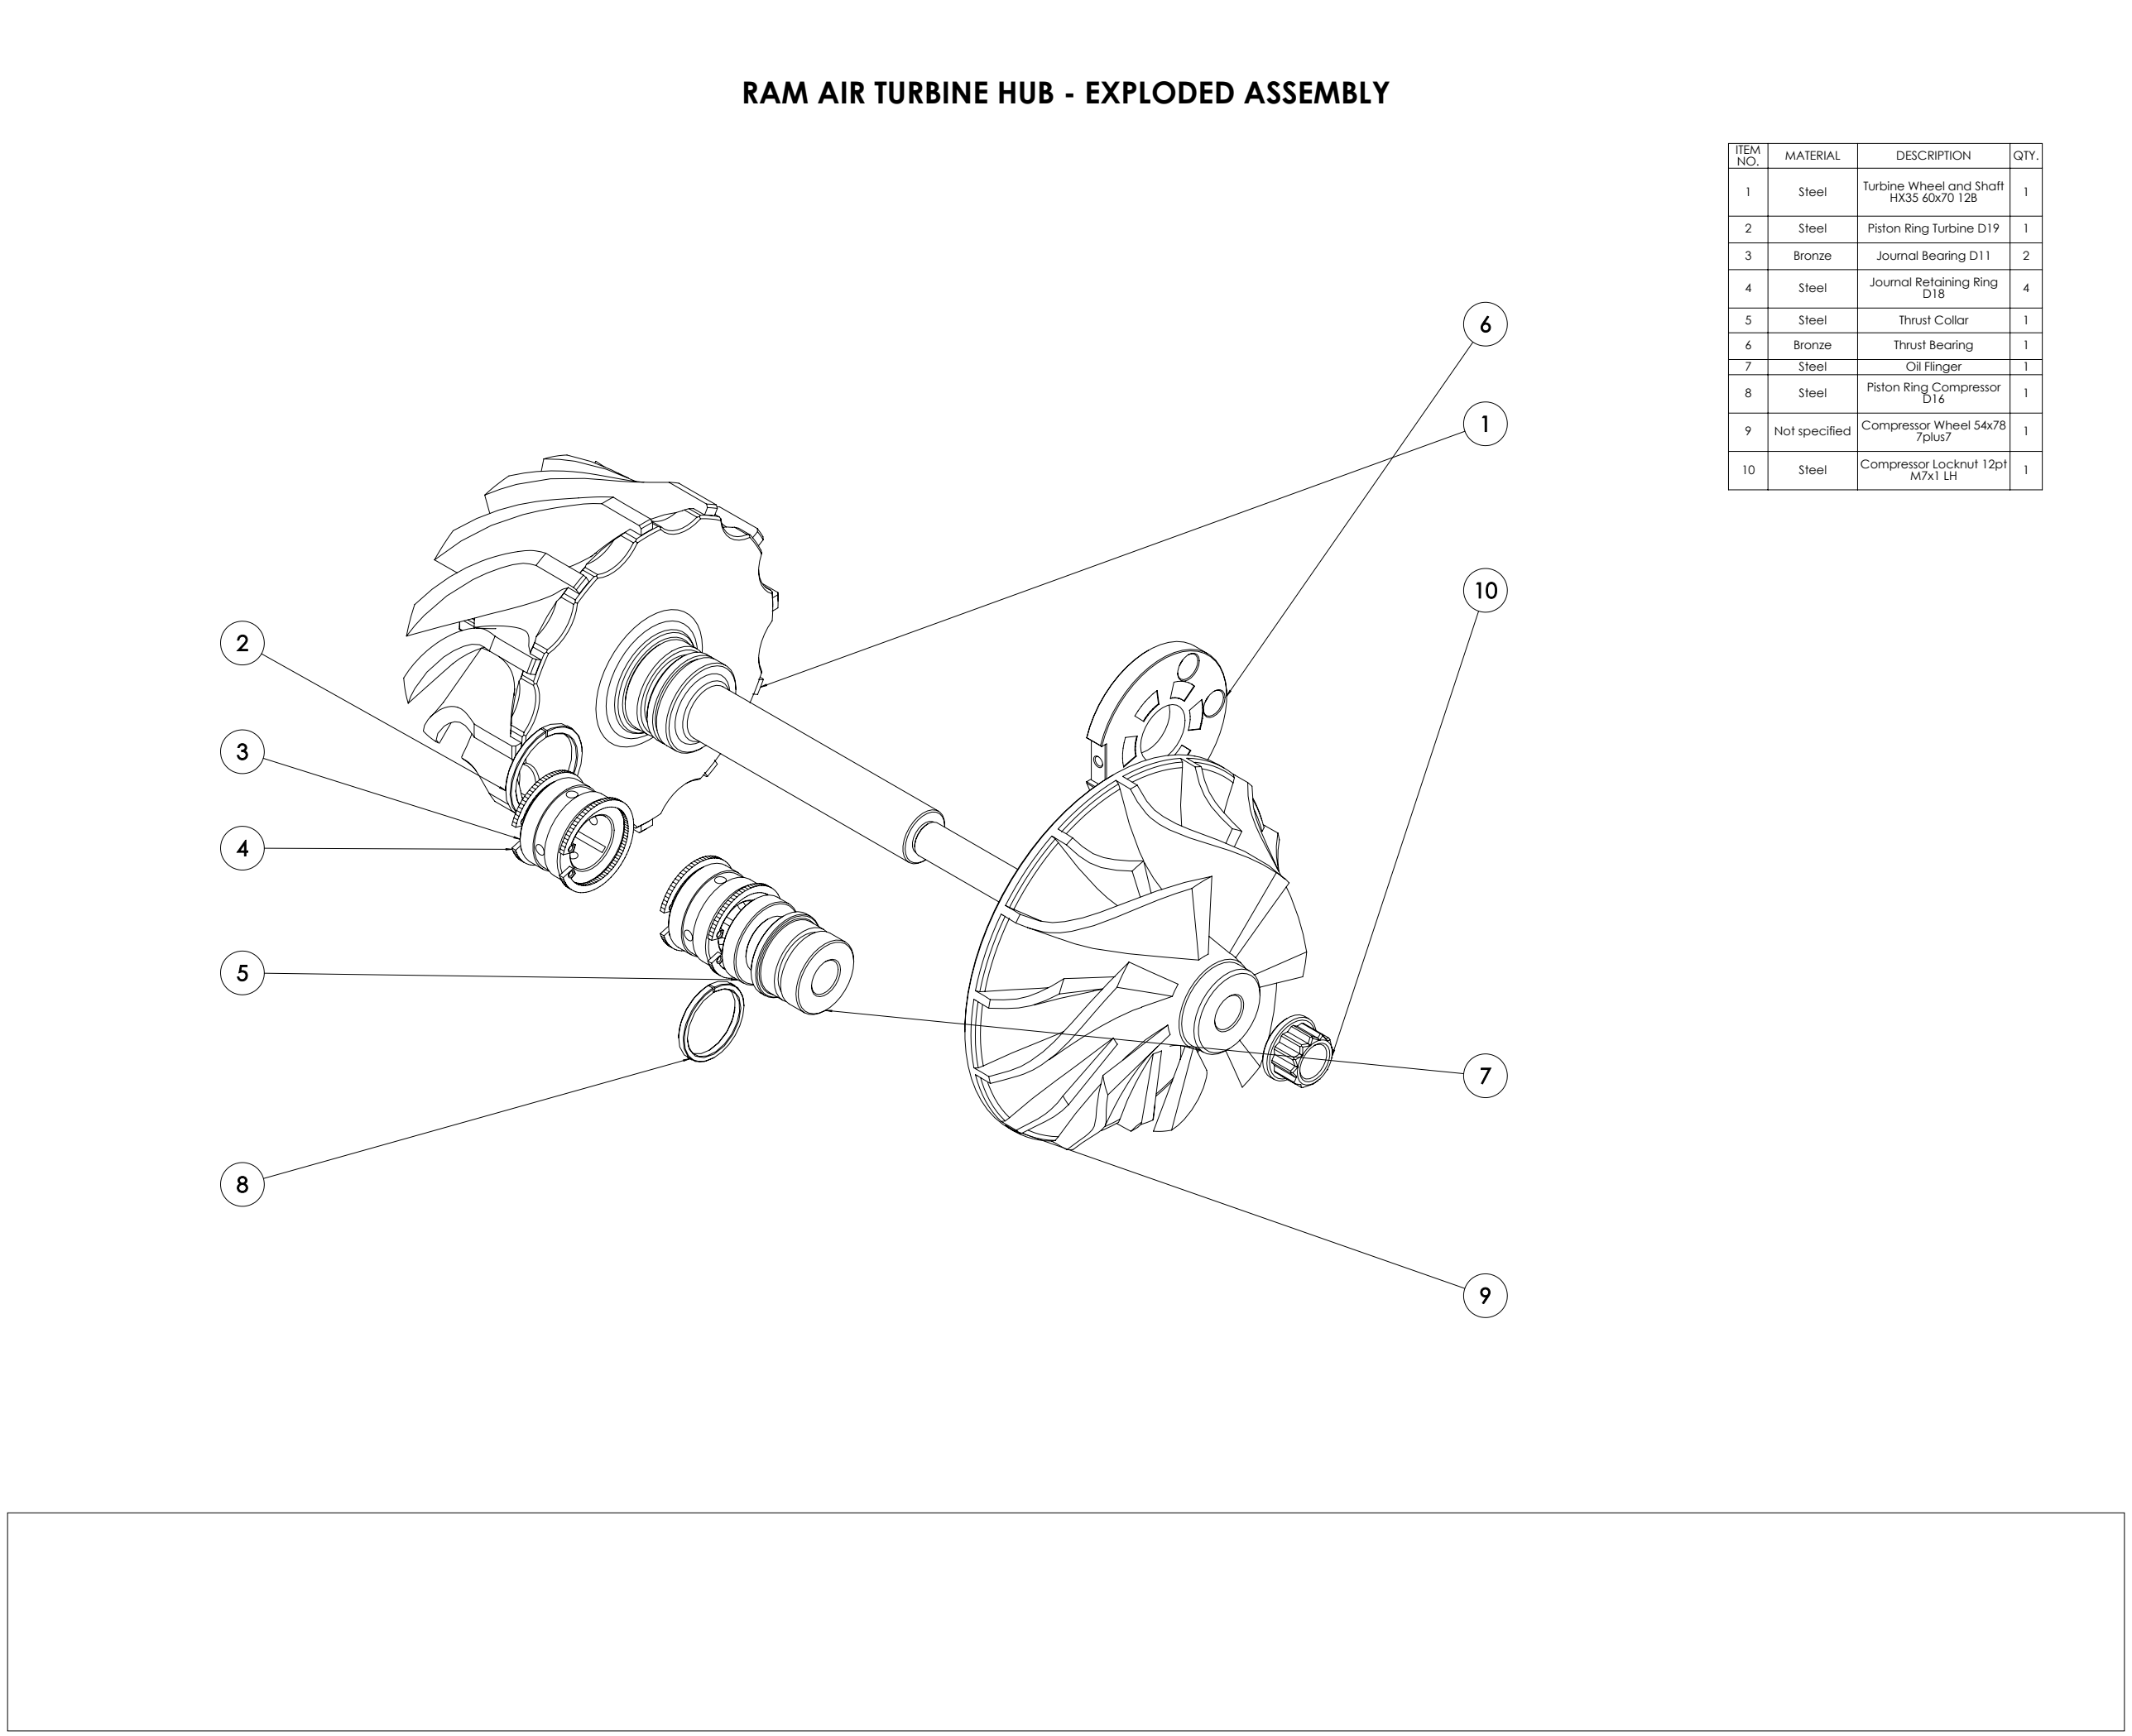
ISO-10303-21;
HEADER;
/* Generated by software containing ST-Developer
 * from STEP Tools, Inc. (www.steptools.com) 
 */

FILE_DESCRIPTION(
/* description */ (''),
/* implementation_level */ '2;1');

FILE_NAME(
/* name */ 'MAS-496',
/* time_stamp */ '2026-10-25T01:10:36-07:00',
/* author */ (''),
/* organization */ (''),
/* preprocessor_version */ 'ST-DEVELOPER v20.2',
/* originating_system */ 'Autodesk Translation Framework v15.15.0.0',
/* authorisation */ '');

FILE_SCHEMA (('AUTOMOTIVE_DESIGN { 1 0 10303 214 3 1 1 }'));
ENDSEC;

DATA;
#10=MECHANICAL_DESIGN_GEOMETRIC_PRESENTATION_REPRESENTATION('',(#1098,#1099,
#1100,#1101,#1102,#1103,#1104,#1105,#1106,#1107,#1108,#1109,#1110,#1111,
#1112,#1113,#1114,#1115,#1116,#1117,#1118,#1119,#1120,#1121,#1122,#1123,
#1124,#1125,#1126,#1127,#1128,#1129,#1130,#1131,#1132,#1133,#1134,#1135,
#1136,#1137,#1138,#1139,#1140,#1141,#1142,#1143,#1144,#1145,#1146,#1147,
#1148,#1149,#1150,#1151,#1152,#1153,#1154,#1155,#1156,#1157,#1158,#1159,
#1160,#1161,#1162,#1163,#1164,#1165,#1166,#1167,#1168,#1169,#1170,#1171,
#1172,#1173,#1174,#1175,#1176,#1177,#1178,#1179,#1180,#1181,#1182,#1183,
#1184,#1185,#1186,#1187,#1188,#1189,#1190,#1191,#1192,#1193,#1194,#1195,
#1196,#1197,#1198,#1199,#1200,#1201,#1202,#1203,#1204,#1205,#1206,#1207,
#1208,#1209,#1210,#1211,#1212,#1213,#1214,#1215,#1216,#1217,#1218,#1219,
#1220,#1221,#1222,#1223,#1224,#1225,#1226,#1227,#1228,#1229,#1230,#1231,
#1232,#1233,#1234,#1235,#1236,#1237,#1238,#1239,#1240,#1241,#1242,#1243,
#1244,#1245,#1246,#1247,#1248,#1249,#1250,#1251,#1252,#1253,#1254,#1255,
#1256,#1257,#1258,#1259,#1260,#1261,#1262,#1263,#1264,#1265,#1266,#1267,
#1268,#1269,#1270,#1271,#1272,#1273,#1274,#1275,#1276,#1277,#1278,#1279,
#1280,#1281,#1282,#1283,#1284,#1285,#1286,#1287,#1288,#1289,#1290,#1291,
#1292,#1293,#1294,#1295,#1296,#1297,#1298,#1299,#1300,#1301,#1302,#1303,
#1304),#60365);
#11=ITEM_DEFINED_TRANSFORMATION($,$,#18419,#19664);
#12=ITEM_DEFINED_TRANSFORMATION($,$,#18916,#19665);
#13=ITEM_DEFINED_TRANSFORMATION($,$,#18921,#19666);
#14=ITEM_DEFINED_TRANSFORMATION($,$,#18938,#19667);
#15=ITEM_DEFINED_TRANSFORMATION($,$,#19163,#19668);
#16=ITEM_DEFINED_TRANSFORMATION($,$,#19226,#19669);
#17=ITEM_DEFINED_TRANSFORMATION($,$,#19231,#19670);
#18=ITEM_DEFINED_TRANSFORMATION($,$,#19368,#19671);
#19=ITEM_DEFINED_TRANSFORMATION($,$,#19440,#19672);
#20=ITEM_DEFINED_TRANSFORMATION($,$,#19440,#19673);
#21=ITEM_DEFINED_TRANSFORMATION($,$,#19497,#19674);
#22=ITEM_DEFINED_TRANSFORMATION($,$,#19497,#19675);
#23=ITEM_DEFINED_TRANSFORMATION($,$,#19497,#19676);
#24=ITEM_DEFINED_TRANSFORMATION($,$,#19497,#19677);
#25=(
REPRESENTATION_RELATIONSHIP($,$,#60407,#60406)
REPRESENTATION_RELATIONSHIP_WITH_TRANSFORMATION(#11)
SHAPE_REPRESENTATION_RELATIONSHIP()
);
#26=(
REPRESENTATION_RELATIONSHIP($,$,#60408,#60406)
REPRESENTATION_RELATIONSHIP_WITH_TRANSFORMATION(#12)
SHAPE_REPRESENTATION_RELATIONSHIP()
);
#27=(
REPRESENTATION_RELATIONSHIP($,$,#60409,#60406)
REPRESENTATION_RELATIONSHIP_WITH_TRANSFORMATION(#13)
SHAPE_REPRESENTATION_RELATIONSHIP()
);
#28=(
REPRESENTATION_RELATIONSHIP($,$,#60410,#60406)
REPRESENTATION_RELATIONSHIP_WITH_TRANSFORMATION(#14)
SHAPE_REPRESENTATION_RELATIONSHIP()
);
#29=(
REPRESENTATION_RELATIONSHIP($,$,#60411,#60406)
REPRESENTATION_RELATIONSHIP_WITH_TRANSFORMATION(#15)
SHAPE_REPRESENTATION_RELATIONSHIP()
);
#30=(
REPRESENTATION_RELATIONSHIP($,$,#60412,#60406)
REPRESENTATION_RELATIONSHIP_WITH_TRANSFORMATION(#16)
SHAPE_REPRESENTATION_RELATIONSHIP()
);
#31=(
REPRESENTATION_RELATIONSHIP($,$,#60413,#60406)
REPRESENTATION_RELATIONSHIP_WITH_TRANSFORMATION(#17)
SHAPE_REPRESENTATION_RELATIONSHIP()
);
#32=(
REPRESENTATION_RELATIONSHIP($,$,#60414,#60406)
REPRESENTATION_RELATIONSHIP_WITH_TRANSFORMATION(#18)
SHAPE_REPRESENTATION_RELATIONSHIP()
);
#33=(
REPRESENTATION_RELATIONSHIP($,$,#60415,#60406)
REPRESENTATION_RELATIONSHIP_WITH_TRANSFORMATION(#19)
SHAPE_REPRESENTATION_RELATIONSHIP()
);
#34=(
REPRESENTATION_RELATIONSHIP($,$,#60415,#60406)
REPRESENTATION_RELATIONSHIP_WITH_TRANSFORMATION(#20)
SHAPE_REPRESENTATION_RELATIONSHIP()
);
#35=(
REPRESENTATION_RELATIONSHIP($,$,#60416,#60406)
REPRESENTATION_RELATIONSHIP_WITH_TRANSFORMATION(#21)
SHAPE_REPRESENTATION_RELATIONSHIP()
);
#36=(
REPRESENTATION_RELATIONSHIP($,$,#60416,#60406)
REPRESENTATION_RELATIONSHIP_WITH_TRANSFORMATION(#22)
SHAPE_REPRESENTATION_RELATIONSHIP()
);
#37=(
REPRESENTATION_RELATIONSHIP($,$,#60416,#60406)
REPRESENTATION_RELATIONSHIP_WITH_TRANSFORMATION(#23)
SHAPE_REPRESENTATION_RELATIONSHIP()
);
#38=(
REPRESENTATION_RELATIONSHIP($,$,#60416,#60406)
REPRESENTATION_RELATIONSHIP_WITH_TRANSFORMATION(#24)
SHAPE_REPRESENTATION_RELATIONSHIP()
);
#39=CONTEXT_DEPENDENT_SHAPE_REPRESENTATION(#25,#60392);
#40=CONTEXT_DEPENDENT_SHAPE_REPRESENTATION(#26,#60393);
#41=CONTEXT_DEPENDENT_SHAPE_REPRESENTATION(#27,#60394);
#42=CONTEXT_DEPENDENT_SHAPE_REPRESENTATION(#28,#60395);
#43=CONTEXT_DEPENDENT_SHAPE_REPRESENTATION(#29,#60396);
#44=CONTEXT_DEPENDENT_SHAPE_REPRESENTATION(#30,#60397);
#45=CONTEXT_DEPENDENT_SHAPE_REPRESENTATION(#31,#60398);
#46=CONTEXT_DEPENDENT_SHAPE_REPRESENTATION(#32,#60399);
#47=CONTEXT_DEPENDENT_SHAPE_REPRESENTATION(#33,#60400);
#48=CONTEXT_DEPENDENT_SHAPE_REPRESENTATION(#34,#60401);
#49=CONTEXT_DEPENDENT_SHAPE_REPRESENTATION(#35,#60402);
#50=CONTEXT_DEPENDENT_SHAPE_REPRESENTATION(#36,#60403);
#51=CONTEXT_DEPENDENT_SHAPE_REPRESENTATION(#37,#60404);
#52=CONTEXT_DEPENDENT_SHAPE_REPRESENTATION(#38,#60405);
#53=NEXT_ASSEMBLY_USAGE_OCCURRENCE(
'01_Turbine_Wheel_and_Shaft_HX35_60x70_12B:2',
'01_Turbine_Wheel_and_Shaft_HX35_60x70_12B:2',
'01_Turbine_Wheel_and_Shaft_HX35_60x70_12B:2',#60418,#60419,
'01_Turbine_Wheel_and_Shaft_HX35_60x70_12B:2');
#54=NEXT_ASSEMBLY_USAGE_OCCURRENCE('02_Piston_Ring_Turbine_D19:2',
'02_Piston_Ring_Turbine_D19:2','02_Piston_Ring_Turbine_D19:2',#60418,#60420,
'02_Piston_Ring_Turbine_D19:2');
#55=NEXT_ASSEMBLY_USAGE_OCCURRENCE('05_Thrust_Collar:2',
'05_Thrust_Collar:2','05_Thrust_Collar:2',#60418,#60421,
'05_Thrust_Collar:2');
#56=NEXT_ASSEMBLY_USAGE_OCCURRENCE('06_Thrust_Bearing:2',
'06_Thrust_Bearing:2','06_Thrust_Bearing:2',#60418,#60422,
'06_Thrust_Bearing:2');
#57=NEXT_ASSEMBLY_USAGE_OCCURRENCE('07_Oil_Flinger:2',
'07_Oil_Flinger:2','07_Oil_Flinger:2',#60418,#60423,'07_Oil_Flinger:2');
#58=NEXT_ASSEMBLY_USAGE_OCCURRENCE('08_Piston_Ring_Compressor_D16:2',
'08_Piston_Ring_Compressor_D16:2','08_Piston_Ring_Compressor_D16:2',#60418,
#60424,'08_Piston_Ring_Compressor_D16:2');
#59=NEXT_ASSEMBLY_USAGE_OCCURRENCE('09_Compressor_Wheel_54x78_7plus7:2',
'09_Compressor_Wheel_54x78_7plus7:2',
'09_Compressor_Wheel_54x78_7plus7:2',#60418,#60425,
'09_Compressor_Wheel_54x78_7plus7:2');
#60=NEXT_ASSEMBLY_USAGE_OCCURRENCE(
'10_Compressor_Locknut_12pt_M7x1_LH:2',
'10_Compressor_Locknut_12pt_M7x1_LH:2',
'10_Compressor_Locknut_12pt_M7x1_LH:2',#60418,#60426,
'10_Compressor_Locknut_12pt_M7x1_LH:2');
#61=NEXT_ASSEMBLY_USAGE_OCCURRENCE('03_Journal_Bearing_D11:2',
'03_Journal_Bearing_D11:2','03_Journal_Bearing_D11:2',#60418,#60427,
'03_Journal_Bearing_D11:2');
#62=NEXT_ASSEMBLY_USAGE_OCCURRENCE('03_Journal_Bearing_D11:3',
'03_Journal_Bearing_D11:3','03_Journal_Bearing_D11:3',#60418,#60427,
'03_Journal_Bearing_D11:3');
#63=NEXT_ASSEMBLY_USAGE_OCCURRENCE('04_Journal_Retaining_Ring_D18:2',
'04_Journal_Retaining_Ring_D18:2','04_Journal_Retaining_Ring_D18:2',#60418,
#60428,'04_Journal_Retaining_Ring_D18:2');
#64=NEXT_ASSEMBLY_USAGE_OCCURRENCE('04_Journal_Retaining_Ring_D18:3',
'04_Journal_Retaining_Ring_D18:3','04_Journal_Retaining_Ring_D18:3',#60418,
#60428,'04_Journal_Retaining_Ring_D18:3');
#65=NEXT_ASSEMBLY_USAGE_OCCURRENCE('04_Journal_Retaining_Ring_D18:4',
'04_Journal_Retaining_Ring_D18:4','04_Journal_Retaining_Ring_D18:4',#60418,
#60428,'04_Journal_Retaining_Ring_D18:4');
#66=NEXT_ASSEMBLY_USAGE_OCCURRENCE('04_Journal_Retaining_Ring_D18:5',
'04_Journal_Retaining_Ring_D18:5','04_Journal_Retaining_Ring_D18:5',#60418,
#60428,'04_Journal_Retaining_Ring_D18:5');
#67=SHAPE_REPRESENTATION_RELATIONSHIP('SRR','None',#60407,#77);
#68=SHAPE_REPRESENTATION_RELATIONSHIP('SRR','None',#60408,#78);
#69=SHAPE_REPRESENTATION_RELATIONSHIP('SRR','None',#60409,#79);
#70=SHAPE_REPRESENTATION_RELATIONSHIP('SRR','None',#60410,#80);
#71=SHAPE_REPRESENTATION_RELATIONSHIP('SRR','None',#60411,#81);
#72=SHAPE_REPRESENTATION_RELATIONSHIP('SRR','None',#60412,#82);
#73=SHAPE_REPRESENTATION_RELATIONSHIP('SRR','None',#60413,#83);
#74=SHAPE_REPRESENTATION_RELATIONSHIP('SRR','None',#60414,#84);
#75=SHAPE_REPRESENTATION_RELATIONSHIP('SRR','None',#60415,#85);
#76=SHAPE_REPRESENTATION_RELATIONSHIP('SRR','None',#60416,#86);
#77=ADVANCED_BREP_SHAPE_REPRESENTATION('',(#87),#60355);
#78=ADVANCED_BREP_SHAPE_REPRESENTATION('',(#88),#60356);
#79=ADVANCED_BREP_SHAPE_REPRESENTATION('',(#89),#60357);
#80=ADVANCED_BREP_SHAPE_REPRESENTATION('',(#90),#60358);
#81=ADVANCED_BREP_SHAPE_REPRESENTATION('',(#91),#60359);
#82=ADVANCED_BREP_SHAPE_REPRESENTATION('',(#92),#60360);
#83=ADVANCED_BREP_SHAPE_REPRESENTATION('',(#93),#60361);
#84=ADVANCED_BREP_SHAPE_REPRESENTATION('',(#94),#60362);
#85=ADVANCED_BREP_SHAPE_REPRESENTATION('',(#95),#60363);
#86=ADVANCED_BREP_SHAPE_REPRESENTATION('',(#96),#60364);
#87=MANIFOLD_SOLID_BREP('Body1',#18297);
#88=MANIFOLD_SOLID_BREP('Body1',#18298);
#89=MANIFOLD_SOLID_BREP('Body1',#18299);
#90=MANIFOLD_SOLID_BREP('Body1',#18300);
#91=MANIFOLD_SOLID_BREP('Body1',#18301);
#92=MANIFOLD_SOLID_BREP('Body1',#18302);
#93=MANIFOLD_SOLID_BREP('Body1',#18303);
#94=MANIFOLD_SOLID_BREP('Body1',#18304);
#95=MANIFOLD_SOLID_BREP('Body1',#18305);
#96=MANIFOLD_SOLID_BREP('Body1',#18306);
#97=B_SPLINE_SURFACE_WITH_KNOTS('',3,3,((#27482,#27483,#27484,#27485,#27486,
#27487,#27488,#27489,#27490,#27491,#27492,#27493,#27494,#27495,#27496,#27497,
#27498,#27499,#27500,#27501,#27502,#27503,#27504,#27505,#27506,#27507,#27508,
#27509,#27510,#27511,#27512,#27513,#27514,#27515,#27516,#27517,#27518,#27519,
#27520,#27521,#27522,#27523),(#27524,#27525,#27526,#27527,#27528,#27529,
#27530,#27531,#27532,#27533,#27534,#27535,#27536,#27537,#27538,#27539,#27540,
#27541,#27542,#27543,#27544,#27545,#27546,#27547,#27548,#27549,#27550,#27551,
#27552,#27553,#27554,#27555,#27556,#27557,#27558,#27559,#27560,#27561,#27562,
#27563,#27564,#27565),(#27566,#27567,#27568,#27569,#27570,#27571,#27572,
#27573,#27574,#27575,#27576,#27577,#27578,#27579,#27580,#27581,#27582,#27583,
#27584,#27585,#27586,#27587,#27588,#27589,#27590,#27591,#27592,#27593,#27594,
#27595,#27596,#27597,#27598,#27599,#27600,#27601,#27602,#27603,#27604,#27605,
#27606,#27607),(#27608,#27609,#27610,#27611,#27612,#27613,#27614,#27615,
#27616,#27617,#27618,#27619,#27620,#27621,#27622,#27623,#27624,#27625,#27626,
#27627,#27628,#27629,#27630,#27631,#27632,#27633,#27634,#27635,#27636,#27637,
#27638,#27639,#27640,#27641,#27642,#27643,#27644,#27645,#27646,#27647,#27648,
#27649),(#27650,#27651,#27652,#27653,#27654,#27655,#27656,#27657,#27658,
#27659,#27660,#27661,#27662,#27663,#27664,#27665,#27666,#27667,#27668,#27669,
#27670,#27671,#27672,#27673,#27674,#27675,#27676,#27677,#27678,#27679,#27680,
#27681,#27682,#27683,#27684,#27685,#27686,#27687,#27688,#27689,#27690,#27691)),
 .UNSPECIFIED.,.F.,.F.,.F.,(4,1,4),(4,2,2,2,2,2,1,1,2,1,1,1,1,1,1,2,1,2,
1,1,1,1,2,1,1,1,1,1,1,1,4),(0.10381731230502,0.585202227283102,0.946240913516665),
(0.0903575719412648,0.100793262783688,0.212043315812054,0.313257792411489,
0.405143101782566,0.488664067632647,0.50778607271066,0.526908077788674,
0.565152087944702,0.574062129417373,0.582972170890044,0.600792253835385,
0.618612336780727,0.627522378253398,0.631977398989734,0.636432419726069,
0.66210667165326,0.704897091531912,0.716247203396069,0.727597315260226,
0.736109899158344,0.750297538988541,0.79569798644517,0.806906221911025,
0.815312398510416,0.81811445737688,0.840530928308591,0.851739163774446,
0.874155634706157,0.885363870172012,0.975029753898854),.UNSPECIFIED.);
#98=B_SPLINE_SURFACE_WITH_KNOTS('',3,3,((#27985,#27986,#27987,#27988,#27989,
#27990,#27991,#27992,#27993,#27994,#27995,#27996,#27997,#27998,#27999,#28000,
#28001,#28002,#28003,#28004,#28005,#28006,#28007,#28008,#28009,#28010,#28011,
#28012,#28013,#28014,#28015,#28016,#28017,#28018,#28019,#28020,#28021,#28022),
(#28023,#28024,#28025,#28026,#28027,#28028,#28029,#28030,#28031,#28032,
#28033,#28034,#28035,#28036,#28037,#28038,#28039,#28040,#28041,#28042,#28043,
#28044,#28045,#28046,#28047,#28048,#28049,#28050,#28051,#28052,#28053,#28054,
#28055,#28056,#28057,#28058,#28059,#28060),(#28061,#28062,#28063,#28064,
#28065,#28066,#28067,#28068,#28069,#28070,#28071,#28072,#28073,#28074,#28075,
#28076,#28077,#28078,#28079,#28080,#28081,#28082,#28083,#28084,#28085,#28086,
#28087,#28088,#28089,#28090,#28091,#28092,#28093,#28094,#28095,#28096,#28097,
#28098),(#28099,#28100,#28101,#28102,#28103,#28104,#28105,#28106,#28107,
#28108,#28109,#28110,#28111,#28112,#28113,#28114,#28115,#28116,#28117,#28118,
#28119,#28120,#28121,#28122,#28123,#28124,#28125,#28126,#28127,#28128,#28129,
#28130,#28131,#28132,#28133,#28134,#28135,#28136),(#28137,#28138,#28139,
#28140,#28141,#28142,#28143,#28144,#28145,#28146,#28147,#28148,#28149,#28150,
#28151,#28152,#28153,#28154,#28155,#28156,#28157,#28158,#28159,#28160,#28161,
#28162,#28163,#28164,#28165,#28166,#28167,#28168,#28169,#28170,#28171,#28172,
#28173,#28174)),.UNSPECIFIED.,.F.,.F.,.F.,(4,1,4),(4,2,2,2,2,2,1,1,2,1,
1,1,1,1,2,1,2,1,1,1,2,1,1,1,1,1,4),(0.10381731230502,0.464855998538582,
0.946240913516665),(0.0903575719412648,0.100793262783688,0.212043315812054,
0.313257792411489,0.405143101782566,0.488664067632647,0.50778607271066,
0.526908077788674,0.565152087944702,0.574062129417373,0.582972170890044,
0.600792253835385,0.609702295308056,0.618612336780727,0.636432419726069,
0.65354858767753,0.704897091531912,0.716247203396069,0.727597315260226,
0.750297538988541,0.79569798644517,0.806906221911025,0.81811445737688,0.840530928308591,
0.862947399240301,0.885363870172012,0.975029753898854),.UNSPECIFIED.);
#99=B_SPLINE_SURFACE_WITH_KNOTS('',3,3,((#28427,#28428,#28429,#28430,#28431,
#28432,#28433,#28434,#28435,#28436,#28437,#28438,#28439,#28440,#28441,#28442,
#28443,#28444,#28445,#28446,#28447,#28448,#28449,#28450,#28451,#28452,#28453,
#28454,#28455,#28456,#28457,#28458,#28459,#28460,#28461,#28462,#28463,#28464,
#28465,#28466,#28467,#28468,#28469,#28470),(#28471,#28472,#28473,#28474,
#28475,#28476,#28477,#28478,#28479,#28480,#28481,#28482,#28483,#28484,#28485,
#28486,#28487,#28488,#28489,#28490,#28491,#28492,#28493,#28494,#28495,#28496,
#28497,#28498,#28499,#28500,#28501,#28502,#28503,#28504,#28505,#28506,#28507,
#28508,#28509,#28510,#28511,#28512,#28513,#28514),(#28515,#28516,#28517,
#28518,#28519,#28520,#28521,#28522,#28523,#28524,#28525,#28526,#28527,#28528,
#28529,#28530,#28531,#28532,#28533,#28534,#28535,#28536,#28537,#28538,#28539,
#28540,#28541,#28542,#28543,#28544,#28545,#28546,#28547,#28548,#28549,#28550,
#28551,#28552,#28553,#28554,#28555,#28556,#28557,#28558),(#28559,#28560,
#28561,#28562,#28563,#28564,#28565,#28566,#28567,#28568,#28569,#28570,#28571,
#28572,#28573,#28574,#28575,#28576,#28577,#28578,#28579,#28580,#28581,#28582,
#28583,#28584,#28585,#28586,#28587,#28588,#28589,#28590,#28591,#28592,#28593,
#28594,#28595,#28596,#28597,#28598,#28599,#28600,#28601,#28602),(#28603,
#28604,#28605,#28606,#28607,#28608,#28609,#28610,#28611,#28612,#28613,#28614,
#28615,#28616,#28617,#28618,#28619,#28620,#28621,#28622,#28623,#28624,#28625,
#28626,#28627,#28628,#28629,#28630,#28631,#28632,#28633,#28634,#28635,#28636,
#28637,#28638,#28639,#28640,#28641,#28642,#28643,#28644,#28645,#28646)),
 .UNSPECIFIED.,.F.,.F.,.F.,(4,1,4),(4,2,2,2,2,2,1,1,1,2,1,1,1,1,1,1,1,2,
1,2,1,1,1,1,1,2,1,1,1,1,1,1,4),(0.10381731230502,0.464855998538582,0.946240913516665),
(0.0903575719412648,0.100793262783688,0.212043315812054,0.313257792411489,
0.405143101782566,0.488664067632647,0.50778607271066,0.526908077788674,
0.546030082866688,0.565152087944702,0.574062129417373,0.582972170890044,
0.600792253835385,0.609702295308056,0.618612336780727,0.627522378253398,
0.631977398989734,0.636432419726069,0.670664755628991,0.704897091531912,
0.71057214746399,0.716247203396069,0.727597315260226,0.738947427124383,
0.750297538988541,0.79569798644517,0.806906221911025,0.81811445737688,0.829322692842735,
0.840530928308591,0.862947399240301,0.885363870172012,0.975029753898854),
 .UNSPECIFIED.);
#100=B_SPLINE_SURFACE_WITH_KNOTS('',3,3,((#28899,#28900,#28901,#28902,#28903,
#28904,#28905,#28906,#28907,#28908,#28909,#28910,#28911,#28912,#28913,#28914,
#28915,#28916,#28917,#28918,#28919,#28920,#28921,#28922,#28923,#28924,#28925,
#28926,#28927,#28928,#28929,#28930,#28931,#28932,#28933,#28934,#28935,#28936,
#28937,#28938,#28939,#28940),(#28941,#28942,#28943,#28944,#28945,#28946,
#28947,#28948,#28949,#28950,#28951,#28952,#28953,#28954,#28955,#28956,#28957,
#28958,#28959,#28960,#28961,#28962,#28963,#28964,#28965,#28966,#28967,#28968,
#28969,#28970,#28971,#28972,#28973,#28974,#28975,#28976,#28977,#28978,#28979,
#28980,#28981,#28982),(#28983,#28984,#28985,#28986,#28987,#28988,#28989,
#28990,#28991,#28992,#28993,#28994,#28995,#28996,#28997,#28998,#28999,#29000,
#29001,#29002,#29003,#29004,#29005,#29006,#29007,#29008,#29009,#29010,#29011,
#29012,#29013,#29014,#29015,#29016,#29017,#29018,#29019,#29020,#29021,#29022,
#29023,#29024),(#29025,#29026,#29027,#29028,#29029,#29030,#29031,#29032,
#29033,#29034,#29035,#29036,#29037,#29038,#29039,#29040,#29041,#29042,#29043,
#29044,#29045,#29046,#29047,#29048,#29049,#29050,#29051,#29052,#29053,#29054,
#29055,#29056,#29057,#29058,#29059,#29060,#29061,#29062,#29063,#29064,#29065,
#29066),(#29067,#29068,#29069,#29070,#29071,#29072,#29073,#29074,#29075,
#29076,#29077,#29078,#29079,#29080,#29081,#29082,#29083,#29084,#29085,#29086,
#29087,#29088,#29089,#29090,#29091,#29092,#29093,#29094,#29095,#29096,#29097,
#29098,#29099,#29100,#29101,#29102,#29103,#29104,#29105,#29106,#29107,#29108)),
 .UNSPECIFIED.,.F.,.F.,.F.,(4,1,4),(4,2,2,2,2,2,1,1,2,1,1,1,1,1,1,2,1,2,
1,1,1,1,2,1,1,1,1,1,1,1,4),(0.10381731230502,0.585202227283103,0.946240913516665),
(0.0903575719412648,0.100793262783688,0.212043315812054,0.313257792411489,
0.405143101782566,0.488664067632647,0.50778607271066,0.526908077788674,
0.565152087944702,0.574062129417373,0.582972170890044,0.600792253835385,
0.618612336780727,0.627522378253398,0.631977398989734,0.636432419726069,
0.66210667165326,0.704897091531912,0.716247203396069,0.727597315260226,
0.736109899158344,0.750297538988541,0.79569798644517,0.806906221911025,
0.815312398510416,0.81811445737688,0.840530928308591,0.851739163774446,
0.874155634706157,0.885363870172012,0.975029753898854),.UNSPECIFIED.);
#101=B_SPLINE_SURFACE_WITH_KNOTS('',3,3,((#29355,#29356,#29357,#29358,#29359,
#29360,#29361,#29362,#29363,#29364,#29365,#29366,#29367,#29368,#29369,#29370,
#29371,#29372,#29373,#29374,#29375,#29376,#29377,#29378,#29379,#29380,#29381,
#29382,#29383,#29384,#29385,#29386,#29387,#29388,#29389,#29390,#29391,#29392),
(#29393,#29394,#29395,#29396,#29397,#29398,#29399,#29400,#29401,#29402,
#29403,#29404,#29405,#29406,#29407,#29408,#29409,#29410,#29411,#29412,#29413,
#29414,#29415,#29416,#29417,#29418,#29419,#29420,#29421,#29422,#29423,#29424,
#29425,#29426,#29427,#29428,#29429,#29430),(#29431,#29432,#29433,#29434,
#29435,#29436,#29437,#29438,#29439,#29440,#29441,#29442,#29443,#29444,#29445,
#29446,#29447,#29448,#29449,#29450,#29451,#29452,#29453,#29454,#29455,#29456,
#29457,#29458,#29459,#29460,#29461,#29462,#29463,#29464,#29465,#29466,#29467,
#29468),(#29469,#29470,#29471,#29472,#29473,#29474,#29475,#29476,#29477,
#29478,#29479,#29480,#29481,#29482,#29483,#29484,#29485,#29486,#29487,#29488,
#29489,#29490,#29491,#29492,#29493,#29494,#29495,#29496,#29497,#29498,#29499,
#29500,#29501,#29502,#29503,#29504,#29505,#29506),(#29507,#29508,#29509,
#29510,#29511,#29512,#29513,#29514,#29515,#29516,#29517,#29518,#29519,#29520,
#29521,#29522,#29523,#29524,#29525,#29526,#29527,#29528,#29529,#29530,#29531,
#29532,#29533,#29534,#29535,#29536,#29537,#29538,#29539,#29540,#29541,#29542,
#29543,#29544)),.UNSPECIFIED.,.F.,.F.,.F.,(4,1,4),(4,2,2,2,2,2,1,1,2,1,
1,1,1,1,2,1,2,1,1,1,2,1,1,1,1,1,4),(0.10381731230502,0.464855998538582,
0.946240913516665),(0.0903575719412648,0.100793262783688,0.212043315812054,
0.313257792411489,0.405143101782566,0.488664067632647,0.50778607271066,
0.526908077788674,0.565152087944702,0.574062129417373,0.582972170890044,
0.600792253835385,0.609702295308056,0.618612336780727,0.636432419726069,
0.65354858767753,0.704897091531912,0.716247203396069,0.727597315260226,
0.750297538988541,0.79569798644517,0.806906221911025,0.81811445737688,0.840530928308591,
0.862947399240301,0.885363870172012,0.975029753898854),.UNSPECIFIED.);
#102=B_SPLINE_SURFACE_WITH_KNOTS('',3,3,((#29797,#29798,#29799,#29800,#29801,
#29802,#29803,#29804,#29805,#29806,#29807,#29808,#29809,#29810,#29811,#29812,
#29813,#29814,#29815,#29816,#29817,#29818,#29819,#29820,#29821,#29822,#29823,
#29824,#29825,#29826,#29827,#29828,#29829,#29830,#29831,#29832,#29833,#29834,
#29835,#29836,#29837,#29838,#29839,#29840),(#29841,#29842,#29843,#29844,
#29845,#29846,#29847,#29848,#29849,#29850,#29851,#29852,#29853,#29854,#29855,
#29856,#29857,#29858,#29859,#29860,#29861,#29862,#29863,#29864,#29865,#29866,
#29867,#29868,#29869,#29870,#29871,#29872,#29873,#29874,#29875,#29876,#29877,
#29878,#29879,#29880,#29881,#29882,#29883,#29884),(#29885,#29886,#29887,
#29888,#29889,#29890,#29891,#29892,#29893,#29894,#29895,#29896,#29897,#29898,
#29899,#29900,#29901,#29902,#29903,#29904,#29905,#29906,#29907,#29908,#29909,
#29910,#29911,#29912,#29913,#29914,#29915,#29916,#29917,#29918,#29919,#29920,
#29921,#29922,#29923,#29924,#29925,#29926,#29927,#29928),(#29929,#29930,
#29931,#29932,#29933,#29934,#29935,#29936,#29937,#29938,#29939,#29940,#29941,
#29942,#29943,#29944,#29945,#29946,#29947,#29948,#29949,#29950,#29951,#29952,
#29953,#29954,#29955,#29956,#29957,#29958,#29959,#29960,#29961,#29962,#29963,
#29964,#29965,#29966,#29967,#29968,#29969,#29970,#29971,#29972),(#29973,
#29974,#29975,#29976,#29977,#29978,#29979,#29980,#29981,#29982,#29983,#29984,
#29985,#29986,#29987,#29988,#29989,#29990,#29991,#29992,#29993,#29994,#29995,
#29996,#29997,#29998,#29999,#30000,#30001,#30002,#30003,#30004,#30005,#30006,
#30007,#30008,#30009,#30010,#30011,#30012,#30013,#30014,#30015,#30016)),
 .UNSPECIFIED.,.F.,.F.,.F.,(4,1,4),(4,2,2,2,2,2,1,1,1,2,1,1,1,1,1,1,1,2,
1,2,1,1,1,1,1,2,1,1,1,1,1,1,4),(0.10381731230502,0.585202227283102,0.946240913516665),
(0.0903575719412648,0.100793262783688,0.212043315812054,0.313257792411489,
0.405143101782566,0.488664067632647,0.50778607271066,0.526908077788674,
0.546030082866688,0.565152087944702,0.574062129417373,0.582972170890044,
0.600792253835385,0.609702295308056,0.618612336780727,0.627522378253398,
0.631977398989734,0.636432419726069,0.670664755628991,0.704897091531912,
0.71057214746399,0.716247203396069,0.727597315260226,0.738947427124383,
0.750297538988541,0.79569798644517,0.806906221911025,0.81811445737688,0.829322692842735,
0.840530928308591,0.862947399240301,0.885363870172012,0.975029753898854),
 .UNSPECIFIED.);
#103=B_SPLINE_SURFACE_WITH_KNOTS('',3,3,((#30269,#30270,#30271,#30272,#30273,
#30274,#30275,#30276,#30277,#30278,#30279,#30280,#30281,#30282,#30283,#30284,
#30285,#30286,#30287,#30288,#30289,#30290,#30291,#30292,#30293,#30294,#30295,
#30296,#30297,#30298,#30299,#30300,#30301,#30302,#30303,#30304,#30305,#30306,
#30307,#30308,#30309,#30310),(#30311,#30312,#30313,#30314,#30315,#30316,
#30317,#30318,#30319,#30320,#30321,#30322,#30323,#30324,#30325,#30326,#30327,
#30328,#30329,#30330,#30331,#30332,#30333,#30334,#30335,#30336,#30337,#30338,
#30339,#30340,#30341,#30342,#30343,#30344,#30345,#30346,#30347,#30348,#30349,
#30350,#30351,#30352),(#30353,#30354,#30355,#30356,#30357,#30358,#30359,
#30360,#30361,#30362,#30363,#30364,#30365,#30366,#30367,#30368,#30369,#30370,
#30371,#30372,#30373,#30374,#30375,#30376,#30377,#30378,#30379,#30380,#30381,
#30382,#30383,#30384,#30385,#30386,#30387,#30388,#30389,#30390,#30391,#30392,
#30393,#30394),(#30395,#30396,#30397,#30398,#30399,#30400,#30401,#30402,
#30403,#30404,#30405,#30406,#30407,#30408,#30409,#30410,#30411,#30412,#30413,
#30414,#30415,#30416,#30417,#30418,#30419,#30420,#30421,#30422,#30423,#30424,
#30425,#30426,#30427,#30428,#30429,#30430,#30431,#30432,#30433,#30434,#30435,
#30436),(#30437,#30438,#30439,#30440,#30441,#30442,#30443,#30444,#30445,
#30446,#30447,#30448,#30449,#30450,#30451,#30452,#30453,#30454,#30455,#30456,
#30457,#30458,#30459,#30460,#30461,#30462,#30463,#30464,#30465,#30466,#30467,
#30468,#30469,#30470,#30471,#30472,#30473,#30474,#30475,#30476,#30477,#30478)),
 .UNSPECIFIED.,.F.,.F.,.F.,(4,1,4),(4,2,2,2,2,2,1,1,2,1,1,1,1,1,1,2,1,2,
1,1,1,1,2,1,1,1,1,1,1,1,4),(0.10381731230502,0.585202227283102,0.946240913516665),
(0.0903575719412648,0.100793262783688,0.212043315812054,0.313257792411489,
0.405143101782566,0.488664067632647,0.50778607271066,0.526908077788674,
0.565152087944702,0.574062129417373,0.582972170890044,0.600792253835385,
0.618612336780727,0.627522378253398,0.631977398989734,0.636432419726069,
0.66210667165326,0.704897091531912,0.716247203396069,0.727597315260226,
0.736109899158344,0.750297538988541,0.79569798644517,0.806906221911025,
0.815312398510416,0.81811445737688,0.840530928308591,0.851739163774446,
0.874155634706157,0.885363870172012,0.975029753898854),.UNSPECIFIED.);
#104=B_SPLINE_SURFACE_WITH_KNOTS('',3,3,((#30725,#30726,#30727,#30728,#30729,
#30730,#30731,#30732,#30733,#30734,#30735,#30736,#30737,#30738,#30739,#30740,
#30741,#30742,#30743,#30744,#30745,#30746,#30747,#30748,#30749,#30750,#30751,
#30752,#30753,#30754,#30755,#30756,#30757,#30758,#30759,#30760,#30761,#30762),
(#30763,#30764,#30765,#30766,#30767,#30768,#30769,#30770,#30771,#30772,
#30773,#30774,#30775,#30776,#30777,#30778,#30779,#30780,#30781,#30782,#30783,
#30784,#30785,#30786,#30787,#30788,#30789,#30790,#30791,#30792,#30793,#30794,
#30795,#30796,#30797,#30798,#30799,#30800),(#30801,#30802,#30803,#30804,
#30805,#30806,#30807,#30808,#30809,#30810,#30811,#30812,#30813,#30814,#30815,
#30816,#30817,#30818,#30819,#30820,#30821,#30822,#30823,#30824,#30825,#30826,
#30827,#30828,#30829,#30830,#30831,#30832,#30833,#30834,#30835,#30836,#30837,
#30838),(#30839,#30840,#30841,#30842,#30843,#30844,#30845,#30846,#30847,
#30848,#30849,#30850,#30851,#30852,#30853,#30854,#30855,#30856,#30857,#30858,
#30859,#30860,#30861,#30862,#30863,#30864,#30865,#30866,#30867,#30868,#30869,
#30870,#30871,#30872,#30873,#30874,#30875,#30876),(#30877,#30878,#30879,
#30880,#30881,#30882,#30883,#30884,#30885,#30886,#30887,#30888,#30889,#30890,
#30891,#30892,#30893,#30894,#30895,#30896,#30897,#30898,#30899,#30900,#30901,
#30902,#30903,#30904,#30905,#30906,#30907,#30908,#30909,#30910,#30911,#30912,
#30913,#30914)),.UNSPECIFIED.,.F.,.F.,.F.,(4,1,4),(4,2,2,2,2,2,1,1,2,1,
1,1,1,1,2,1,2,1,1,1,2,1,1,1,1,1,4),(0.10381731230502,0.464855998538582,
0.946240913516665),(0.0903575719412648,0.100793262783688,0.212043315812054,
0.313257792411489,0.405143101782566,0.488664067632647,0.50778607271066,
0.526908077788674,0.565152087944702,0.574062129417373,0.582972170890044,
0.600792253835385,0.609702295308056,0.618612336780727,0.636432419726069,
0.65354858767753,0.704897091531912,0.716247203396069,0.727597315260226,
0.750297538988541,0.79569798644517,0.806906221911025,0.81811445737688,0.840530928308591,
0.862947399240301,0.885363870172012,0.975029753898854),.UNSPECIFIED.);
#105=B_SPLINE_SURFACE_WITH_KNOTS('',3,3,((#31167,#31168,#31169,#31170,#31171,
#31172,#31173,#31174,#31175,#31176,#31177,#31178,#31179,#31180,#31181,#31182,
#31183,#31184,#31185,#31186,#31187,#31188,#31189,#31190,#31191,#31192,#31193,
#31194,#31195,#31196,#31197,#31198,#31199,#31200,#31201,#31202,#31203,#31204,
#31205,#31206,#31207,#31208,#31209,#31210),(#31211,#31212,#31213,#31214,
#31215,#31216,#31217,#31218,#31219,#31220,#31221,#31222,#31223,#31224,#31225,
#31226,#31227,#31228,#31229,#31230,#31231,#31232,#31233,#31234,#31235,#31236,
#31237,#31238,#31239,#31240,#31241,#31242,#31243,#31244,#31245,#31246,#31247,
#31248,#31249,#31250,#31251,#31252,#31253,#31254),(#31255,#31256,#31257,
#31258,#31259,#31260,#31261,#31262,#31263,#31264,#31265,#31266,#31267,#31268,
#31269,#31270,#31271,#31272,#31273,#31274,#31275,#31276,#31277,#31278,#31279,
#31280,#31281,#31282,#31283,#31284,#31285,#31286,#31287,#31288,#31289,#31290,
#31291,#31292,#31293,#31294,#31295,#31296,#31297,#31298),(#31299,#31300,
#31301,#31302,#31303,#31304,#31305,#31306,#31307,#31308,#31309,#31310,#31311,
#31312,#31313,#31314,#31315,#31316,#31317,#31318,#31319,#31320,#31321,#31322,
#31323,#31324,#31325,#31326,#31327,#31328,#31329,#31330,#31331,#31332,#31333,
#31334,#31335,#31336,#31337,#31338,#31339,#31340,#31341,#31342),(#31343,
#31344,#31345,#31346,#31347,#31348,#31349,#31350,#31351,#31352,#31353,#31354,
#31355,#31356,#31357,#31358,#31359,#31360,#31361,#31362,#31363,#31364,#31365,
#31366,#31367,#31368,#31369,#31370,#31371,#31372,#31373,#31374,#31375,#31376,
#31377,#31378,#31379,#31380,#31381,#31382,#31383,#31384,#31385,#31386)),
 .UNSPECIFIED.,.F.,.F.,.F.,(4,1,4),(4,2,2,2,2,2,1,1,1,2,1,1,1,1,1,1,1,2,
1,2,1,1,1,1,1,2,1,1,1,1,1,1,4),(0.10381731230502,0.464855998538582,0.946240913516665),
(0.0903575719412648,0.100793262783688,0.212043315812054,0.313257792411489,
0.405143101782566,0.488664067632647,0.50778607271066,0.526908077788674,
0.546030082866688,0.565152087944702,0.574062129417373,0.582972170890044,
0.600792253835385,0.609702295308056,0.618612336780727,0.627522378253398,
0.631977398989734,0.636432419726069,0.670664755628991,0.704897091531912,
0.71057214746399,0.716247203396069,0.727597315260226,0.738947427124383,
0.750297538988541,0.79569798644517,0.806906221911025,0.81811445737688,0.829322692842735,
0.840530928308591,0.862947399240301,0.885363870172012,0.975029753898854),
 .UNSPECIFIED.);
#106=B_SPLINE_SURFACE_WITH_KNOTS('',3,3,((#31639,#31640,#31641,#31642,#31643,
#31644,#31645,#31646,#31647,#31648,#31649,#31650,#31651,#31652,#31653,#31654,
#31655,#31656,#31657,#31658,#31659,#31660,#31661,#31662,#31663,#31664,#31665,
#31666,#31667,#31668,#31669,#31670,#31671,#31672,#31673,#31674,#31675,#31676,
#31677,#31678,#31679,#31680),(#31681,#31682,#31683,#31684,#31685,#31686,
#31687,#31688,#31689,#31690,#31691,#31692,#31693,#31694,#31695,#31696,#31697,
#31698,#31699,#31700,#31701,#31702,#31703,#31704,#31705,#31706,#31707,#31708,
#31709,#31710,#31711,#31712,#31713,#31714,#31715,#31716,#31717,#31718,#31719,
#31720,#31721,#31722),(#31723,#31724,#31725,#31726,#31727,#31728,#31729,
#31730,#31731,#31732,#31733,#31734,#31735,#31736,#31737,#31738,#31739,#31740,
#31741,#31742,#31743,#31744,#31745,#31746,#31747,#31748,#31749,#31750,#31751,
#31752,#31753,#31754,#31755,#31756,#31757,#31758,#31759,#31760,#31761,#31762,
#31763,#31764),(#31765,#31766,#31767,#31768,#31769,#31770,#31771,#31772,
#31773,#31774,#31775,#31776,#31777,#31778,#31779,#31780,#31781,#31782,#31783,
#31784,#31785,#31786,#31787,#31788,#31789,#31790,#31791,#31792,#31793,#31794,
#31795,#31796,#31797,#31798,#31799,#31800,#31801,#31802,#31803,#31804,#31805,
#31806),(#31807,#31808,#31809,#31810,#31811,#31812,#31813,#31814,#31815,
#31816,#31817,#31818,#31819,#31820,#31821,#31822,#31823,#31824,#31825,#31826,
#31827,#31828,#31829,#31830,#31831,#31832,#31833,#31834,#31835,#31836,#31837,
#31838,#31839,#31840,#31841,#31842,#31843,#31844,#31845,#31846,#31847,#31848)),
 .UNSPECIFIED.,.F.,.F.,.F.,(4,1,4),(4,2,2,2,2,2,1,1,2,1,1,1,1,1,1,2,1,2,
1,1,1,1,2,1,1,1,1,1,1,1,4),(0.10381731230502,0.464855998538582,0.946240913516665),
(0.0903575719412648,0.100793262783688,0.212043315812054,0.313257792411489,
0.405143101782566,0.488664067632647,0.50778607271066,0.526908077788674,
0.565152087944702,0.574062129417373,0.582972170890044,0.600792253835385,
0.618612336780727,0.627522378253398,0.631977398989734,0.636432419726069,
0.66210667165326,0.704897091531912,0.716247203396069,0.727597315260226,
0.736109899158344,0.750297538988541,0.79569798644517,0.806906221911025,
0.815312398510416,0.81811445737688,0.840530928308591,0.851739163774446,
0.874155634706157,0.885363870172012,0.975029753898854),.UNSPECIFIED.);
#107=B_SPLINE_SURFACE_WITH_KNOTS('',3,3,((#32095,#32096,#32097,#32098,#32099,
#32100,#32101,#32102,#32103,#32104,#32105,#32106,#32107,#32108,#32109,#32110,
#32111,#32112,#32113,#32114,#32115,#32116,#32117,#32118,#32119,#32120,#32121,
#32122,#32123,#32124,#32125,#32126,#32127,#32128,#32129,#32130,#32131,#32132),
(#32133,#32134,#32135,#32136,#32137,#32138,#32139,#32140,#32141,#32142,
#32143,#32144,#32145,#32146,#32147,#32148,#32149,#32150,#32151,#32152,#32153,
#32154,#32155,#32156,#32157,#32158,#32159,#32160,#32161,#32162,#32163,#32164,
#32165,#32166,#32167,#32168,#32169,#32170),(#32171,#32172,#32173,#32174,
#32175,#32176,#32177,#32178,#32179,#32180,#32181,#32182,#32183,#32184,#32185,
#32186,#32187,#32188,#32189,#32190,#32191,#32192,#32193,#32194,#32195,#32196,
#32197,#32198,#32199,#32200,#32201,#32202,#32203,#32204,#32205,#32206,#32207,
#32208),(#32209,#32210,#32211,#32212,#32213,#32214,#32215,#32216,#32217,
#32218,#32219,#32220,#32221,#32222,#32223,#32224,#32225,#32226,#32227,#32228,
#32229,#32230,#32231,#32232,#32233,#32234,#32235,#32236,#32237,#32238,#32239,
#32240,#32241,#32242,#32243,#32244,#32245,#32246),(#32247,#32248,#32249,
#32250,#32251,#32252,#32253,#32254,#32255,#32256,#32257,#32258,#32259,#32260,
#32261,#32262,#32263,#32264,#32265,#32266,#32267,#32268,#32269,#32270,#32271,
#32272,#32273,#32274,#32275,#32276,#32277,#32278,#32279,#32280,#32281,#32282,
#32283,#32284)),.UNSPECIFIED.,.F.,.F.,.F.,(4,1,4),(4,2,2,2,2,2,1,1,2,1,
1,1,1,1,2,1,2,1,1,1,2,1,1,1,1,1,4),(0.10381731230502,0.464855998538582,
0.946240913516665),(0.0903575719412648,0.100793262783688,0.212043315812054,
0.313257792411489,0.405143101782566,0.488664067632647,0.50778607271066,
0.526908077788674,0.565152087944702,0.574062129417373,0.582972170890044,
0.600792253835385,0.609702295308056,0.618612336780727,0.636432419726069,
0.65354858767753,0.704897091531912,0.716247203396069,0.727597315260226,
0.750297538988541,0.79569798644517,0.806906221911025,0.81811445737688,0.840530928308591,
0.862947399240301,0.885363870172012,0.975029753898854),.UNSPECIFIED.);
#108=B_SPLINE_SURFACE_WITH_KNOTS('',3,3,((#32537,#32538,#32539,#32540,#32541,
#32542,#32543,#32544,#32545,#32546,#32547,#32548,#32549,#32550,#32551,#32552,
#32553,#32554,#32555,#32556,#32557,#32558,#32559,#32560,#32561,#32562,#32563,
#32564,#32565,#32566,#32567,#32568,#32569,#32570,#32571,#32572,#32573,#32574,
#32575,#32576,#32577,#32578,#32579,#32580),(#32581,#32582,#32583,#32584,
#32585,#32586,#32587,#32588,#32589,#32590,#32591,#32592,#32593,#32594,#32595,
#32596,#32597,#32598,#32599,#32600,#32601,#32602,#32603,#32604,#32605,#32606,
#32607,#32608,#32609,#32610,#32611,#32612,#32613,#32614,#32615,#32616,#32617,
#32618,#32619,#32620,#32621,#32622,#32623,#32624),(#32625,#32626,#32627,
#32628,#32629,#32630,#32631,#32632,#32633,#32634,#32635,#32636,#32637,#32638,
#32639,#32640,#32641,#32642,#32643,#32644,#32645,#32646,#32647,#32648,#32649,
#32650,#32651,#32652,#32653,#32654,#32655,#32656,#32657,#32658,#32659,#32660,
#32661,#32662,#32663,#32664,#32665,#32666,#32667,#32668),(#32669,#32670,
#32671,#32672,#32673,#32674,#32675,#32676,#32677,#32678,#32679,#32680,#32681,
#32682,#32683,#32684,#32685,#32686,#32687,#32688,#32689,#32690,#32691,#32692,
#32693,#32694,#32695,#32696,#32697,#32698,#32699,#32700,#32701,#32702,#32703,
#32704,#32705,#32706,#32707,#32708,#32709,#32710,#32711,#32712),(#32713,
#32714,#32715,#32716,#32717,#32718,#32719,#32720,#32721,#32722,#32723,#32724,
#32725,#32726,#32727,#32728,#32729,#32730,#32731,#32732,#32733,#32734,#32735,
#32736,#32737,#32738,#32739,#32740,#32741,#32742,#32743,#32744,#32745,#32746,
#32747,#32748,#32749,#32750,#32751,#32752,#32753,#32754,#32755,#32756)),
 .UNSPECIFIED.,.F.,.F.,.F.,(4,1,4),(4,2,2,2,2,2,1,1,1,2,1,1,1,1,1,1,1,2,
1,2,1,1,1,1,1,2,1,1,1,1,1,1,4),(0.10381731230502,0.585202227283103,0.946240913516665),
(0.0903575719412648,0.100793262783688,0.212043315812054,0.313257792411489,
0.405143101782566,0.488664067632647,0.50778607271066,0.526908077788674,
0.546030082866688,0.565152087944702,0.574062129417373,0.582972170890044,
0.600792253835385,0.609702295308056,0.618612336780727,0.627522378253398,
0.631977398989734,0.636432419726069,0.670664755628991,0.704897091531912,
0.71057214746399,0.716247203396069,0.727597315260226,0.738947427124383,
0.750297538988541,0.79569798644517,0.806906221911025,0.81811445737688,0.829322692842735,
0.840530928308591,0.862947399240301,0.885363870172012,0.975029753898854),
 .UNSPECIFIED.);
#109=B_SPLINE_SURFACE_WITH_KNOTS('',3,3,((#33831,#33832,#33833,#33834,#33835,
#33836,#33837,#33838,#33839,#33840,#33841,#33842,#33843,#33844,#33845,#33846,
#33847,#33848,#33849,#33850,#33851,#33852,#33853,#33854,#33855,#33856,#33857,
#33858,#33859,#33860,#33861,#33862,#33863,#33864,#33865,#33866,#33867,#33868,
#33869,#33870,#33871,#33872,#33873,#33874,#33875,#33876,#33877,#33878,#33879,
#33880,#33881,#33882,#33883,#33884,#33885,#33886,#33887,#33888,#33889,#33890,
#33891,#33892,#33893,#33894,#33895,#33896,#33897,#33898,#33899,#33900,#33901,
#33902,#33903,#33904,#33905,#33906,#33907,#33908,#33909,#33910,#33911,#33912,
#33913,#33914,#33915,#33916,#33917,#33918,#33919,#33920,#33921,#33922,#33923,
#33924,#33925,#33926,#33927,#33928,#33929,#33930,#33931,#33932,#33933,#33934,
#33935,#33936,#33937),(#33938,#33939,#33940,#33941,#33942,#33943,#33944,
#33945,#33946,#33947,#33948,#33949,#33950,#33951,#33952,#33953,#33954,#33955,
#33956,#33957,#33958,#33959,#33960,#33961,#33962,#33963,#33964,#33965,#33966,
#33967,#33968,#33969,#33970,#33971,#33972,#33973,#33974,#33975,#33976,#33977,
#33978,#33979,#33980,#33981,#33982,#33983,#33984,#33985,#33986,#33987,#33988,
#33989,#33990,#33991,#33992,#33993,#33994,#33995,#33996,#33997,#33998,#33999,
#34000,#34001,#34002,#34003,#34004,#34005,#34006,#34007,#34008,#34009,#34010,
#34011,#34012,#34013,#34014,#34015,#34016,#34017,#34018,#34019,#34020,#34021,
#34022,#34023,#34024,#34025,#34026,#34027,#34028,#34029,#34030,#34031,#34032,
#34033,#34034,#34035,#34036,#34037,#34038,#34039,#34040,#34041,#34042,#34043,
#34044),(#34045,#34046,#34047,#34048,#34049,#34050,#34051,#34052,#34053,
#34054,#34055,#34056,#34057,#34058,#34059,#34060,#34061,#34062,#34063,#34064,
#34065,#34066,#34067,#34068,#34069,#34070,#34071,#34072,#34073,#34074,#34075,
#34076,#34077,#34078,#34079,#34080,#34081,#34082,#34083,#34084,#34085,#34086,
#34087,#34088,#34089,#34090,#34091,#34092,#34093,#34094,#34095,#34096,#34097,
#34098,#34099,#34100,#34101,#34102,#34103,#34104,#34105,#34106,#34107,#34108,
#34109,#34110,#34111,#34112,#34113,#34114,#34115,#34116,#34117,#34118,#34119,
#34120,#34121,#34122,#34123,#34124,#34125,#34126,#34127,#34128,#34129,#34130,
#34131,#34132,#34133,#34134,#34135,#34136,#34137,#34138,#34139,#34140,#34141,
#34142,#34143,#34144,#34145,#34146,#34147,#34148,#34149,#34150,#34151),
(#34152,#34153,#34154,#34155,#34156,#34157,#34158,#34159,#34160,#34161,
#34162,#34163,#34164,#34165,#34166,#34167,#34168,#34169,#34170,#34171,#34172,
#34173,#34174,#34175,#34176,#34177,#34178,#34179,#34180,#34181,#34182,#34183,
#34184,#34185,#34186,#34187,#34188,#34189,#34190,#34191,#34192,#34193,#34194,
#34195,#34196,#34197,#34198,#34199,#34200,#34201,#34202,#34203,#34204,#34205,
#34206,#34207,#34208,#34209,#34210,#34211,#34212,#34213,#34214,#34215,#34216,
#34217,#34218,#34219,#34220,#34221,#34222,#34223,#34224,#34225,#34226,#34227,
#34228,#34229,#34230,#34231,#34232,#34233,#34234,#34235,#34236,#34237,#34238,
#34239,#34240,#34241,#34242,#34243,#34244,#34245,#34246,#34247,#34248,#34249,
#34250,#34251,#34252,#34253,#34254,#34255,#34256,#34257,#34258)),
 .UNSPECIFIED.,.F.,.F.,.F.,(4,4),(4,1,1,1,1,1,1,1,1,1,1,1,1,1,1,1,1,1,1,
1,1,1,1,1,1,1,1,1,1,1,1,1,1,1,1,1,1,1,1,1,1,1,1,1,1,1,1,1,1,1,1,1,1,1,1,
1,1,1,1,1,1,1,1,1,1,1,1,1,1,1,1,1,1,1,1,1,1,1,1,1,1,1,1,1,1,1,1,1,1,1,1,
1,1,1,1,1,1,1,1,1,1,1,1,1,4),(0.,0.0658179306876168),(8.30838445208336,
9.3001665031586,10.2919485542338,11.2837306053091,12.2755126563843,13.2672947074596,
14.2590767585348,15.25085880961,16.2426408606853,17.2344229117605,18.2262049628358,
19.217987013911,20.2097690649862,21.2015511160615,22.1933331671367,23.185115218212,
24.1768972692872,25.1686793203624,26.1604613714377,27.1522434225129,28.1440254735882,
29.1358075246634,30.1275895757386,31.1193716268139,32.1111536778891,33.1029357289644,
34.0947177800396,35.0864998311148,36.0782818821901,37.0700639332653,38.0618459843406,
39.0536280354158,40.0454100864911,41.0371921375663,42.0289741886415,43.0207562397168,
44.012538290792,45.0043203418673,45.9961023929425,46.9878844440177,47.979666495093,
48.9714485461682,49.9632305972435,50.9550126483187,51.9467946993939,52.9385767504692,
53.9303588015444,54.9221408526197,55.9139229036949,56.9057049547701,57.8974870058454,
58.8892690569206,59.8810511079959,60.8728331590711,61.8646152101463,62.8563972612216,
63.8481793122968,64.8399613633721,65.8317434144473,66.8235254655226,67.8153075165978,
68.807089567673,69.7988716187483,70.7906536698235,71.7824357208987,72.774217771974,
73.7659998230492,74.7577818741245,75.7495639251997,76.741345976275,77.7331280273502,
78.7249100784254,79.7166921295007,80.7084741805759,81.7002562316512,82.6920382827264,
83.6838203338016,84.6756023848769,85.6673844359521,86.6591664870274,87.6509485381026,
88.6427305891778,89.6345126402531,90.6262946913283,91.6180767424036,92.6098587934788,
93.601640844554,94.5934228956293,95.5852049467045,96.5769869977798,97.568769048855,
98.5605510999303,99.5523331510055,100.544115202081,101.535897253156,102.527679304231,
103.519461355306,104.511243406382,105.503025457457,106.494807508532,107.486589559607,
108.478371610683,109.470153661758,110.461935712833,111.453717763908),
 .UNSPECIFIED.);
#110=B_SPLINE_SURFACE_WITH_KNOTS('',3,3,((#34494,#34495,#34496,#34497,#34498,
#34499,#34500,#34501,#34502,#34503,#34504,#34505,#34506,#34507,#34508,#34509,
#34510,#34511,#34512,#34513,#34514,#34515,#34516,#34517,#34518,#34519,#34520,
#34521,#34522,#34523,#34524,#34525,#34526,#34527,#34528,#34529,#34530,#34531,
#34532,#34533,#34534,#34535,#34536,#34537,#34538,#34539,#34540,#34541,#34542,
#34543,#34544,#34545,#34546,#34547,#34548,#34549,#34550,#34551,#34552,#34553,
#34554,#34555,#34556,#34557,#34558,#34559,#34560,#34561,#34562,#34563,#34564,
#34565,#34566,#34567,#34568,#34569,#34570,#34571,#34572,#34573,#34574,#34575,
#34576,#34577,#34578,#34579,#34580,#34581,#34582,#34583,#34584,#34585,#34586,
#34587,#34588,#34589,#34590,#34591,#34592,#34593,#34594,#34595,#34596,#34597,
#34598,#34599,#34600),(#34601,#34602,#34603,#34604,#34605,#34606,#34607,
#34608,#34609,#34610,#34611,#34612,#34613,#34614,#34615,#34616,#34617,#34618,
#34619,#34620,#34621,#34622,#34623,#34624,#34625,#34626,#34627,#34628,#34629,
#34630,#34631,#34632,#34633,#34634,#34635,#34636,#34637,#34638,#34639,#34640,
#34641,#34642,#34643,#34644,#34645,#34646,#34647,#34648,#34649,#34650,#34651,
#34652,#34653,#34654,#34655,#34656,#34657,#34658,#34659,#34660,#34661,#34662,
#34663,#34664,#34665,#34666,#34667,#34668,#34669,#34670,#34671,#34672,#34673,
#34674,#34675,#34676,#34677,#34678,#34679,#34680,#34681,#34682,#34683,#34684,
#34685,#34686,#34687,#34688,#34689,#34690,#34691,#34692,#34693,#34694,#34695,
#34696,#34697,#34698,#34699,#34700,#34701,#34702,#34703,#34704,#34705,#34706,
#34707),(#34708,#34709,#34710,#34711,#34712,#34713,#34714,#34715,#34716,
#34717,#34718,#34719,#34720,#34721,#34722,#34723,#34724,#34725,#34726,#34727,
#34728,#34729,#34730,#34731,#34732,#34733,#34734,#34735,#34736,#34737,#34738,
#34739,#34740,#34741,#34742,#34743,#34744,#34745,#34746,#34747,#34748,#34749,
#34750,#34751,#34752,#34753,#34754,#34755,#34756,#34757,#34758,#34759,#34760,
#34761,#34762,#34763,#34764,#34765,#34766,#34767,#34768,#34769,#34770,#34771,
#34772,#34773,#34774,#34775,#34776,#34777,#34778,#34779,#34780,#34781,#34782,
#34783,#34784,#34785,#34786,#34787,#34788,#34789,#34790,#34791,#34792,#34793,
#34794,#34795,#34796,#34797,#34798,#34799,#34800,#34801,#34802,#34803,#34804,
#34805,#34806,#34807,#34808,#34809,#34810,#34811,#34812,#34813,#34814),
(#34815,#34816,#34817,#34818,#34819,#34820,#34821,#34822,#34823,#34824,
#34825,#34826,#34827,#34828,#34829,#34830,#34831,#34832,#34833,#34834,#34835,
#34836,#34837,#34838,#34839,#34840,#34841,#34842,#34843,#34844,#34845,#34846,
#34847,#34848,#34849,#34850,#34851,#34852,#34853,#34854,#34855,#34856,#34857,
#34858,#34859,#34860,#34861,#34862,#34863,#34864,#34865,#34866,#34867,#34868,
#34869,#34870,#34871,#34872,#34873,#34874,#34875,#34876,#34877,#34878,#34879,
#34880,#34881,#34882,#34883,#34884,#34885,#34886,#34887,#34888,#34889,#34890,
#34891,#34892,#34893,#34894,#34895,#34896,#34897,#34898,#34899,#34900,#34901,
#34902,#34903,#34904,#34905,#34906,#34907,#34908,#34909,#34910,#34911,#34912,
#34913,#34914,#34915,#34916,#34917,#34918,#34919,#34920,#34921)),
 .UNSPECIFIED.,.F.,.F.,.F.,(4,4),(4,1,1,1,1,1,1,1,1,1,1,1,1,1,1,1,1,1,1,
1,1,1,1,1,1,1,1,1,1,1,1,1,1,1,1,1,1,1,1,1,1,1,1,1,1,1,1,1,1,1,1,1,1,1,1,
1,1,1,1,1,1,1,1,1,1,1,1,1,1,1,1,1,1,1,1,1,1,1,1,1,1,1,1,1,1,1,1,1,1,1,1,
1,1,1,1,1,1,1,1,1,1,1,1,1,4),(0.,0.0658179306876168),(11.6150328478185,
12.6068148988938,13.598596949969,14.5903790010443,15.5821610521195,16.5739431031947,
17.56572515427,18.5575072053452,19.5492892564205,20.5410713074957,21.5328533585709,
22.5246354096462,23.5164174607214,24.5081995117967,25.4999815628719,26.4917636139471,
27.4835456650224,28.4753277160976,29.4671097671729,30.4588918182481,31.4506738693233,
32.4424559203986,33.4342379714738,34.4260200225491,35.4178020736243,36.4095841246995,
37.4013661757748,38.39314822685,39.3849302779253,40.3767123290005,41.3684943800758,
42.360276431151,43.3520584822262,44.3438405333015,45.3356225843767,46.327404635452,
47.3191866865272,48.3109687376024,49.3027507886777,50.2945328397529,51.2863148908282,
52.2780969419034,53.2698789929786,54.2616610440539,55.2534430951291,56.2452251462044,
57.2370071972796,58.2287892483548,59.2205712994301,60.2123533505053,61.2041354015806,
62.1959174526558,63.187699503731,64.1794815548063,65.1712636058815,66.1630456569568,
67.154827708032,68.1466097591072,69.1383918101825,70.1301738612577,71.121955912333,
72.1137379634082,73.1055200144834,74.0973020655587,75.0890841166339,76.0808661677092,
77.0726482187844,78.0644302698597,79.0562123209349,80.0479943720101,81.0397764230854,
82.0315584741606,83.0233405252359,84.0151225763111,85.0069046273863,85.9986866784616,
86.9904687295368,87.9822507806121,88.9740328316873,89.9658148827625,90.9575969338378,
91.949378984913,92.9411610359883,93.9329430870635,94.9247251381387,95.916507189214,
96.9082892402892,97.9000712913645,98.8918533424397,99.883635393515,100.87541744459,
101.867199495665,102.858981546741,103.850763597816,104.842545648891,105.834327699966,
106.826109751042,107.817891802117,108.809673853192,109.801455904267,110.793237955343,
111.785020006418,112.776802057493,113.768584108568,114.760366159644),
 .UNSPECIFIED.);
#111=B_SPLINE_SURFACE_WITH_KNOTS('',3,3,((#35814,#35815,#35816,#35817,#35818,
#35819,#35820,#35821,#35822,#35823,#35824,#35825,#35826,#35827,#35828,#35829,
#35830,#35831,#35832,#35833,#35834,#35835,#35836,#35837,#35838,#35839,#35840,
#35841,#35842,#35843,#35844,#35845,#35846,#35847,#35848,#35849,#35850,#35851,
#35852,#35853),(#35854,#35855,#35856,#35857,#35858,#35859,#35860,#35861,
#35862,#35863,#35864,#35865,#35866,#35867,#35868,#35869,#35870,#35871,#35872,
#35873,#35874,#35875,#35876,#35877,#35878,#35879,#35880,#35881,#35882,#35883,
#35884,#35885,#35886,#35887,#35888,#35889,#35890,#35891,#35892,#35893),
(#35894,#35895,#35896,#35897,#35898,#35899,#35900,#35901,#35902,#35903,
#35904,#35905,#35906,#35907,#35908,#35909,#35910,#35911,#35912,#35913,#35914,
#35915,#35916,#35917,#35918,#35919,#35920,#35921,#35922,#35923,#35924,#35925,
#35926,#35927,#35928,#35929,#35930,#35931,#35932,#35933),(#35934,#35935,
#35936,#35937,#35938,#35939,#35940,#35941,#35942,#35943,#35944,#35945,#35946,
#35947,#35948,#35949,#35950,#35951,#35952,#35953,#35954,#35955,#35956,#35957,
#35958,#35959,#35960,#35961,#35962,#35963,#35964,#35965,#35966,#35967,#35968,
#35969,#35970,#35971,#35972,#35973),(#35974,#35975,#35976,#35977,#35978,
#35979,#35980,#35981,#35982,#35983,#35984,#35985,#35986,#35987,#35988,#35989,
#35990,#35991,#35992,#35993,#35994,#35995,#35996,#35997,#35998,#35999,#36000,
#36001,#36002,#36003,#36004,#36005,#36006,#36007,#36008,#36009,#36010,#36011,
#36012,#36013)),.UNSPECIFIED.,.F.,.F.,.F.,(4,1,4),(4,2,2,2,2,2,1,1,2,1,
1,1,1,1,1,2,1,2,1,1,1,1,2,1,1,1,1,1,4),(0.104020343629189,0.464972094135687,
0.946241094811018),(0.00211325483337195,0.100793262783688,0.212043315812054,
0.313257792411489,0.405143101782566,0.488664067632647,0.50778607271066,
0.526908077788674,0.565152087944702,0.569607108681037,0.574062129417373,
0.582972170890044,0.600792253835385,0.618612336780727,0.627522378253398,
0.636432419726069,0.670664755628991,0.704897091531912,0.71057214746399,
0.716247203396069,0.727597315260226,0.750297538988541,0.79569798644517,
0.806906221911025,0.81811445737688,0.840530928308591,0.862947399240301,
0.885363870172012,0.975029753898854),.UNSPECIFIED.);
#112=B_SPLINE_SURFACE_WITH_KNOTS('',3,3,((#36323,#36324,#36325,#36326,#36327,
#36328,#36329,#36330,#36331,#36332,#36333,#36334,#36335,#36336,#36337,#36338,
#36339,#36340,#36341,#36342,#36343,#36344,#36345,#36346,#36347,#36348,#36349,
#36350,#36351,#36352,#36353,#36354,#36355,#36356,#36357,#36358,#36359,#36360,
#36361,#36362,#36363,#36364),(#36365,#36366,#36367,#36368,#36369,#36370,
#36371,#36372,#36373,#36374,#36375,#36376,#36377,#36378,#36379,#36380,#36381,
#36382,#36383,#36384,#36385,#36386,#36387,#36388,#36389,#36390,#36391,#36392,
#36393,#36394,#36395,#36396,#36397,#36398,#36399,#36400,#36401,#36402,#36403,
#36404,#36405,#36406),(#36407,#36408,#36409,#36410,#36411,#36412,#36413,
#36414,#36415,#36416,#36417,#36418,#36419,#36420,#36421,#36422,#36423,#36424,
#36425,#36426,#36427,#36428,#36429,#36430,#36431,#36432,#36433,#36434,#36435,
#36436,#36437,#36438,#36439,#36440,#36441,#36442,#36443,#36444,#36445,#36446,
#36447,#36448),(#36449,#36450,#36451,#36452,#36453,#36454,#36455,#36456,
#36457,#36458,#36459,#36460,#36461,#36462,#36463,#36464,#36465,#36466,#36467,
#36468,#36469,#36470,#36471,#36472,#36473,#36474,#36475,#36476,#36477,#36478,
#36479,#36480,#36481,#36482,#36483,#36484,#36485,#36486,#36487,#36488,#36489,
#36490),(#36491,#36492,#36493,#36494,#36495,#36496,#36497,#36498,#36499,
#36500,#36501,#36502,#36503,#36504,#36505,#36506,#36507,#36508,#36509,#36510,
#36511,#36512,#36513,#36514,#36515,#36516,#36517,#36518,#36519,#36520,#36521,
#36522,#36523,#36524,#36525,#36526,#36527,#36528,#36529,#36530,#36531,#36532)),
 .UNSPECIFIED.,.F.,.F.,.F.,(4,1,4),(4,2,2,2,1,2,2,1,1,2,1,1,1,1,1,1,1,2,
1,2,1,1,1,1,2,1,1,1,1,1,4),(0.104020343629189,0.464972094135687,0.946241094811018),
(0.00211325483337195,0.100793262783688,0.212043315812054,0.313257792411489,
0.336229119754259,0.405143101782566,0.488664067632647,0.50778607271066,
0.526908077788674,0.565152087944702,0.582972170890044,0.600792253835385,
0.609702295308056,0.618612336780727,0.627522378253398,0.631977398989734,
0.634204909357901,0.636432419726069,0.670664755628991,0.704897091531912,
0.71057214746399,0.716247203396069,0.727597315260226,0.750297538988541,
0.79569798644517,0.806906221911025,0.81811445737688,0.840530928308591,0.862947399240301,
0.885363870172012,0.975029753898854),.UNSPECIFIED.);
#113=B_SPLINE_SURFACE_WITH_KNOTS('',3,3,((#36842,#36843,#36844,#36845,#36846,
#36847,#36848,#36849,#36850,#36851,#36852,#36853,#36854,#36855,#36856,#36857,
#36858,#36859,#36860,#36861,#36862,#36863,#36864,#36865,#36866,#36867,#36868,
#36869,#36870,#36871,#36872,#36873,#36874,#36875,#36876,#36877,#36878,#36879),
(#36880,#36881,#36882,#36883,#36884,#36885,#36886,#36887,#36888,#36889,
#36890,#36891,#36892,#36893,#36894,#36895,#36896,#36897,#36898,#36899,#36900,
#36901,#36902,#36903,#36904,#36905,#36906,#36907,#36908,#36909,#36910,#36911,
#36912,#36913,#36914,#36915,#36916,#36917),(#36918,#36919,#36920,#36921,
#36922,#36923,#36924,#36925,#36926,#36927,#36928,#36929,#36930,#36931,#36932,
#36933,#36934,#36935,#36936,#36937,#36938,#36939,#36940,#36941,#36942,#36943,
#36944,#36945,#36946,#36947,#36948,#36949,#36950,#36951,#36952,#36953,#36954,
#36955),(#36956,#36957,#36958,#36959,#36960,#36961,#36962,#36963,#36964,
#36965,#36966,#36967,#36968,#36969,#36970,#36971,#36972,#36973,#36974,#36975,
#36976,#36977,#36978,#36979,#36980,#36981,#36982,#36983,#36984,#36985,#36986,
#36987,#36988,#36989,#36990,#36991,#36992,#36993),(#36994,#36995,#36996,
#36997,#36998,#36999,#37000,#37001,#37002,#37003,#37004,#37005,#37006,#37007,
#37008,#37009,#37010,#37011,#37012,#37013,#37014,#37015,#37016,#37017,#37018,
#37019,#37020,#37021,#37022,#37023,#37024,#37025,#37026,#37027,#37028,#37029,
#37030,#37031)),.UNSPECIFIED.,.F.,.F.,.F.,(4,1,4),(4,2,2,2,1,2,2,1,2,1,
1,1,1,1,2,1,2,1,1,1,2,1,1,1,1,1,4),(0.104020343629189,0.464972094135687,
0.946241094811018),(0.00211325483337195,0.100793262783688,0.212043315812054,
0.313257792411489,0.336229119754259,0.405143101782566,0.488664067632647,
0.526908077788674,0.565152087944702,0.569607108681037,0.574062129417373,
0.582972170890044,0.600792253835385,0.618612336780727,0.636432419726069,
0.65354858767753,0.704897091531912,0.716247203396069,0.727597315260226,
0.750297538988541,0.79569798644517,0.806906221911025,0.81811445737688,0.840530928308591,
0.851739163774446,0.885363870172012,0.975029753898854),.UNSPECIFIED.);
#114=B_SPLINE_SURFACE_WITH_KNOTS('',3,3,((#37341,#37342,#37343,#37344,#37345,
#37346,#37347,#37348,#37349,#37350,#37351,#37352,#37353,#37354,#37355,#37356,
#37357,#37358,#37359,#37360,#37361,#37362,#37363,#37364,#37365,#37366,#37367,
#37368,#37369,#37370,#37371,#37372,#37373,#37374,#37375,#37376,#37377,#37378,
#37379,#37380),(#37381,#37382,#37383,#37384,#37385,#37386,#37387,#37388,
#37389,#37390,#37391,#37392,#37393,#37394,#37395,#37396,#37397,#37398,#37399,
#37400,#37401,#37402,#37403,#37404,#37405,#37406,#37407,#37408,#37409,#37410,
#37411,#37412,#37413,#37414,#37415,#37416,#37417,#37418,#37419,#37420),
(#37421,#37422,#37423,#37424,#37425,#37426,#37427,#37428,#37429,#37430,
#37431,#37432,#37433,#37434,#37435,#37436,#37437,#37438,#37439,#37440,#37441,
#37442,#37443,#37444,#37445,#37446,#37447,#37448,#37449,#37450,#37451,#37452,
#37453,#37454,#37455,#37456,#37457,#37458,#37459,#37460),(#37461,#37462,
#37463,#37464,#37465,#37466,#37467,#37468,#37469,#37470,#37471,#37472,#37473,
#37474,#37475,#37476,#37477,#37478,#37479,#37480,#37481,#37482,#37483,#37484,
#37485,#37486,#37487,#37488,#37489,#37490,#37491,#37492,#37493,#37494,#37495,
#37496,#37497,#37498,#37499,#37500),(#37501,#37502,#37503,#37504,#37505,
#37506,#37507,#37508,#37509,#37510,#37511,#37512,#37513,#37514,#37515,#37516,
#37517,#37518,#37519,#37520,#37521,#37522,#37523,#37524,#37525,#37526,#37527,
#37528,#37529,#37530,#37531,#37532,#37533,#37534,#37535,#37536,#37537,#37538,
#37539,#37540)),.UNSPECIFIED.,.F.,.F.,.F.,(4,1,4),(4,2,2,2,2,2,1,1,2,1,
1,1,1,1,1,2,1,2,1,1,1,1,2,1,1,1,1,1,4),(0.104020343629189,0.464972094135687,
0.946241094811018),(0.00211325483337195,0.100793262783688,0.212043315812054,
0.313257792411489,0.405143101782566,0.488664067632647,0.50778607271066,
0.526908077788674,0.565152087944702,0.569607108681037,0.574062129417373,
0.582972170890044,0.600792253835385,0.618612336780727,0.627522378253398,
0.636432419726069,0.670664755628991,0.704897091531912,0.71057214746399,
0.716247203396069,0.727597315260226,0.750297538988541,0.79569798644517,
0.806906221911025,0.81811445737688,0.840530928308591,0.862947399240301,
0.885363870172012,0.975029753898854),.UNSPECIFIED.);
#115=B_SPLINE_SURFACE_WITH_KNOTS('',3,3,((#37850,#37851,#37852,#37853,#37854,
#37855,#37856,#37857,#37858,#37859,#37860,#37861,#37862,#37863,#37864,#37865,
#37866,#37867,#37868,#37869,#37870,#37871,#37872,#37873,#37874,#37875,#37876,
#37877,#37878,#37879,#37880,#37881,#37882,#37883,#37884,#37885,#37886,#37887,
#37888,#37889,#37890,#37891),(#37892,#37893,#37894,#37895,#37896,#37897,
#37898,#37899,#37900,#37901,#37902,#37903,#37904,#37905,#37906,#37907,#37908,
#37909,#37910,#37911,#37912,#37913,#37914,#37915,#37916,#37917,#37918,#37919,
#37920,#37921,#37922,#37923,#37924,#37925,#37926,#37927,#37928,#37929,#37930,
#37931,#37932,#37933),(#37934,#37935,#37936,#37937,#37938,#37939,#37940,
#37941,#37942,#37943,#37944,#37945,#37946,#37947,#37948,#37949,#37950,#37951,
#37952,#37953,#37954,#37955,#37956,#37957,#37958,#37959,#37960,#37961,#37962,
#37963,#37964,#37965,#37966,#37967,#37968,#37969,#37970,#37971,#37972,#37973,
#37974,#37975),(#37976,#37977,#37978,#37979,#37980,#37981,#37982,#37983,
#37984,#37985,#37986,#37987,#37988,#37989,#37990,#37991,#37992,#37993,#37994,
#37995,#37996,#37997,#37998,#37999,#38000,#38001,#38002,#38003,#38004,#38005,
#38006,#38007,#38008,#38009,#38010,#38011,#38012,#38013,#38014,#38015,#38016,
#38017),(#38018,#38019,#38020,#38021,#38022,#38023,#38024,#38025,#38026,
#38027,#38028,#38029,#38030,#38031,#38032,#38033,#38034,#38035,#38036,#38037,
#38038,#38039,#38040,#38041,#38042,#38043,#38044,#38045,#38046,#38047,#38048,
#38049,#38050,#38051,#38052,#38053,#38054,#38055,#38056,#38057,#38058,#38059)),
 .UNSPECIFIED.,.F.,.F.,.F.,(4,1,4),(4,2,2,2,1,2,2,1,1,2,1,1,1,1,1,1,1,2,
1,2,1,1,1,1,2,1,1,1,1,1,4),(0.104020343629189,0.464972094135687,0.946241094811018),
(0.00211325483337195,0.100793262783688,0.212043315812054,0.313257792411489,
0.336229119754259,0.405143101782566,0.488664067632647,0.50778607271066,
0.526908077788674,0.565152087944702,0.582972170890044,0.600792253835385,
0.609702295308056,0.618612336780727,0.627522378253398,0.631977398989734,
0.634204909357901,0.636432419726069,0.670664755628991,0.704897091531912,
0.71057214746399,0.716247203396069,0.727597315260226,0.750297538988541,
0.79569798644517,0.806906221911025,0.81811445737688,0.840530928308591,0.862947399240301,
0.885363870172012,0.975029753898854),.UNSPECIFIED.);
#116=B_SPLINE_SURFACE_WITH_KNOTS('',3,3,((#38369,#38370,#38371,#38372,#38373,
#38374,#38375,#38376,#38377,#38378,#38379,#38380,#38381,#38382,#38383,#38384,
#38385,#38386,#38387,#38388,#38389,#38390,#38391,#38392,#38393,#38394,#38395,
#38396,#38397,#38398,#38399,#38400,#38401,#38402,#38403,#38404,#38405,#38406),
(#38407,#38408,#38409,#38410,#38411,#38412,#38413,#38414,#38415,#38416,
#38417,#38418,#38419,#38420,#38421,#38422,#38423,#38424,#38425,#38426,#38427,
#38428,#38429,#38430,#38431,#38432,#38433,#38434,#38435,#38436,#38437,#38438,
#38439,#38440,#38441,#38442,#38443,#38444),(#38445,#38446,#38447,#38448,
#38449,#38450,#38451,#38452,#38453,#38454,#38455,#38456,#38457,#38458,#38459,
#38460,#38461,#38462,#38463,#38464,#38465,#38466,#38467,#38468,#38469,#38470,
#38471,#38472,#38473,#38474,#38475,#38476,#38477,#38478,#38479,#38480,#38481,
#38482),(#38483,#38484,#38485,#38486,#38487,#38488,#38489,#38490,#38491,
#38492,#38493,#38494,#38495,#38496,#38497,#38498,#38499,#38500,#38501,#38502,
#38503,#38504,#38505,#38506,#38507,#38508,#38509,#38510,#38511,#38512,#38513,
#38514,#38515,#38516,#38517,#38518,#38519,#38520),(#38521,#38522,#38523,
#38524,#38525,#38526,#38527,#38528,#38529,#38530,#38531,#38532,#38533,#38534,
#38535,#38536,#38537,#38538,#38539,#38540,#38541,#38542,#38543,#38544,#38545,
#38546,#38547,#38548,#38549,#38550,#38551,#38552,#38553,#38554,#38555,#38556,
#38557,#38558)),.UNSPECIFIED.,.F.,.F.,.F.,(4,1,4),(4,2,2,2,1,2,2,1,2,1,
1,1,1,1,2,1,2,1,1,1,2,1,1,1,1,1,4),(0.104020343629189,0.464972094135687,
0.946241094811018),(0.00211325483337195,0.100793262783688,0.212043315812054,
0.313257792411489,0.336229119754259,0.405143101782566,0.488664067632647,
0.526908077788674,0.565152087944702,0.569607108681037,0.574062129417373,
0.582972170890044,0.600792253835385,0.618612336780727,0.636432419726069,
0.65354858767753,0.704897091531912,0.716247203396069,0.727597315260226,
0.750297538988541,0.79569798644517,0.806906221911025,0.81811445737688,0.840530928308591,
0.851739163774446,0.885363870172012,0.975029753898854),.UNSPECIFIED.);
#117=B_SPLINE_SURFACE_WITH_KNOTS('',3,3,((#38868,#38869,#38870,#38871,#38872,
#38873,#38874,#38875,#38876,#38877,#38878,#38879,#38880,#38881,#38882,#38883,
#38884,#38885,#38886,#38887,#38888,#38889,#38890,#38891,#38892,#38893,#38894,
#38895,#38896,#38897,#38898,#38899,#38900,#38901,#38902,#38903,#38904,#38905,
#38906,#38907),(#38908,#38909,#38910,#38911,#38912,#38913,#38914,#38915,
#38916,#38917,#38918,#38919,#38920,#38921,#38922,#38923,#38924,#38925,#38926,
#38927,#38928,#38929,#38930,#38931,#38932,#38933,#38934,#38935,#38936,#38937,
#38938,#38939,#38940,#38941,#38942,#38943,#38944,#38945,#38946,#38947),
(#38948,#38949,#38950,#38951,#38952,#38953,#38954,#38955,#38956,#38957,
#38958,#38959,#38960,#38961,#38962,#38963,#38964,#38965,#38966,#38967,#38968,
#38969,#38970,#38971,#38972,#38973,#38974,#38975,#38976,#38977,#38978,#38979,
#38980,#38981,#38982,#38983,#38984,#38985,#38986,#38987),(#38988,#38989,
#38990,#38991,#38992,#38993,#38994,#38995,#38996,#38997,#38998,#38999,#39000,
#39001,#39002,#39003,#39004,#39005,#39006,#39007,#39008,#39009,#39010,#39011,
#39012,#39013,#39014,#39015,#39016,#39017,#39018,#39019,#39020,#39021,#39022,
#39023,#39024,#39025,#39026,#39027),(#39028,#39029,#39030,#39031,#39032,
#39033,#39034,#39035,#39036,#39037,#39038,#39039,#39040,#39041,#39042,#39043,
#39044,#39045,#39046,#39047,#39048,#39049,#39050,#39051,#39052,#39053,#39054,
#39055,#39056,#39057,#39058,#39059,#39060,#39061,#39062,#39063,#39064,#39065,
#39066,#39067)),.UNSPECIFIED.,.F.,.F.,.F.,(4,1,4),(4,2,2,2,2,2,1,1,2,1,
1,1,1,1,1,2,1,2,1,1,1,1,2,1,1,1,1,1,4),(0.104020343629189,0.464972094135687,
0.946241094811018),(0.00211325483337195,0.100793262783688,0.212043315812054,
0.313257792411489,0.405143101782566,0.488664067632647,0.50778607271066,
0.526908077788674,0.565152087944702,0.569607108681037,0.574062129417373,
0.582972170890044,0.600792253835385,0.618612336780727,0.627522378253398,
0.636432419726069,0.670664755628991,0.704897091531912,0.71057214746399,
0.716247203396069,0.727597315260226,0.750297538988541,0.79569798644517,
0.806906221911025,0.81811445737688,0.840530928308591,0.862947399240301,
0.885363870172012,0.975029753898854),.UNSPECIFIED.);
#118=B_SPLINE_SURFACE_WITH_KNOTS('',3,3,((#39377,#39378,#39379,#39380,#39381,
#39382,#39383,#39384,#39385,#39386,#39387,#39388,#39389,#39390,#39391,#39392,
#39393,#39394,#39395,#39396,#39397,#39398,#39399,#39400,#39401,#39402,#39403,
#39404,#39405,#39406,#39407,#39408,#39409,#39410,#39411,#39412,#39413,#39414,
#39415,#39416,#39417,#39418),(#39419,#39420,#39421,#39422,#39423,#39424,
#39425,#39426,#39427,#39428,#39429,#39430,#39431,#39432,#39433,#39434,#39435,
#39436,#39437,#39438,#39439,#39440,#39441,#39442,#39443,#39444,#39445,#39446,
#39447,#39448,#39449,#39450,#39451,#39452,#39453,#39454,#39455,#39456,#39457,
#39458,#39459,#39460),(#39461,#39462,#39463,#39464,#39465,#39466,#39467,
#39468,#39469,#39470,#39471,#39472,#39473,#39474,#39475,#39476,#39477,#39478,
#39479,#39480,#39481,#39482,#39483,#39484,#39485,#39486,#39487,#39488,#39489,
#39490,#39491,#39492,#39493,#39494,#39495,#39496,#39497,#39498,#39499,#39500,
#39501,#39502),(#39503,#39504,#39505,#39506,#39507,#39508,#39509,#39510,
#39511,#39512,#39513,#39514,#39515,#39516,#39517,#39518,#39519,#39520,#39521,
#39522,#39523,#39524,#39525,#39526,#39527,#39528,#39529,#39530,#39531,#39532,
#39533,#39534,#39535,#39536,#39537,#39538,#39539,#39540,#39541,#39542,#39543,
#39544),(#39545,#39546,#39547,#39548,#39549,#39550,#39551,#39552,#39553,
#39554,#39555,#39556,#39557,#39558,#39559,#39560,#39561,#39562,#39563,#39564,
#39565,#39566,#39567,#39568,#39569,#39570,#39571,#39572,#39573,#39574,#39575,
#39576,#39577,#39578,#39579,#39580,#39581,#39582,#39583,#39584,#39585,#39586)),
 .UNSPECIFIED.,.F.,.F.,.F.,(4,1,4),(4,2,2,2,1,2,2,1,1,2,1,1,1,1,1,1,1,2,
1,2,1,1,1,1,2,1,1,1,1,1,4),(0.104020343629189,0.464972094135687,0.946241094811018),
(0.00211325483337195,0.100793262783688,0.212043315812054,0.313257792411489,
0.336229119754259,0.405143101782566,0.488664067632647,0.50778607271066,
0.526908077788674,0.565152087944702,0.582972170890044,0.600792253835385,
0.609702295308056,0.618612336780727,0.627522378253398,0.631977398989734,
0.634204909357901,0.636432419726069,0.670664755628991,0.704897091531912,
0.71057214746399,0.716247203396069,0.727597315260226,0.750297538988541,
0.79569798644517,0.806906221911025,0.81811445737688,0.840530928308591,0.862947399240301,
0.885363870172012,0.975029753898854),.UNSPECIFIED.);
#119=B_SPLINE_SURFACE_WITH_KNOTS('',3,3,((#39896,#39897,#39898,#39899,#39900,
#39901,#39902,#39903,#39904,#39905,#39906,#39907,#39908,#39909,#39910,#39911,
#39912,#39913,#39914,#39915,#39916,#39917,#39918,#39919,#39920,#39921,#39922,
#39923,#39924,#39925,#39926,#39927,#39928,#39929,#39930,#39931,#39932,#39933,
#39934,#39935),(#39936,#39937,#39938,#39939,#39940,#39941,#39942,#39943,
#39944,#39945,#39946,#39947,#39948,#39949,#39950,#39951,#39952,#39953,#39954,
#39955,#39956,#39957,#39958,#39959,#39960,#39961,#39962,#39963,#39964,#39965,
#39966,#39967,#39968,#39969,#39970,#39971,#39972,#39973,#39974,#39975),
(#39976,#39977,#39978,#39979,#39980,#39981,#39982,#39983,#39984,#39985,
#39986,#39987,#39988,#39989,#39990,#39991,#39992,#39993,#39994,#39995,#39996,
#39997,#39998,#39999,#40000,#40001,#40002,#40003,#40004,#40005,#40006,#40007,
#40008,#40009,#40010,#40011,#40012,#40013,#40014,#40015),(#40016,#40017,
#40018,#40019,#40020,#40021,#40022,#40023,#40024,#40025,#40026,#40027,#40028,
#40029,#40030,#40031,#40032,#40033,#40034,#40035,#40036,#40037,#40038,#40039,
#40040,#40041,#40042,#40043,#40044,#40045,#40046,#40047,#40048,#40049,#40050,
#40051,#40052,#40053,#40054,#40055),(#40056,#40057,#40058,#40059,#40060,
#40061,#40062,#40063,#40064,#40065,#40066,#40067,#40068,#40069,#40070,#40071,
#40072,#40073,#40074,#40075,#40076,#40077,#40078,#40079,#40080,#40081,#40082,
#40083,#40084,#40085,#40086,#40087,#40088,#40089,#40090,#40091,#40092,#40093,
#40094,#40095)),.UNSPECIFIED.,.F.,.F.,.F.,(4,1,4),(4,2,1,2,1,2,2,2,1,2,
1,1,1,1,1,1,2,1,2,1,1,1,2,1,1,1,1,1,4),(0.104020343629189,0.58528934430452,
0.946241094811018),(0.00211325483337195,0.100793262783688,0.184230802554962,
0.212043315812054,0.287954173261631,0.313257792411489,0.405143101782566,
0.488664067632647,0.526908077788674,0.565152087944702,0.569607108681037,
0.574062129417373,0.582972170890044,0.600792253835385,0.618612336780727,
0.627522378253398,0.636432419726069,0.65354858767753,0.704897091531912,
0.716247203396069,0.727597315260226,0.750297538988541,0.79569798644517,
0.806906221911025,0.81811445737688,0.840530928308591,0.851739163774446,
0.885363870172012,0.975029753898854),.UNSPECIFIED.);
#120=B_SPLINE_SURFACE_WITH_KNOTS('',3,3,((#40405,#40406,#40407,#40408,#40409,
#40410,#40411,#40412,#40413,#40414,#40415,#40416,#40417,#40418,#40419,#40420,
#40421,#40422,#40423,#40424,#40425,#40426,#40427,#40428,#40429,#40430,#40431,
#40432,#40433,#40434,#40435,#40436,#40437,#40438,#40439,#40440,#40441,#40442,
#40443,#40444),(#40445,#40446,#40447,#40448,#40449,#40450,#40451,#40452,
#40453,#40454,#40455,#40456,#40457,#40458,#40459,#40460,#40461,#40462,#40463,
#40464,#40465,#40466,#40467,#40468,#40469,#40470,#40471,#40472,#40473,#40474,
#40475,#40476,#40477,#40478,#40479,#40480,#40481,#40482,#40483,#40484),
(#40485,#40486,#40487,#40488,#40489,#40490,#40491,#40492,#40493,#40494,
#40495,#40496,#40497,#40498,#40499,#40500,#40501,#40502,#40503,#40504,#40505,
#40506,#40507,#40508,#40509,#40510,#40511,#40512,#40513,#40514,#40515,#40516,
#40517,#40518,#40519,#40520,#40521,#40522,#40523,#40524),(#40525,#40526,
#40527,#40528,#40529,#40530,#40531,#40532,#40533,#40534,#40535,#40536,#40537,
#40538,#40539,#40540,#40541,#40542,#40543,#40544,#40545,#40546,#40547,#40548,
#40549,#40550,#40551,#40552,#40553,#40554,#40555,#40556,#40557,#40558,#40559,
#40560,#40561,#40562,#40563,#40564),(#40565,#40566,#40567,#40568,#40569,
#40570,#40571,#40572,#40573,#40574,#40575,#40576,#40577,#40578,#40579,#40580,
#40581,#40582,#40583,#40584,#40585,#40586,#40587,#40588,#40589,#40590,#40591,
#40592,#40593,#40594,#40595,#40596,#40597,#40598,#40599,#40600,#40601,#40602,
#40603,#40604)),.UNSPECIFIED.,.F.,.F.,.F.,(4,1,4),(4,2,2,2,2,2,1,1,2,1,
1,1,1,1,1,2,1,2,1,1,1,1,2,1,1,1,1,1,4),(0.104020343629189,0.464972094135687,
0.946241094811018),(0.00211325483337195,0.100793262783688,0.212043315812054,
0.313257792411489,0.405143101782566,0.488664067632647,0.50778607271066,
0.526908077788674,0.565152087944702,0.569607108681037,0.574062129417373,
0.582972170890044,0.600792253835385,0.618612336780727,0.627522378253398,
0.636432419726069,0.670664755628991,0.704897091531912,0.71057214746399,
0.716247203396069,0.727597315260226,0.750297538988541,0.79569798644517,
0.806906221911025,0.81811445737688,0.840530928308591,0.862947399240301,
0.885363870172012,0.975029753898854),.UNSPECIFIED.);
#121=B_SPLINE_SURFACE_WITH_KNOTS('',3,3,((#40914,#40915,#40916,#40917,#40918,
#40919,#40920,#40921,#40922,#40923,#40924,#40925,#40926,#40927,#40928,#40929,
#40930,#40931,#40932,#40933,#40934,#40935,#40936,#40937,#40938,#40939,#40940,
#40941,#40942,#40943,#40944,#40945,#40946,#40947,#40948,#40949,#40950,#40951,
#40952,#40953,#40954,#40955),(#40956,#40957,#40958,#40959,#40960,#40961,
#40962,#40963,#40964,#40965,#40966,#40967,#40968,#40969,#40970,#40971,#40972,
#40973,#40974,#40975,#40976,#40977,#40978,#40979,#40980,#40981,#40982,#40983,
#40984,#40985,#40986,#40987,#40988,#40989,#40990,#40991,#40992,#40993,#40994,
#40995,#40996,#40997),(#40998,#40999,#41000,#41001,#41002,#41003,#41004,
#41005,#41006,#41007,#41008,#41009,#41010,#41011,#41012,#41013,#41014,#41015,
#41016,#41017,#41018,#41019,#41020,#41021,#41022,#41023,#41024,#41025,#41026,
#41027,#41028,#41029,#41030,#41031,#41032,#41033,#41034,#41035,#41036,#41037,
#41038,#41039),(#41040,#41041,#41042,#41043,#41044,#41045,#41046,#41047,
#41048,#41049,#41050,#41051,#41052,#41053,#41054,#41055,#41056,#41057,#41058,
#41059,#41060,#41061,#41062,#41063,#41064,#41065,#41066,#41067,#41068,#41069,
#41070,#41071,#41072,#41073,#41074,#41075,#41076,#41077,#41078,#41079,#41080,
#41081),(#41082,#41083,#41084,#41085,#41086,#41087,#41088,#41089,#41090,
#41091,#41092,#41093,#41094,#41095,#41096,#41097,#41098,#41099,#41100,#41101,
#41102,#41103,#41104,#41105,#41106,#41107,#41108,#41109,#41110,#41111,#41112,
#41113,#41114,#41115,#41116,#41117,#41118,#41119,#41120,#41121,#41122,#41123)),
 .UNSPECIFIED.,.F.,.F.,.F.,(4,1,4),(4,2,2,2,1,2,2,1,1,2,1,1,1,1,1,1,1,2,
1,2,1,1,1,1,2,1,1,1,1,1,4),(0.104020343629189,0.464972094135687,0.946241094811018),
(0.00211325483337195,0.100793262783688,0.212043315812054,0.313257792411489,
0.336229119754259,0.405143101782566,0.488664067632647,0.50778607271066,
0.526908077788674,0.565152087944702,0.582972170890044,0.600792253835385,
0.609702295308056,0.618612336780727,0.627522378253398,0.631977398989734,
0.634204909357901,0.636432419726069,0.670664755628991,0.704897091531912,
0.71057214746399,0.716247203396069,0.727597315260226,0.750297538988541,
0.79569798644517,0.806906221911025,0.81811445737688,0.840530928308591,0.862947399240301,
0.885363870172012,0.975029753898854),.UNSPECIFIED.);
#122=B_SPLINE_SURFACE_WITH_KNOTS('',3,3,((#41433,#41434,#41435,#41436,#41437,
#41438,#41439,#41440,#41441,#41442,#41443,#41444,#41445,#41446,#41447,#41448,
#41449,#41450,#41451,#41452,#41453,#41454,#41455,#41456,#41457,#41458,#41459,
#41460,#41461,#41462,#41463,#41464,#41465,#41466,#41467,#41468,#41469,#41470),
(#41471,#41472,#41473,#41474,#41475,#41476,#41477,#41478,#41479,#41480,
#41481,#41482,#41483,#41484,#41485,#41486,#41487,#41488,#41489,#41490,#41491,
#41492,#41493,#41494,#41495,#41496,#41497,#41498,#41499,#41500,#41501,#41502,
#41503,#41504,#41505,#41506,#41507,#41508),(#41509,#41510,#41511,#41512,
#41513,#41514,#41515,#41516,#41517,#41518,#41519,#41520,#41521,#41522,#41523,
#41524,#41525,#41526,#41527,#41528,#41529,#41530,#41531,#41532,#41533,#41534,
#41535,#41536,#41537,#41538,#41539,#41540,#41541,#41542,#41543,#41544,#41545,
#41546),(#41547,#41548,#41549,#41550,#41551,#41552,#41553,#41554,#41555,
#41556,#41557,#41558,#41559,#41560,#41561,#41562,#41563,#41564,#41565,#41566,
#41567,#41568,#41569,#41570,#41571,#41572,#41573,#41574,#41575,#41576,#41577,
#41578,#41579,#41580,#41581,#41582,#41583,#41584),(#41585,#41586,#41587,
#41588,#41589,#41590,#41591,#41592,#41593,#41594,#41595,#41596,#41597,#41598,
#41599,#41600,#41601,#41602,#41603,#41604,#41605,#41606,#41607,#41608,#41609,
#41610,#41611,#41612,#41613,#41614,#41615,#41616,#41617,#41618,#41619,#41620,
#41621,#41622)),.UNSPECIFIED.,.F.,.F.,.F.,(4,1,4),(4,2,2,2,1,2,2,1,2,1,
1,1,1,1,2,1,2,1,1,1,2,1,1,1,1,1,4),(0.104020343629189,0.464972094135687,
0.946241094811018),(0.00211325483337195,0.100793262783688,0.212043315812054,
0.313257792411489,0.336229119754259,0.405143101782566,0.488664067632647,
0.526908077788674,0.565152087944702,0.569607108681037,0.574062129417373,
0.582972170890044,0.600792253835385,0.618612336780727,0.636432419726069,
0.65354858767753,0.704897091531912,0.716247203396069,0.727597315260226,
0.750297538988541,0.79569798644517,0.806906221911025,0.81811445737688,0.840530928308591,
0.851739163774446,0.885363870172012,0.975029753898854),.UNSPECIFIED.);
#123=B_SPLINE_SURFACE_WITH_KNOTS('',3,3,((#41716,#41717,#41718,#41719,#41720,
#41721,#41722,#41723,#41724,#41725,#41726,#41727,#41728,#41729,#41730,#41731,
#41732),(#41733,#41734,#41735,#41736,#41737,#41738,#41739,#41740,#41741,
#41742,#41743,#41744,#41745,#41746,#41747,#41748,#41749),(#41750,#41751,
#41752,#41753,#41754,#41755,#41756,#41757,#41758,#41759,#41760,#41761,#41762,
#41763,#41764,#41765,#41766),(#41767,#41768,#41769,#41770,#41771,#41772,
#41773,#41774,#41775,#41776,#41777,#41778,#41779,#41780,#41781,#41782,#41783)),
 .UNSPECIFIED.,.F.,.F.,.F.,(4,4),(4,1,1,1,1,1,1,1,1,1,1,1,1,1,4),(0.,1.),
(0.,0.0714285714285714,0.142857142857143,0.214285714285714,0.285714285714286,
0.357142857142857,0.428571428571429,0.476190476190476,0.571428571428571,
0.619047619047619,0.714285714285714,0.785714285714286,0.857142857142857,
0.928571428571429,1.),.UNSPECIFIED.);
#124=B_SPLINE_SURFACE_WITH_KNOTS('',3,3,((#42606,#42607,#42608,#42609,#42610,
#42611,#42612,#42613,#42614,#42615,#42616,#42617,#42618,#42619,#42620,#42621,
#42622),(#42623,#42624,#42625,#42626,#42627,#42628,#42629,#42630,#42631,
#42632,#42633,#42634,#42635,#42636,#42637,#42638,#42639),(#42640,#42641,
#42642,#42643,#42644,#42645,#42646,#42647,#42648,#42649,#42650,#42651,#42652,
#42653,#42654,#42655,#42656),(#42657,#42658,#42659,#42660,#42661,#42662,
#42663,#42664,#42665,#42666,#42667,#42668,#42669,#42670,#42671,#42672,#42673)),
 .UNSPECIFIED.,.F.,.F.,.F.,(4,4),(4,1,1,1,1,1,1,1,1,1,1,1,1,1,4),(0.,1.),
(-3.39227166254691E-15,0.071428563366594,0.142857126733191,0.214285690099789,
0.285714253466386,0.380952337955183,0.428571380199581,0.523809464688377,
0.571428506932776,0.642857070299373,0.71428563366597,0.785714197032568,
0.857142760399165,0.928571323765762,0.99999988713236),.UNSPECIFIED.);
#125=B_SPLINE_SURFACE_WITH_KNOTS('',3,3,((#42696,#42697,#42698,#42699,#42700,
#42701,#42702,#42703,#42704,#42705,#42706,#42707,#42708,#42709,#42710,#42711),
(#42712,#42713,#42714,#42715,#42716,#42717,#42718,#42719,#42720,#42721,
#42722,#42723,#42724,#42725,#42726,#42727),(#42728,#42729,#42730,#42731,
#42732,#42733,#42734,#42735,#42736,#42737,#42738,#42739,#42740,#42741,#42742,
#42743),(#42744,#42745,#42746,#42747,#42748,#42749,#42750,#42751,#42752,
#42753,#42754,#42755,#42756,#42757,#42758,#42759),(#42760,#42761,#42762,
#42763,#42764,#42765,#42766,#42767,#42768,#42769,#42770,#42771,#42772,#42773,
#42774,#42775),(#42776,#42777,#42778,#42779,#42780,#42781,#42782,#42783,
#42784,#42785,#42786,#42787,#42788,#42789,#42790,#42791),(#42792,#42793,
#42794,#42795,#42796,#42797,#42798,#42799,#42800,#42801,#42802,#42803,#42804,
#42805,#42806,#42807),(#42808,#42809,#42810,#42811,#42812,#42813,#42814,
#42815,#42816,#42817,#42818,#42819,#42820,#42821,#42822,#42823),(#42824,
#42825,#42826,#42827,#42828,#42829,#42830,#42831,#42832,#42833,#42834,#42835,
#42836,#42837,#42838,#42839)),.UNSPECIFIED.,.F.,.F.,.F.,(4,1,1,1,1,1,4),
(4,1,1,1,1,1,1,1,1,1,1,1,1,4),(0.,0.0357142857142857,0.0714285714285714,
0.107142857142857,0.142857142857143,0.285714285714286,1.),(-1.31922727866773E-7,
0.0444444444444444,0.114351851851852,0.184259259259259,0.254166666666666,
0.324074074074073,0.39398148148148,0.463888888888888,0.55324074074074,0.642592592592592,
0.731944444444444,0.821296296296296,0.910648148148148,1.),.UNSPECIFIED.);
#126=B_SPLINE_SURFACE_WITH_KNOTS('',3,3,((#43632,#43633,#43634,#43635,#43636,
#43637,#43638,#43639,#43640,#43641,#43642,#43643,#43644,#43645,#43646,#43647,
#43648),(#43649,#43650,#43651,#43652,#43653,#43654,#43655,#43656,#43657,
#43658,#43659,#43660,#43661,#43662,#43663,#43664,#43665),(#43666,#43667,
#43668,#43669,#43670,#43671,#43672,#43673,#43674,#43675,#43676,#43677,#43678,
#43679,#43680,#43681,#43682),(#43683,#43684,#43685,#43686,#43687,#43688,
#43689,#43690,#43691,#43692,#43693,#43694,#43695,#43696,#43697,#43698,#43699)),
 .UNSPECIFIED.,.F.,.F.,.F.,(4,4),(4,1,1,1,1,1,1,1,1,1,1,1,1,1,4),(0.,1.),
(-1.31922727866773E-7,0.0305555555555556,0.0444444444444444,0.114351851851852,
0.184259259259259,0.254166666666666,0.324074074074073,0.39398148148148,
0.463888888888888,0.55324074074074,0.642592592592592,0.731944444444444,
0.821296296296296,0.910648148148148,1.),.UNSPECIFIED.);
#127=B_SPLINE_SURFACE_WITH_KNOTS('',3,3,((#45073,#45074,#45075,#45076,#45077,
#45078,#45079,#45080,#45081,#45082,#45083,#45084,#45085,#45086),(#45087,
#45088,#45089,#45090,#45091,#45092,#45093,#45094,#45095,#45096,#45097,#45098,
#45099,#45100),(#45101,#45102,#45103,#45104,#45105,#45106,#45107,#45108,
#45109,#45110,#45111,#45112,#45113,#45114),(#45115,#45116,#45117,#45118,
#45119,#45120,#45121,#45122,#45123,#45124,#45125,#45126,#45127,#45128)),
 .UNSPECIFIED.,.F.,.F.,.F.,(4,4),(4,1,1,1,1,1,1,1,1,1,1,4),(0.,1.),(-3.29679099043599E-16,
0.0888888888888885,0.177777777777777,0.266666666666666,0.275,0.389814814814814,
0.504629629629628,0.619444444444443,0.744444444444442,0.829629629629628,
0.914814814814814,1.),.UNSPECIFIED.);
#128=B_SPLINE_SURFACE_WITH_KNOTS('',3,3,((#45942,#45943,#45944,#45945,#45946,
#45947,#45948,#45949,#45950,#45951,#45952,#45953,#45954,#45955),(#45956,
#45957,#45958,#45959,#45960,#45961,#45962,#45963,#45964,#45965,#45966,#45967,
#45968,#45969),(#45970,#45971,#45972,#45973,#45974,#45975,#45976,#45977,
#45978,#45979,#45980,#45981,#45982,#45983),(#45984,#45985,#45986,#45987,
#45988,#45989,#45990,#45991,#45992,#45993,#45994,#45995,#45996,#45997)),
 .UNSPECIFIED.,.F.,.F.,.F.,(4,4),(4,1,1,1,1,1,1,1,1,1,1,4),(0.,1.),(-4.77815499535063E-15,
0.0888888888888856,0.177777777777776,0.266666666666666,0.275,0.389814814814814,
0.504629629629628,0.619444444444443,0.744444444444442,0.829629584919082,
0.914814725393722,0.999999865868361),.UNSPECIFIED.);
#129=B_SPLINE_SURFACE_WITH_KNOTS('',3,3,((#46017,#46018,#46019,#46020,#46021,
#46022,#46023,#46024,#46025,#46026,#46027,#46028,#46029,#46030,#46031,#46032,
#46033,#46034,#46035,#46036,#46037,#46038,#46039,#46040,#46041,#46042),
(#46043,#46044,#46045,#46046,#46047,#46048,#46049,#46050,#46051,#46052,
#46053,#46054,#46055,#46056,#46057,#46058,#46059,#46060,#46061,#46062,#46063,
#46064,#46065,#46066,#46067,#46068),(#46069,#46070,#46071,#46072,#46073,
#46074,#46075,#46076,#46077,#46078,#46079,#46080,#46081,#46082,#46083,#46084,
#46085,#46086,#46087,#46088,#46089,#46090,#46091,#46092,#46093,#46094),
(#46095,#46096,#46097,#46098,#46099,#46100,#46101,#46102,#46103,#46104,
#46105,#46106,#46107,#46108,#46109,#46110,#46111,#46112,#46113,#46114,#46115,
#46116,#46117,#46118,#46119,#46120)),.UNSPECIFIED.,.F.,.F.,.F.,(4,4),(4,
1,1,1,1,1,1,1,1,1,1,1,1,1,1,1,1,1,1,1,1,1,1,4),(0.,1.),(-1.52611180263545E-7,
0.00277777777777778,0.05,0.102777777777778,0.105555555555556,0.130555555555556,
0.147222222222222,0.15,0.158333333333333,0.218055555555555,0.277777777777777,
0.36111111111111,0.433333333333332,0.466666666666666,0.547222222222221,
0.644444444444443,0.658333333333332,0.686111111111109,0.688888888888887,
0.744444444444442,0.856944444444442,0.969444444444442,0.988888888888886,
1.),.UNSPECIFIED.);
#130=B_SPLINE_SURFACE_WITH_KNOTS('',3,3,((#46935,#46936,#46937,#46938,#46939,
#46940,#46941,#46942,#46943,#46944,#46945,#46946,#46947,#46948,#46949,#46950,
#46951,#46952,#46953,#46954,#46955,#46956,#46957,#46958),(#46959,#46960,
#46961,#46962,#46963,#46964,#46965,#46966,#46967,#46968,#46969,#46970,#46971,
#46972,#46973,#46974,#46975,#46976,#46977,#46978,#46979,#46980,#46981,#46982),
(#46983,#46984,#46985,#46986,#46987,#46988,#46989,#46990,#46991,#46992,
#46993,#46994,#46995,#46996,#46997,#46998,#46999,#47000,#47001,#47002,#47003,
#47004,#47005,#47006),(#47007,#47008,#47009,#47010,#47011,#47012,#47013,
#47014,#47015,#47016,#47017,#47018,#47019,#47020,#47021,#47022,#47023,#47024,
#47025,#47026,#47027,#47028,#47029,#47030)),.UNSPECIFIED.,.F.,.F.,.F.,(4,
4),(4,1,1,1,1,1,1,1,1,1,1,1,1,1,1,1,1,1,1,1,1,4),(0.,1.),(-1.52611180304074E-7,
0.05,0.0527777777777778,0.105555555555556,0.147222222222222,0.15,0.158333333333333,
0.218055555555555,0.277777777777777,0.36111111111111,0.433333333333332,
0.466666666666666,0.547222222222221,0.644444444444443,0.658333333333332,
0.686111111111109,0.688888888888887,0.744444444444442,0.856944444444442,
0.969444444444442,0.988888888888886,1.),.UNSPECIFIED.);
#131=B_SPLINE_SURFACE_WITH_KNOTS('',3,3,((#48070,#48071,#48072,#48073,#48074,
#48075,#48076,#48077,#48078,#48079,#48080,#48081,#48082,#48083,#48084,#48085,
#48086,#48087,#48088,#48089,#48090,#48091,#48092,#48093,#48094,#48095,#48096),
(#48097,#48098,#48099,#48100,#48101,#48102,#48103,#48104,#48105,#48106,
#48107,#48108,#48109,#48110,#48111,#48112,#48113,#48114,#48115,#48116,#48117,
#48118,#48119,#48120,#48121,#48122,#48123),(#48124,#48125,#48126,#48127,
#48128,#48129,#48130,#48131,#48132,#48133,#48134,#48135,#48136,#48137,#48138,
#48139,#48140,#48141,#48142,#48143,#48144,#48145,#48146,#48147,#48148,#48149,
#48150),(#48151,#48152,#48153,#48154,#48155,#48156,#48157,#48158,#48159,
#48160,#48161,#48162,#48163,#48164,#48165,#48166,#48167,#48168,#48169,#48170,
#48171,#48172,#48173,#48174,#48175,#48176,#48177)),.UNSPECIFIED.,.F.,.F.,
 .F.,(4,4),(4,2,1,1,1,2,1,1,1,1,1,1,2,1,1,1,1,1,2,1,4),(0.266176291422809,
0.969386396335851),(0.0275328340336186,0.114720141806747,0.131928163077759,
0.149136184348771,0.183552226890795,0.252384311974843,0.26119115197838,
0.269997991981918,0.287611671988993,0.305225351996068,0.322839032003143,
0.358066392017293,0.393293752031443,0.516081621889917,0.536546266866329,
0.546778589354535,0.551894750598638,0.55445283122069,0.557010911842741,
0.604124367076873,0.651237822311005),.UNSPECIFIED.);
#132=B_SPLINE_SURFACE_WITH_KNOTS('',3,3,((#48414,#48415,#48416,#48417,#48418,
#48419,#48420,#48421,#48422,#48423,#48424,#48425,#48426,#48427,#48428,#48429,
#48430,#48431,#48432,#48433,#48434,#48435,#48436,#48437,#48438),(#48439,
#48440,#48441,#48442,#48443,#48444,#48445,#48446,#48447,#48448,#48449,#48450,
#48451,#48452,#48453,#48454,#48455,#48456,#48457,#48458,#48459,#48460,#48461,
#48462,#48463),(#48464,#48465,#48466,#48467,#48468,#48469,#48470,#48471,
#48472,#48473,#48474,#48475,#48476,#48477,#48478,#48479,#48480,#48481,#48482,
#48483,#48484,#48485,#48486,#48487,#48488),(#48489,#48490,#48491,#48492,
#48493,#48494,#48495,#48496,#48497,#48498,#48499,#48500,#48501,#48502,#48503,
#48504,#48505,#48506,#48507,#48508,#48509,#48510,#48511,#48512,#48513)),
 .UNSPECIFIED.,.F.,.F.,.F.,(4,4),(4,2,1,1,2,1,1,1,1,1,1,2,1,1,1,2,1,1,4),
(0.266100373933286,0.969385828517312),(0.0275328340336185,0.114720141806747,
0.149136184348771,0.183552226890795,0.252384311974843,0.26119115197838,
0.269997991981918,0.287611671988993,0.305225351996068,0.322839032003143,
0.340452712010218,0.393293752031443,0.475152331937092,0.516081621889917,
0.536546266866329,0.557010911842741,0.602472788890741,0.647934665938741,
0.738858420034741),.UNSPECIFIED.);
#133=B_SPLINE_SURFACE_WITH_KNOTS('',3,3,((#48540,#48541,#48542,#48543,#48544,
#48545,#48546,#48547,#48548,#48549,#48550,#48551,#48552,#48553,#48554,#48555,
#48556,#48557,#48558,#48559,#48560,#48561,#48562,#48563,#48564,#48565,#48566),
(#48567,#48568,#48569,#48570,#48571,#48572,#48573,#48574,#48575,#48576,
#48577,#48578,#48579,#48580,#48581,#48582,#48583,#48584,#48585,#48586,#48587,
#48588,#48589,#48590,#48591,#48592,#48593),(#48594,#48595,#48596,#48597,
#48598,#48599,#48600,#48601,#48602,#48603,#48604,#48605,#48606,#48607,#48608,
#48609,#48610,#48611,#48612,#48613,#48614,#48615,#48616,#48617,#48618,#48619,
#48620),(#48621,#48622,#48623,#48624,#48625,#48626,#48627,#48628,#48629,
#48630,#48631,#48632,#48633,#48634,#48635,#48636,#48637,#48638,#48639,#48640,
#48641,#48642,#48643,#48644,#48645,#48646,#48647)),.UNSPECIFIED.,.F.,.F.,
 .F.,(4,4),(4,2,1,1,1,2,1,1,1,1,1,1,2,1,1,1,1,1,2,1,4),(0.266176291422809,
0.969386396335851),(0.0275328340336186,0.114720141806747,0.131928163077759,
0.149136184348771,0.183552226890795,0.252384311974843,0.26119115197838,
0.269997991981918,0.287611671988993,0.305225351996068,0.322839032003143,
0.358066392017293,0.393293752031443,0.516081621889917,0.536546266866329,
0.546778589354535,0.551894750598638,0.55445283122069,0.557010911842741,
0.604124367076873,0.651237822311005),.UNSPECIFIED.);
#134=B_SPLINE_SURFACE_WITH_KNOTS('',3,3,((#48884,#48885,#48886,#48887,#48888,
#48889,#48890,#48891,#48892,#48893,#48894,#48895,#48896,#48897,#48898,#48899,
#48900,#48901,#48902,#48903,#48904,#48905,#48906,#48907,#48908),(#48909,
#48910,#48911,#48912,#48913,#48914,#48915,#48916,#48917,#48918,#48919,#48920,
#48921,#48922,#48923,#48924,#48925,#48926,#48927,#48928,#48929,#48930,#48931,
#48932,#48933),(#48934,#48935,#48936,#48937,#48938,#48939,#48940,#48941,
#48942,#48943,#48944,#48945,#48946,#48947,#48948,#48949,#48950,#48951,#48952,
#48953,#48954,#48955,#48956,#48957,#48958),(#48959,#48960,#48961,#48962,
#48963,#48964,#48965,#48966,#48967,#48968,#48969,#48970,#48971,#48972,#48973,
#48974,#48975,#48976,#48977,#48978,#48979,#48980,#48981,#48982,#48983)),
 .UNSPECIFIED.,.F.,.F.,.F.,(4,4),(4,2,1,1,2,1,1,1,1,1,1,2,1,1,1,2,1,1,4),
(0.266100373933286,0.969385828517312),(0.0275328340336192,0.114720141806747,
0.149136184348771,0.183552226890795,0.252384311974843,0.26119115197838,
0.269997991981918,0.287611671988993,0.305225351996068,0.322839032003143,
0.340452712010218,0.393293752031443,0.475152331937092,0.516081621889917,
0.536546266866329,0.557010911842741,0.602472788890741,0.647934665938741,
0.738858420034741),.UNSPECIFIED.);
#135=B_SPLINE_SURFACE_WITH_KNOTS('',3,3,((#49010,#49011,#49012,#49013,#49014,
#49015,#49016,#49017,#49018,#49019,#49020,#49021,#49022,#49023,#49024,#49025,
#49026,#49027,#49028,#49029,#49030,#49031,#49032,#49033,#49034,#49035,#49036),
(#49037,#49038,#49039,#49040,#49041,#49042,#49043,#49044,#49045,#49046,
#49047,#49048,#49049,#49050,#49051,#49052,#49053,#49054,#49055,#49056,#49057,
#49058,#49059,#49060,#49061,#49062,#49063),(#49064,#49065,#49066,#49067,
#49068,#49069,#49070,#49071,#49072,#49073,#49074,#49075,#49076,#49077,#49078,
#49079,#49080,#49081,#49082,#49083,#49084,#49085,#49086,#49087,#49088,#49089,
#49090),(#49091,#49092,#49093,#49094,#49095,#49096,#49097,#49098,#49099,
#49100,#49101,#49102,#49103,#49104,#49105,#49106,#49107,#49108,#49109,#49110,
#49111,#49112,#49113,#49114,#49115,#49116,#49117)),.UNSPECIFIED.,.F.,.F.,
 .F.,(4,4),(4,2,1,1,1,2,1,1,1,1,1,1,2,1,1,1,1,1,2,1,4),(0.266176291422809,
0.969386396335851),(0.0275328340336192,0.114720141806747,0.131928163077759,
0.149136184348771,0.183552226890795,0.252384311974843,0.26119115197838,
0.269997991981918,0.287611671988993,0.305225351996068,0.322839032003143,
0.358066392017293,0.393293752031443,0.516081621889917,0.536546266866329,
0.546778589354535,0.551894750598638,0.55445283122069,0.557010911842741,
0.604124367076873,0.651237822311005),.UNSPECIFIED.);
#136=B_SPLINE_SURFACE_WITH_KNOTS('',3,3,((#49354,#49355,#49356,#49357,#49358,
#49359,#49360,#49361,#49362,#49363,#49364,#49365,#49366,#49367,#49368,#49369,
#49370,#49371,#49372,#49373,#49374,#49375,#49376,#49377,#49378),(#49379,
#49380,#49381,#49382,#49383,#49384,#49385,#49386,#49387,#49388,#49389,#49390,
#49391,#49392,#49393,#49394,#49395,#49396,#49397,#49398,#49399,#49400,#49401,
#49402,#49403),(#49404,#49405,#49406,#49407,#49408,#49409,#49410,#49411,
#49412,#49413,#49414,#49415,#49416,#49417,#49418,#49419,#49420,#49421,#49422,
#49423,#49424,#49425,#49426,#49427,#49428),(#49429,#49430,#49431,#49432,
#49433,#49434,#49435,#49436,#49437,#49438,#49439,#49440,#49441,#49442,#49443,
#49444,#49445,#49446,#49447,#49448,#49449,#49450,#49451,#49452,#49453)),
 .UNSPECIFIED.,.F.,.F.,.F.,(4,4),(4,2,1,1,2,1,1,1,1,1,1,2,1,1,1,2,1,1,4),
(0.266100373933287,0.969385828517312),(0.0275328340336187,0.114720141806747,
0.149136184348771,0.183552226890795,0.252384311974843,0.26119115197838,
0.269997991981918,0.287611671988993,0.305225351996068,0.322839032003143,
0.340452712010218,0.393293752031443,0.475152331937092,0.516081621889917,
0.536546266866329,0.557010911842741,0.602472788890741,0.647934665938741,
0.738858420034741),.UNSPECIFIED.);
#137=B_SPLINE_SURFACE_WITH_KNOTS('',3,3,((#49480,#49481,#49482,#49483,#49484,
#49485,#49486,#49487,#49488,#49489,#49490,#49491,#49492,#49493,#49494,#49495,
#49496,#49497,#49498,#49499,#49500,#49501,#49502,#49503,#49504,#49505,#49506),
(#49507,#49508,#49509,#49510,#49511,#49512,#49513,#49514,#49515,#49516,
#49517,#49518,#49519,#49520,#49521,#49522,#49523,#49524,#49525,#49526,#49527,
#49528,#49529,#49530,#49531,#49532,#49533),(#49534,#49535,#49536,#49537,
#49538,#49539,#49540,#49541,#49542,#49543,#49544,#49545,#49546,#49547,#49548,
#49549,#49550,#49551,#49552,#49553,#49554,#49555,#49556,#49557,#49558,#49559,
#49560),(#49561,#49562,#49563,#49564,#49565,#49566,#49567,#49568,#49569,
#49570,#49571,#49572,#49573,#49574,#49575,#49576,#49577,#49578,#49579,#49580,
#49581,#49582,#49583,#49584,#49585,#49586,#49587)),.UNSPECIFIED.,.F.,.F.,
 .F.,(4,4),(4,2,1,1,1,2,1,1,1,1,1,1,2,1,1,1,1,1,2,1,4),(0.266176291422809,
0.969386396335851),(0.0275328340336192,0.114720141806747,0.131928163077759,
0.149136184348771,0.183552226890795,0.252384311974843,0.26119115197838,
0.269997991981918,0.287611671988993,0.305225351996068,0.322839032003143,
0.358066392017293,0.393293752031443,0.516081621889917,0.536546266866329,
0.546778589354535,0.551894750598638,0.55445283122069,0.557010911842741,
0.604124367076873,0.651237822311005),.UNSPECIFIED.);
#138=B_SPLINE_SURFACE_WITH_KNOTS('',3,3,((#49826,#49827,#49828,#49829,#49830,
#49831,#49832,#49833,#49834,#49835,#49836,#49837,#49838,#49839,#49840,#49841,
#49842,#49843,#49844,#49845,#49846,#49847,#49848,#49849,#49850),(#49851,
#49852,#49853,#49854,#49855,#49856,#49857,#49858,#49859,#49860,#49861,#49862,
#49863,#49864,#49865,#49866,#49867,#49868,#49869,#49870,#49871,#49872,#49873,
#49874,#49875),(#49876,#49877,#49878,#49879,#49880,#49881,#49882,#49883,
#49884,#49885,#49886,#49887,#49888,#49889,#49890,#49891,#49892,#49893,#49894,
#49895,#49896,#49897,#49898,#49899,#49900),(#49901,#49902,#49903,#49904,
#49905,#49906,#49907,#49908,#49909,#49910,#49911,#49912,#49913,#49914,#49915,
#49916,#49917,#49918,#49919,#49920,#49921,#49922,#49923,#49924,#49925)),
 .UNSPECIFIED.,.F.,.F.,.F.,(4,4),(4,2,1,1,2,1,1,1,1,1,1,2,1,1,1,2,1,1,4),
(0.266100373933287,0.969385828517312),(0.0275328340336186,0.114720141806747,
0.149136184348771,0.183552226890795,0.252384311974843,0.26119115197838,
0.269997991981918,0.287611671988993,0.305225351996068,0.322839032003143,
0.340452712010218,0.393293752031443,0.475152331937092,0.516081621889917,
0.536546266866329,0.557010911842741,0.602472788890741,0.647934665938741,
0.738858420034741),.UNSPECIFIED.);
#139=B_SPLINE_SURFACE_WITH_KNOTS('',3,3,((#49952,#49953,#49954,#49955,#49956,
#49957,#49958,#49959,#49960,#49961,#49962,#49963,#49964,#49965,#49966,#49967,
#49968,#49969,#49970,#49971,#49972,#49973,#49974,#49975,#49976,#49977,#49978),
(#49979,#49980,#49981,#49982,#49983,#49984,#49985,#49986,#49987,#49988,
#49989,#49990,#49991,#49992,#49993,#49994,#49995,#49996,#49997,#49998,#49999,
#50000,#50001,#50002,#50003,#50004,#50005),(#50006,#50007,#50008,#50009,
#50010,#50011,#50012,#50013,#50014,#50015,#50016,#50017,#50018,#50019,#50020,
#50021,#50022,#50023,#50024,#50025,#50026,#50027,#50028,#50029,#50030,#50031,
#50032),(#50033,#50034,#50035,#50036,#50037,#50038,#50039,#50040,#50041,
#50042,#50043,#50044,#50045,#50046,#50047,#50048,#50049,#50050,#50051,#50052,
#50053,#50054,#50055,#50056,#50057,#50058,#50059)),.UNSPECIFIED.,.F.,.F.,
 .F.,(4,4),(4,2,1,1,1,2,1,1,1,1,1,1,2,1,1,1,1,1,2,1,4),(0.266176291422809,
0.969386396335851),(0.0275328340336195,0.114720141806747,0.131928163077759,
0.149136184348771,0.183552226890795,0.252384311974843,0.26119115197838,
0.269997991981918,0.287611671988993,0.305225351996068,0.322839032003143,
0.358066392017293,0.393293752031443,0.516081621889917,0.536546266866329,
0.546778589354535,0.551894750598638,0.55445283122069,0.557010911842741,
0.604124367076873,0.651237822311005),.UNSPECIFIED.);
#140=B_SPLINE_SURFACE_WITH_KNOTS('',3,3,((#50298,#50299,#50300,#50301,#50302,
#50303,#50304,#50305,#50306,#50307,#50308,#50309,#50310,#50311,#50312,#50313,
#50314,#50315,#50316,#50317,#50318,#50319,#50320,#50321,#50322),(#50323,
#50324,#50325,#50326,#50327,#50328,#50329,#50330,#50331,#50332,#50333,#50334,
#50335,#50336,#50337,#50338,#50339,#50340,#50341,#50342,#50343,#50344,#50345,
#50346,#50347),(#50348,#50349,#50350,#50351,#50352,#50353,#50354,#50355,
#50356,#50357,#50358,#50359,#50360,#50361,#50362,#50363,#50364,#50365,#50366,
#50367,#50368,#50369,#50370,#50371,#50372),(#50373,#50374,#50375,#50376,
#50377,#50378,#50379,#50380,#50381,#50382,#50383,#50384,#50385,#50386,#50387,
#50388,#50389,#50390,#50391,#50392,#50393,#50394,#50395,#50396,#50397)),
 .UNSPECIFIED.,.F.,.F.,.F.,(4,4),(4,2,1,1,2,1,1,1,1,1,1,2,1,1,1,2,1,1,4),
(0.266100373933287,0.969385828517312),(0.0275328340336187,0.114720141806747,
0.149136184348771,0.183552226890795,0.252384311974843,0.26119115197838,
0.269997991981918,0.287611671988993,0.305225351996068,0.322839032003143,
0.340452712010218,0.393293752031443,0.475152331937092,0.516081621889917,
0.536546266866329,0.557010911842741,0.602472788890741,0.647934665938741,
0.738858420034741),.UNSPECIFIED.);
#141=B_SPLINE_SURFACE_WITH_KNOTS('',3,3,((#50424,#50425,#50426,#50427,#50428,
#50429,#50430,#50431,#50432,#50433,#50434,#50435,#50436,#50437,#50438,#50439,
#50440,#50441,#50442,#50443,#50444,#50445,#50446,#50447,#50448,#50449,#50450),
(#50451,#50452,#50453,#50454,#50455,#50456,#50457,#50458,#50459,#50460,
#50461,#50462,#50463,#50464,#50465,#50466,#50467,#50468,#50469,#50470,#50471,
#50472,#50473,#50474,#50475,#50476,#50477),(#50478,#50479,#50480,#50481,
#50482,#50483,#50484,#50485,#50486,#50487,#50488,#50489,#50490,#50491,#50492,
#50493,#50494,#50495,#50496,#50497,#50498,#50499,#50500,#50501,#50502,#50503,
#50504),(#50505,#50506,#50507,#50508,#50509,#50510,#50511,#50512,#50513,
#50514,#50515,#50516,#50517,#50518,#50519,#50520,#50521,#50522,#50523,#50524,
#50525,#50526,#50527,#50528,#50529,#50530,#50531)),.UNSPECIFIED.,.F.,.F.,
 .F.,(4,4),(4,2,1,1,1,2,1,1,1,1,1,1,2,1,1,1,1,1,2,1,4),(0.266176291422809,
0.969386396335851),(0.0275328340336193,0.114720141806747,0.131928163077759,
0.149136184348771,0.183552226890795,0.252384311974843,0.26119115197838,
0.269997991981918,0.287611671988993,0.305225351996068,0.322839032003143,
0.358066392017293,0.393293752031443,0.516081621889917,0.536546266866329,
0.546778589354535,0.551894750598638,0.55445283122069,0.557010911842741,
0.604124367076873,0.651237822311005),.UNSPECIFIED.);
#142=B_SPLINE_SURFACE_WITH_KNOTS('',3,3,((#50768,#50769,#50770,#50771,#50772,
#50773,#50774,#50775,#50776,#50777,#50778,#50779,#50780,#50781,#50782,#50783,
#50784,#50785,#50786,#50787,#50788,#50789,#50790,#50791,#50792),(#50793,
#50794,#50795,#50796,#50797,#50798,#50799,#50800,#50801,#50802,#50803,#50804,
#50805,#50806,#50807,#50808,#50809,#50810,#50811,#50812,#50813,#50814,#50815,
#50816,#50817),(#50818,#50819,#50820,#50821,#50822,#50823,#50824,#50825,
#50826,#50827,#50828,#50829,#50830,#50831,#50832,#50833,#50834,#50835,#50836,
#50837,#50838,#50839,#50840,#50841,#50842),(#50843,#50844,#50845,#50846,
#50847,#50848,#50849,#50850,#50851,#50852,#50853,#50854,#50855,#50856,#50857,
#50858,#50859,#50860,#50861,#50862,#50863,#50864,#50865,#50866,#50867)),
 .UNSPECIFIED.,.F.,.F.,.F.,(4,4),(4,2,1,1,2,1,1,1,1,1,1,2,1,1,1,2,1,1,4),
(0.266100373933286,0.969385828517312),(0.0275328340336187,0.114720141806747,
0.149136184348771,0.183552226890795,0.252384311974843,0.26119115197838,
0.269997991981918,0.287611671988993,0.305225351996068,0.322839032003143,
0.340452712010218,0.393293752031443,0.475152331937092,0.516081621889917,
0.536546266866329,0.557010911842741,0.602472788890741,0.647934665938741,
0.738858420034741),.UNSPECIFIED.);
#143=B_SPLINE_SURFACE_WITH_KNOTS('',3,3,((#50894,#50895,#50896,#50897,#50898,
#50899,#50900,#50901,#50902,#50903,#50904,#50905,#50906,#50907,#50908,#50909,
#50910,#50911,#50912,#50913,#50914,#50915,#50916,#50917,#50918,#50919,#50920),
(#50921,#50922,#50923,#50924,#50925,#50926,#50927,#50928,#50929,#50930,
#50931,#50932,#50933,#50934,#50935,#50936,#50937,#50938,#50939,#50940,#50941,
#50942,#50943,#50944,#50945,#50946,#50947),(#50948,#50949,#50950,#50951,
#50952,#50953,#50954,#50955,#50956,#50957,#50958,#50959,#50960,#50961,#50962,
#50963,#50964,#50965,#50966,#50967,#50968,#50969,#50970,#50971,#50972,#50973,
#50974),(#50975,#50976,#50977,#50978,#50979,#50980,#50981,#50982,#50983,
#50984,#50985,#50986,#50987,#50988,#50989,#50990,#50991,#50992,#50993,#50994,
#50995,#50996,#50997,#50998,#50999,#51000,#51001)),.UNSPECIFIED.,.F.,.F.,
 .F.,(4,4),(4,2,1,1,1,2,1,1,1,1,1,1,2,1,1,1,1,1,2,1,4),(0.266176291422809,
0.969386396335851),(0.0275328340336186,0.114720141806747,0.131928163077759,
0.149136184348771,0.183552226890795,0.252384311974843,0.26119115197838,
0.269997991981918,0.287611671988993,0.305225351996068,0.322839032003143,
0.358066392017293,0.393293752031443,0.516081621889917,0.536546266866329,
0.546778589354535,0.551894750598638,0.55445283122069,0.557010911842741,
0.604124367076873,0.651237822311005),.UNSPECIFIED.);
#144=B_SPLINE_SURFACE_WITH_KNOTS('',3,3,((#51203,#51204,#51205,#51206,#51207,
#51208,#51209,#51210,#51211,#51212,#51213,#51214,#51215,#51216,#51217,#51218,
#51219,#51220,#51221,#51222,#51223,#51224,#51225,#51226,#51227),(#51228,
#51229,#51230,#51231,#51232,#51233,#51234,#51235,#51236,#51237,#51238,#51239,
#51240,#51241,#51242,#51243,#51244,#51245,#51246,#51247,#51248,#51249,#51250,
#51251,#51252),(#51253,#51254,#51255,#51256,#51257,#51258,#51259,#51260,
#51261,#51262,#51263,#51264,#51265,#51266,#51267,#51268,#51269,#51270,#51271,
#51272,#51273,#51274,#51275,#51276,#51277),(#51278,#51279,#51280,#51281,
#51282,#51283,#51284,#51285,#51286,#51287,#51288,#51289,#51290,#51291,#51292,
#51293,#51294,#51295,#51296,#51297,#51298,#51299,#51300,#51301,#51302)),
 .UNSPECIFIED.,.F.,.F.,.F.,(4,4),(4,2,1,1,2,1,1,1,1,1,1,2,1,1,1,2,1,1,4),
(0.266100373933287,0.969385828517312),(0.0275328340336187,0.114720141806747,
0.149136184348771,0.183552226890795,0.252384311974843,0.26119115197838,
0.269997991981918,0.287611671988993,0.305225351996068,0.322839032003143,
0.340452712010218,0.393293752031443,0.475152331937092,0.516081621889917,
0.536546266866329,0.557010911842741,0.602472788890741,0.647934665938741,
0.738858420034741),.UNSPECIFIED.);
#145=B_SPLINE_SURFACE_WITH_KNOTS('',3,3,((#51312,#51313,#51314,#51315,#51316,
#51317,#51318,#51319,#51320,#51321,#51322,#51323,#51324,#51325,#51326,#51327,
#51328,#51329,#51330,#51331,#51332,#51333,#51334,#51335,#51336,#51337,#51338,
#51339,#51340,#51341,#51342,#51343,#51344,#51345,#51346),(#51347,#51348,
#51349,#51350,#51351,#51352,#51353,#51354,#51355,#51356,#51357,#51358,#51359,
#51360,#51361,#51362,#51363,#51364,#51365,#51366,#51367,#51368,#51369,#51370,
#51371,#51372,#51373,#51374,#51375,#51376,#51377,#51378,#51379,#51380,#51381),
(#51382,#51383,#51384,#51385,#51386,#51387,#51388,#51389,#51390,#51391,
#51392,#51393,#51394,#51395,#51396,#51397,#51398,#51399,#51400,#51401,#51402,
#51403,#51404,#51405,#51406,#51407,#51408,#51409,#51410,#51411,#51412,#51413,
#51414,#51415,#51416),(#51417,#51418,#51419,#51420,#51421,#51422,#51423,
#51424,#51425,#51426,#51427,#51428,#51429,#51430,#51431,#51432,#51433,#51434,
#51435,#51436,#51437,#51438,#51439,#51440,#51441,#51442,#51443,#51444,#51445,
#51446,#51447,#51448,#51449,#51450,#51451),(#51452,#51453,#51454,#51455,
#51456,#51457,#51458,#51459,#51460,#51461,#51462,#51463,#51464,#51465,#51466,
#51467,#51468,#51469,#51470,#51471,#51472,#51473,#51474,#51475,#51476,#51477,
#51478,#51479,#51480,#51481,#51482,#51483,#51484,#51485,#51486)),
 .UNSPECIFIED.,.F.,.F.,.F.,(4,1,4),(4,2,1,1,1,2,1,1,1,1,1,1,1,2,1,2,1,1,
2,1,1,2,1,1,2,4),(0.081890721945263,0.462246010974744,0.969386396347385),
(0.0162979902041911,0.0679082925174644,0.0780945363950841,0.0882807802727037,
0.108653268027943,0.149398243538422,0.154611429799316,0.159824616060209,
0.165037802321103,0.170250988581997,0.191103733625573,0.211956478669149,
0.222382851190937,0.232809223712724,0.281265199287278,0.329721174861832,
0.35931187583389,0.388902576805948,0.448083978750065,0.484049840267495,
0.520015701784926,0.591947424819786,0.634833203943942,0.677718983068097,
0.763490541316409,0.884888589856318),.UNSPECIFIED.);
#146=B_SPLINE_SURFACE_WITH_KNOTS('',3,3,((#51895,#51896,#51897,#51898,#51899,
#51900,#51901,#51902,#51903,#51904,#51905,#51906,#51907,#51908,#51909,#51910,
#51911,#51912,#51913,#51914,#51915,#51916,#51917,#51918,#51919,#51920,#51921,
#51922,#51923,#51924,#51925,#51926,#51927,#51928,#51929,#51930),(#51931,
#51932,#51933,#51934,#51935,#51936,#51937,#51938,#51939,#51940,#51941,#51942,
#51943,#51944,#51945,#51946,#51947,#51948,#51949,#51950,#51951,#51952,#51953,
#51954,#51955,#51956,#51957,#51958,#51959,#51960,#51961,#51962,#51963,#51964,
#51965,#51966),(#51967,#51968,#51969,#51970,#51971,#51972,#51973,#51974,
#51975,#51976,#51977,#51978,#51979,#51980,#51981,#51982,#51983,#51984,#51985,
#51986,#51987,#51988,#51989,#51990,#51991,#51992,#51993,#51994,#51995,#51996,
#51997,#51998,#51999,#52000,#52001,#52002),(#52003,#52004,#52005,#52006,
#52007,#52008,#52009,#52010,#52011,#52012,#52013,#52014,#52015,#52016,#52017,
#52018,#52019,#52020,#52021,#52022,#52023,#52024,#52025,#52026,#52027,#52028,
#52029,#52030,#52031,#52032,#52033,#52034,#52035,#52036,#52037,#52038),
(#52039,#52040,#52041,#52042,#52043,#52044,#52045,#52046,#52047,#52048,
#52049,#52050,#52051,#52052,#52053,#52054,#52055,#52056,#52057,#52058,#52059,
#52060,#52061,#52062,#52063,#52064,#52065,#52066,#52067,#52068,#52069,#52070,
#52071,#52072,#52073,#52074)),.UNSPECIFIED.,.F.,.F.,.F.,(4,1,4),(4,2,1,
1,1,2,1,1,1,1,1,1,1,2,1,2,1,1,2,1,1,1,2,1,1,2,4),(0.081835747691657,0.462214353759979,
0.969385828517743),(0.0162979902041911,0.0679082925174644,0.0780945363950841,
0.0882807802727037,0.108653268027943,0.149398243538422,0.154611429799316,
0.159824616060209,0.165037802321103,0.170250988581997,0.191103733625573,
0.211956478669149,0.222382851190937,0.232809223712724,0.281265199287278,
0.329721174861832,0.35931187583389,0.388902576805948,0.448083978750065,
0.46606690950878,0.484049840267495,0.520015701784926,0.591947424819786,
0.634833203943942,0.677718983068097,0.763490541316409,0.988990749040375),
 .UNSPECIFIED.);
#147=B_SPLINE_SURFACE_WITH_KNOTS('',3,3,((#52134,#52135,#52136,#52137,#52138,
#52139,#52140,#52141,#52142,#52143,#52144,#52145,#52146,#52147,#52148,#52149,
#52150,#52151,#52152,#52153,#52154,#52155,#52156,#52157,#52158,#52159,#52160,
#52161,#52162,#52163,#52164,#52165,#52166,#52167,#52168),(#52169,#52170,
#52171,#52172,#52173,#52174,#52175,#52176,#52177,#52178,#52179,#52180,#52181,
#52182,#52183,#52184,#52185,#52186,#52187,#52188,#52189,#52190,#52191,#52192,
#52193,#52194,#52195,#52196,#52197,#52198,#52199,#52200,#52201,#52202,#52203),
(#52204,#52205,#52206,#52207,#52208,#52209,#52210,#52211,#52212,#52213,
#52214,#52215,#52216,#52217,#52218,#52219,#52220,#52221,#52222,#52223,#52224,
#52225,#52226,#52227,#52228,#52229,#52230,#52231,#52232,#52233,#52234,#52235,
#52236,#52237,#52238),(#52239,#52240,#52241,#52242,#52243,#52244,#52245,
#52246,#52247,#52248,#52249,#52250,#52251,#52252,#52253,#52254,#52255,#52256,
#52257,#52258,#52259,#52260,#52261,#52262,#52263,#52264,#52265,#52266,#52267,
#52268,#52269,#52270,#52271,#52272,#52273),(#52274,#52275,#52276,#52277,
#52278,#52279,#52280,#52281,#52282,#52283,#52284,#52285,#52286,#52287,#52288,
#52289,#52290,#52291,#52292,#52293,#52294,#52295,#52296,#52297,#52298,#52299,
#52300,#52301,#52302,#52303,#52304,#52305,#52306,#52307,#52308)),
 .UNSPECIFIED.,.F.,.F.,.F.,(4,1,4),(4,2,1,1,1,2,1,1,1,1,1,1,1,2,1,2,1,1,
2,1,1,2,1,1,2,4),(0.0818907219452629,0.462246010974744,0.969386396347385),
(0.0162979902041915,0.0679082925174644,0.0780945363950841,0.0882807802727037,
0.108653268027943,0.149398243538422,0.154611429799316,0.159824616060209,
0.165037802321103,0.170250988581997,0.191103733625573,0.211956478669149,
0.222382851190937,0.232809223712724,0.281265199287278,0.329721174861832,
0.35931187583389,0.388902576805948,0.448083978750065,0.484049840267495,
0.520015701784926,0.591947424819786,0.634833203943942,0.677718983068097,
0.763490541316409,0.884888589856318),.UNSPECIFIED.);
#148=B_SPLINE_SURFACE_WITH_KNOTS('',3,3,((#52717,#52718,#52719,#52720,#52721,
#52722,#52723,#52724,#52725,#52726,#52727,#52728,#52729,#52730,#52731,#52732,
#52733,#52734,#52735,#52736,#52737,#52738,#52739,#52740,#52741,#52742,#52743,
#52744,#52745,#52746,#52747,#52748,#52749,#52750,#52751),(#52752,#52753,
#52754,#52755,#52756,#52757,#52758,#52759,#52760,#52761,#52762,#52763,#52764,
#52765,#52766,#52767,#52768,#52769,#52770,#52771,#52772,#52773,#52774,#52775,
#52776,#52777,#52778,#52779,#52780,#52781,#52782,#52783,#52784,#52785,#52786),
(#52787,#52788,#52789,#52790,#52791,#52792,#52793,#52794,#52795,#52796,
#52797,#52798,#52799,#52800,#52801,#52802,#52803,#52804,#52805,#52806,#52807,
#52808,#52809,#52810,#52811,#52812,#52813,#52814,#52815,#52816,#52817,#52818,
#52819,#52820,#52821),(#52822,#52823,#52824,#52825,#52826,#52827,#52828,
#52829,#52830,#52831,#52832,#52833,#52834,#52835,#52836,#52837,#52838,#52839,
#52840,#52841,#52842,#52843,#52844,#52845,#52846,#52847,#52848,#52849,#52850,
#52851,#52852,#52853,#52854,#52855,#52856),(#52857,#52858,#52859,#52860,
#52861,#52862,#52863,#52864,#52865,#52866,#52867,#52868,#52869,#52870,#52871,
#52872,#52873,#52874,#52875,#52876,#52877,#52878,#52879,#52880,#52881,#52882,
#52883,#52884,#52885,#52886,#52887,#52888,#52889,#52890,#52891),(#52892,
#52893,#52894,#52895,#52896,#52897,#52898,#52899,#52900,#52901,#52902,#52903,
#52904,#52905,#52906,#52907,#52908,#52909,#52910,#52911,#52912,#52913,#52914,
#52915,#52916,#52917,#52918,#52919,#52920,#52921,#52922,#52923,#52924,#52925,
#52926)),.UNSPECIFIED.,.F.,.F.,.F.,(4,1,1,4),(4,2,1,1,1,2,1,1,1,1,1,1,2,
1,1,2,1,1,2,1,1,2,1,1,2,4),(0.0818357476916571,0.335421485070539,0.58900722244942,
0.969385828517743),(0.016297990204191,0.0679082925174644,0.0780945363950841,
0.0882807802727037,0.108653268027943,0.149398243538422,0.154611429799316,
0.159824616060209,0.170250988581997,0.180677361103785,0.191103733625573,
0.211956478669149,0.232809223712724,0.281265199287278,0.305493187074555,
0.329721174861832,0.35931187583389,0.388902576805948,0.448083978750065,
0.484049840267495,0.520015701784926,0.591947424819786,0.634833203943942,
0.677718983068097,0.763490541316409,0.988990749040375),.UNSPECIFIED.);
#149=B_SPLINE_SURFACE_WITH_KNOTS('',3,3,((#52986,#52987,#52988,#52989,#52990,
#52991,#52992,#52993,#52994,#52995,#52996,#52997,#52998,#52999,#53000,#53001,
#53002,#53003,#53004,#53005,#53006,#53007,#53008,#53009,#53010,#53011,#53012,
#53013,#53014,#53015,#53016,#53017,#53018,#53019,#53020,#53021),(#53022,
#53023,#53024,#53025,#53026,#53027,#53028,#53029,#53030,#53031,#53032,#53033,
#53034,#53035,#53036,#53037,#53038,#53039,#53040,#53041,#53042,#53043,#53044,
#53045,#53046,#53047,#53048,#53049,#53050,#53051,#53052,#53053,#53054,#53055,
#53056,#53057),(#53058,#53059,#53060,#53061,#53062,#53063,#53064,#53065,
#53066,#53067,#53068,#53069,#53070,#53071,#53072,#53073,#53074,#53075,#53076,
#53077,#53078,#53079,#53080,#53081,#53082,#53083,#53084,#53085,#53086,#53087,
#53088,#53089,#53090,#53091,#53092,#53093),(#53094,#53095,#53096,#53097,
#53098,#53099,#53100,#53101,#53102,#53103,#53104,#53105,#53106,#53107,#53108,
#53109,#53110,#53111,#53112,#53113,#53114,#53115,#53116,#53117,#53118,#53119,
#53120,#53121,#53122,#53123,#53124,#53125,#53126,#53127,#53128,#53129),
(#53130,#53131,#53132,#53133,#53134,#53135,#53136,#53137,#53138,#53139,
#53140,#53141,#53142,#53143,#53144,#53145,#53146,#53147,#53148,#53149,#53150,
#53151,#53152,#53153,#53154,#53155,#53156,#53157,#53158,#53159,#53160,#53161,
#53162,#53163,#53164,#53165)),.UNSPECIFIED.,.F.,.F.,.F.,(4,1,4),(4,2,1,
1,1,2,1,1,1,1,1,1,1,2,1,2,1,1,2,1,1,1,2,1,1,2,4),(0.0818907219452629,0.462246010974744,
0.969386396347385),(0.0162979902041916,0.0679082925174644,0.0780945363950841,
0.0882807802727037,0.108653268027943,0.149398243538422,0.154611429799316,
0.159824616060209,0.165037802321103,0.170250988581997,0.191103733625573,
0.211956478669149,0.222382851190937,0.232809223712724,0.281265199287278,
0.329721174861832,0.35931187583389,0.388902576805948,0.448083978750065,
0.46606690950878,0.484049840267495,0.520015701784926,0.591947424819786,
0.634833203943942,0.677718983068097,0.763490541316409,0.884888589856318),
 .UNSPECIFIED.);
#150=B_SPLINE_SURFACE_WITH_KNOTS('',3,3,((#53574,#53575,#53576,#53577,#53578,
#53579,#53580,#53581,#53582,#53583,#53584,#53585,#53586,#53587,#53588,#53589,
#53590,#53591,#53592,#53593,#53594,#53595,#53596,#53597,#53598,#53599,#53600,
#53601,#53602,#53603,#53604,#53605,#53606,#53607,#53608),(#53609,#53610,
#53611,#53612,#53613,#53614,#53615,#53616,#53617,#53618,#53619,#53620,#53621,
#53622,#53623,#53624,#53625,#53626,#53627,#53628,#53629,#53630,#53631,#53632,
#53633,#53634,#53635,#53636,#53637,#53638,#53639,#53640,#53641,#53642,#53643),
(#53644,#53645,#53646,#53647,#53648,#53649,#53650,#53651,#53652,#53653,
#53654,#53655,#53656,#53657,#53658,#53659,#53660,#53661,#53662,#53663,#53664,
#53665,#53666,#53667,#53668,#53669,#53670,#53671,#53672,#53673,#53674,#53675,
#53676,#53677,#53678),(#53679,#53680,#53681,#53682,#53683,#53684,#53685,
#53686,#53687,#53688,#53689,#53690,#53691,#53692,#53693,#53694,#53695,#53696,
#53697,#53698,#53699,#53700,#53701,#53702,#53703,#53704,#53705,#53706,#53707,
#53708,#53709,#53710,#53711,#53712,#53713),(#53714,#53715,#53716,#53717,
#53718,#53719,#53720,#53721,#53722,#53723,#53724,#53725,#53726,#53727,#53728,
#53729,#53730,#53731,#53732,#53733,#53734,#53735,#53736,#53737,#53738,#53739,
#53740,#53741,#53742,#53743,#53744,#53745,#53746,#53747,#53748)),
 .UNSPECIFIED.,.F.,.F.,.F.,(4,1,4),(4,2,1,1,1,2,1,1,1,1,1,1,1,2,1,2,1,1,
2,1,1,2,1,1,2,4),(0.0818357476916571,0.462214353759979,0.969385828517743),
(0.0162979902041911,0.0679082925174644,0.0780945363950841,0.0882807802727037,
0.108653268027943,0.149398243538422,0.154611429799316,0.159824616060209,
0.165037802321103,0.170250988581997,0.191103733625573,0.211956478669149,
0.222382851190937,0.232809223712724,0.281265199287278,0.329721174861832,
0.35931187583389,0.388902576805948,0.448083978750065,0.484049840267495,
0.520015701784926,0.591947424819786,0.634833203943942,0.677718983068097,
0.763490541316409,0.988990749040375),.UNSPECIFIED.);
#151=B_SPLINE_SURFACE_WITH_KNOTS('',3,3,((#53808,#53809,#53810,#53811,#53812,
#53813,#53814,#53815,#53816,#53817,#53818,#53819,#53820,#53821,#53822,#53823,
#53824,#53825,#53826,#53827,#53828,#53829,#53830,#53831,#53832,#53833,#53834,
#53835,#53836,#53837,#53838,#53839,#53840,#53841,#53842),(#53843,#53844,
#53845,#53846,#53847,#53848,#53849,#53850,#53851,#53852,#53853,#53854,#53855,
#53856,#53857,#53858,#53859,#53860,#53861,#53862,#53863,#53864,#53865,#53866,
#53867,#53868,#53869,#53870,#53871,#53872,#53873,#53874,#53875,#53876,#53877),
(#53878,#53879,#53880,#53881,#53882,#53883,#53884,#53885,#53886,#53887,
#53888,#53889,#53890,#53891,#53892,#53893,#53894,#53895,#53896,#53897,#53898,
#53899,#53900,#53901,#53902,#53903,#53904,#53905,#53906,#53907,#53908,#53909,
#53910,#53911,#53912),(#53913,#53914,#53915,#53916,#53917,#53918,#53919,
#53920,#53921,#53922,#53923,#53924,#53925,#53926,#53927,#53928,#53929,#53930,
#53931,#53932,#53933,#53934,#53935,#53936,#53937,#53938,#53939,#53940,#53941,
#53942,#53943,#53944,#53945,#53946,#53947),(#53948,#53949,#53950,#53951,
#53952,#53953,#53954,#53955,#53956,#53957,#53958,#53959,#53960,#53961,#53962,
#53963,#53964,#53965,#53966,#53967,#53968,#53969,#53970,#53971,#53972,#53973,
#53974,#53975,#53976,#53977,#53978,#53979,#53980,#53981,#53982)),
 .UNSPECIFIED.,.F.,.F.,.F.,(4,1,4),(4,2,1,1,1,2,1,1,1,1,1,1,1,2,1,2,1,1,
2,1,1,2,1,1,2,4),(0.0818907219452629,0.462246010974744,0.969386396347385),
(0.0162979902041915,0.0679082925174644,0.0780945363950841,0.0882807802727037,
0.108653268027943,0.149398243538422,0.154611429799316,0.159824616060209,
0.165037802321103,0.170250988581997,0.191103733625573,0.211956478669149,
0.222382851190937,0.232809223712724,0.281265199287278,0.329721174861832,
0.35931187583389,0.388902576805948,0.448083978750065,0.484049840267495,
0.520015701784926,0.591947424819786,0.634833203943942,0.677718983068097,
0.763490541316409,0.884888589856318),.UNSPECIFIED.);
#152=B_SPLINE_SURFACE_WITH_KNOTS('',3,3,((#54391,#54392,#54393,#54394,#54395,
#54396,#54397,#54398,#54399,#54400,#54401,#54402,#54403,#54404,#54405,#54406,
#54407,#54408,#54409,#54410,#54411,#54412,#54413,#54414,#54415,#54416,#54417,
#54418,#54419,#54420,#54421,#54422,#54423,#54424,#54425),(#54426,#54427,
#54428,#54429,#54430,#54431,#54432,#54433,#54434,#54435,#54436,#54437,#54438,
#54439,#54440,#54441,#54442,#54443,#54444,#54445,#54446,#54447,#54448,#54449,
#54450,#54451,#54452,#54453,#54454,#54455,#54456,#54457,#54458,#54459,#54460),
(#54461,#54462,#54463,#54464,#54465,#54466,#54467,#54468,#54469,#54470,
#54471,#54472,#54473,#54474,#54475,#54476,#54477,#54478,#54479,#54480,#54481,
#54482,#54483,#54484,#54485,#54486,#54487,#54488,#54489,#54490,#54491,#54492,
#54493,#54494,#54495),(#54496,#54497,#54498,#54499,#54500,#54501,#54502,
#54503,#54504,#54505,#54506,#54507,#54508,#54509,#54510,#54511,#54512,#54513,
#54514,#54515,#54516,#54517,#54518,#54519,#54520,#54521,#54522,#54523,#54524,
#54525,#54526,#54527,#54528,#54529,#54530),(#54531,#54532,#54533,#54534,
#54535,#54536,#54537,#54538,#54539,#54540,#54541,#54542,#54543,#54544,#54545,
#54546,#54547,#54548,#54549,#54550,#54551,#54552,#54553,#54554,#54555,#54556,
#54557,#54558,#54559,#54560,#54561,#54562,#54563,#54564,#54565),(#54566,
#54567,#54568,#54569,#54570,#54571,#54572,#54573,#54574,#54575,#54576,#54577,
#54578,#54579,#54580,#54581,#54582,#54583,#54584,#54585,#54586,#54587,#54588,
#54589,#54590,#54591,#54592,#54593,#54594,#54595,#54596,#54597,#54598,#54599,
#54600)),.UNSPECIFIED.,.F.,.F.,.F.,(4,1,1,4),(4,2,1,1,1,2,1,1,1,1,1,1,2,
1,1,2,1,1,2,1,1,2,1,1,2,4),(0.0818357476916571,0.335421485070539,0.58900722244942,
0.969385828517743),(0.0162979902041912,0.0679082925174644,0.0780945363950841,
0.0882807802727037,0.108653268027943,0.149398243538422,0.154611429799316,
0.159824616060209,0.170250988581997,0.180677361103785,0.191103733625573,
0.211956478669149,0.232809223712724,0.281265199287278,0.305493187074555,
0.329721174861832,0.35931187583389,0.388902576805948,0.448083978750065,
0.484049840267495,0.520015701784926,0.591947424819786,0.634833203943942,
0.677718983068097,0.763490541316409,0.988990749040375),.UNSPECIFIED.);
#153=B_SPLINE_SURFACE_WITH_KNOTS('',3,3,((#54660,#54661,#54662,#54663,#54664,
#54665,#54666,#54667,#54668,#54669,#54670,#54671,#54672,#54673,#54674,#54675,
#54676,#54677,#54678,#54679,#54680,#54681,#54682,#54683,#54684,#54685,#54686,
#54687,#54688,#54689,#54690,#54691,#54692,#54693,#54694),(#54695,#54696,
#54697,#54698,#54699,#54700,#54701,#54702,#54703,#54704,#54705,#54706,#54707,
#54708,#54709,#54710,#54711,#54712,#54713,#54714,#54715,#54716,#54717,#54718,
#54719,#54720,#54721,#54722,#54723,#54724,#54725,#54726,#54727,#54728,#54729),
(#54730,#54731,#54732,#54733,#54734,#54735,#54736,#54737,#54738,#54739,
#54740,#54741,#54742,#54743,#54744,#54745,#54746,#54747,#54748,#54749,#54750,
#54751,#54752,#54753,#54754,#54755,#54756,#54757,#54758,#54759,#54760,#54761,
#54762,#54763,#54764),(#54765,#54766,#54767,#54768,#54769,#54770,#54771,
#54772,#54773,#54774,#54775,#54776,#54777,#54778,#54779,#54780,#54781,#54782,
#54783,#54784,#54785,#54786,#54787,#54788,#54789,#54790,#54791,#54792,#54793,
#54794,#54795,#54796,#54797,#54798,#54799),(#54800,#54801,#54802,#54803,
#54804,#54805,#54806,#54807,#54808,#54809,#54810,#54811,#54812,#54813,#54814,
#54815,#54816,#54817,#54818,#54819,#54820,#54821,#54822,#54823,#54824,#54825,
#54826,#54827,#54828,#54829,#54830,#54831,#54832,#54833,#54834)),
 .UNSPECIFIED.,.F.,.F.,.F.,(4,1,4),(4,2,1,1,1,2,1,1,1,1,1,1,1,2,1,2,1,1,
2,1,1,2,1,1,2,4),(0.0818907219452629,0.462246010974744,0.969386396347385),
(0.0162979902041915,0.0679082925174644,0.0780945363950841,0.0882807802727037,
0.108653268027943,0.149398243538422,0.154611429799316,0.159824616060209,
0.165037802321103,0.170250988581997,0.191103733625573,0.211956478669149,
0.222382851190937,0.232809223712724,0.281265199287278,0.329721174861832,
0.35931187583389,0.388902576805948,0.448083978750065,0.484049840267495,
0.520015701784926,0.591947424819786,0.634833203943942,0.677718983068097,
0.763490541316409,0.884888589856319),.UNSPECIFIED.);
#154=B_SPLINE_SURFACE_WITH_KNOTS('',3,3,((#55243,#55244,#55245,#55246,#55247,
#55248,#55249,#55250,#55251,#55252,#55253,#55254,#55255,#55256,#55257,#55258,
#55259,#55260,#55261,#55262,#55263,#55264,#55265,#55266,#55267,#55268,#55269,
#55270,#55271,#55272,#55273,#55274,#55275,#55276,#55277),(#55278,#55279,
#55280,#55281,#55282,#55283,#55284,#55285,#55286,#55287,#55288,#55289,#55290,
#55291,#55292,#55293,#55294,#55295,#55296,#55297,#55298,#55299,#55300,#55301,
#55302,#55303,#55304,#55305,#55306,#55307,#55308,#55309,#55310,#55311,#55312),
(#55313,#55314,#55315,#55316,#55317,#55318,#55319,#55320,#55321,#55322,
#55323,#55324,#55325,#55326,#55327,#55328,#55329,#55330,#55331,#55332,#55333,
#55334,#55335,#55336,#55337,#55338,#55339,#55340,#55341,#55342,#55343,#55344,
#55345,#55346,#55347),(#55348,#55349,#55350,#55351,#55352,#55353,#55354,
#55355,#55356,#55357,#55358,#55359,#55360,#55361,#55362,#55363,#55364,#55365,
#55366,#55367,#55368,#55369,#55370,#55371,#55372,#55373,#55374,#55375,#55376,
#55377,#55378,#55379,#55380,#55381,#55382),(#55383,#55384,#55385,#55386,
#55387,#55388,#55389,#55390,#55391,#55392,#55393,#55394,#55395,#55396,#55397,
#55398,#55399,#55400,#55401,#55402,#55403,#55404,#55405,#55406,#55407,#55408,
#55409,#55410,#55411,#55412,#55413,#55414,#55415,#55416,#55417)),
 .UNSPECIFIED.,.F.,.F.,.F.,(4,1,4),(4,2,1,1,1,2,1,1,1,1,1,1,1,2,1,2,1,1,
2,1,1,2,1,1,2,4),(0.081835747691657,0.462214353759979,0.969385828517743),
(0.0162979902041914,0.0679082925174644,0.0780945363950841,0.0882807802727037,
0.108653268027943,0.149398243538422,0.154611429799316,0.159824616060209,
0.165037802321103,0.170250988581997,0.191103733625573,0.211956478669149,
0.222382851190937,0.232809223712724,0.281265199287278,0.329721174861832,
0.35931187583389,0.388902576805948,0.448083978750065,0.484049840267495,
0.520015701784926,0.591947424819786,0.634833203943942,0.677718983068097,
0.763490541316409,0.988990749040375),.UNSPECIFIED.);
#155=B_SPLINE_SURFACE_WITH_KNOTS('',3,3,((#55477,#55478,#55479,#55480,#55481,
#55482,#55483,#55484,#55485,#55486,#55487,#55488,#55489,#55490,#55491,#55492,
#55493,#55494,#55495,#55496,#55497,#55498,#55499,#55500,#55501,#55502,#55503,
#55504,#55505,#55506,#55507,#55508,#55509,#55510,#55511),(#55512,#55513,
#55514,#55515,#55516,#55517,#55518,#55519,#55520,#55521,#55522,#55523,#55524,
#55525,#55526,#55527,#55528,#55529,#55530,#55531,#55532,#55533,#55534,#55535,
#55536,#55537,#55538,#55539,#55540,#55541,#55542,#55543,#55544,#55545,#55546),
(#55547,#55548,#55549,#55550,#55551,#55552,#55553,#55554,#55555,#55556,
#55557,#55558,#55559,#55560,#55561,#55562,#55563,#55564,#55565,#55566,#55567,
#55568,#55569,#55570,#55571,#55572,#55573,#55574,#55575,#55576,#55577,#55578,
#55579,#55580,#55581),(#55582,#55583,#55584,#55585,#55586,#55587,#55588,
#55589,#55590,#55591,#55592,#55593,#55594,#55595,#55596,#55597,#55598,#55599,
#55600,#55601,#55602,#55603,#55604,#55605,#55606,#55607,#55608,#55609,#55610,
#55611,#55612,#55613,#55614,#55615,#55616),(#55617,#55618,#55619,#55620,
#55621,#55622,#55623,#55624,#55625,#55626,#55627,#55628,#55629,#55630,#55631,
#55632,#55633,#55634,#55635,#55636,#55637,#55638,#55639,#55640,#55641,#55642,
#55643,#55644,#55645,#55646,#55647,#55648,#55649,#55650,#55651)),
 .UNSPECIFIED.,.F.,.F.,.F.,(4,1,4),(4,2,1,1,1,2,1,1,1,1,1,1,1,2,1,2,1,1,
2,1,1,2,1,1,2,4),(0.0818907219452629,0.462246010974744,0.969386396347385),
(0.0162979902041911,0.0679082925174644,0.0780945363950841,0.0882807802727037,
0.108653268027943,0.149398243538422,0.154611429799316,0.159824616060209,
0.165037802321103,0.170250988581997,0.191103733625573,0.211956478669149,
0.222382851190937,0.232809223712724,0.281265199287278,0.329721174861832,
0.35931187583389,0.388902576805948,0.448083978750065,0.484049840267495,
0.520015701784926,0.591947424819786,0.634833203943942,0.677718983068097,
0.763490541316409,0.884888589856318),.UNSPECIFIED.);
#156=B_SPLINE_SURFACE_WITH_KNOTS('',3,3,((#56065,#56066,#56067,#56068,#56069,
#56070,#56071,#56072,#56073,#56074,#56075,#56076,#56077,#56078,#56079,#56080,
#56081,#56082,#56083,#56084,#56085,#56086,#56087,#56088,#56089,#56090,#56091,
#56092,#56093,#56094,#56095,#56096,#56097,#56098,#56099,#56100),(#56101,
#56102,#56103,#56104,#56105,#56106,#56107,#56108,#56109,#56110,#56111,#56112,
#56113,#56114,#56115,#56116,#56117,#56118,#56119,#56120,#56121,#56122,#56123,
#56124,#56125,#56126,#56127,#56128,#56129,#56130,#56131,#56132,#56133,#56134,
#56135,#56136),(#56137,#56138,#56139,#56140,#56141,#56142,#56143,#56144,
#56145,#56146,#56147,#56148,#56149,#56150,#56151,#56152,#56153,#56154,#56155,
#56156,#56157,#56158,#56159,#56160,#56161,#56162,#56163,#56164,#56165,#56166,
#56167,#56168,#56169,#56170,#56171,#56172),(#56173,#56174,#56175,#56176,
#56177,#56178,#56179,#56180,#56181,#56182,#56183,#56184,#56185,#56186,#56187,
#56188,#56189,#56190,#56191,#56192,#56193,#56194,#56195,#56196,#56197,#56198,
#56199,#56200,#56201,#56202,#56203,#56204,#56205,#56206,#56207,#56208),
(#56209,#56210,#56211,#56212,#56213,#56214,#56215,#56216,#56217,#56218,
#56219,#56220,#56221,#56222,#56223,#56224,#56225,#56226,#56227,#56228,#56229,
#56230,#56231,#56232,#56233,#56234,#56235,#56236,#56237,#56238,#56239,#56240,
#56241,#56242,#56243,#56244)),.UNSPECIFIED.,.F.,.F.,.F.,(4,1,4),(4,2,1,
1,2,1,1,1,1,1,1,1,2,1,1,2,1,1,2,1,1,2,1,1,1,2,4),(0.0818357476933141,0.462214353760926,
0.969385828517743),(0.0162979902041911,0.0679082925174644,0.0882807802727037,
0.108653268027943,0.149398243538422,0.154611429799316,0.159824616060209,
0.165037802321103,0.170250988581997,0.191103733625573,0.211956478669149,
0.222382851190937,0.232809223712724,0.281265199287278,0.305493187074555,
0.329721174861832,0.35931187583389,0.388902576805948,0.448083978750065,
0.484049840267495,0.520015701784926,0.591947424819786,0.613390314381864,
0.634833203943942,0.677718983068097,0.763490541316409,0.988990749040375),
 .UNSPECIFIED.);
#157=B_SPLINE_SURFACE_WITH_KNOTS('',3,3,((#56626,#56627,#56628,#56629,#56630,
#56631,#56632,#56633,#56634,#56635,#56636,#56637,#56638,#56639,#56640,#56641,
#56642,#56643,#56644,#56645,#56646,#56647,#56648,#56649,#56650,#56651,#56652,
#56653,#56654,#56655,#56656,#56657,#56658,#56659,#56660),(#56661,#56662,
#56663,#56664,#56665,#56666,#56667,#56668,#56669,#56670,#56671,#56672,#56673,
#56674,#56675,#56676,#56677,#56678,#56679,#56680,#56681,#56682,#56683,#56684,
#56685,#56686,#56687,#56688,#56689,#56690,#56691,#56692,#56693,#56694,#56695),
(#56696,#56697,#56698,#56699,#56700,#56701,#56702,#56703,#56704,#56705,
#56706,#56707,#56708,#56709,#56710,#56711,#56712,#56713,#56714,#56715,#56716,
#56717,#56718,#56719,#56720,#56721,#56722,#56723,#56724,#56725,#56726,#56727,
#56728,#56729,#56730),(#56731,#56732,#56733,#56734,#56735,#56736,#56737,
#56738,#56739,#56740,#56741,#56742,#56743,#56744,#56745,#56746,#56747,#56748,
#56749,#56750,#56751,#56752,#56753,#56754,#56755,#56756,#56757,#56758,#56759,
#56760,#56761,#56762,#56763,#56764,#56765),(#56766,#56767,#56768,#56769,
#56770,#56771,#56772,#56773,#56774,#56775,#56776,#56777,#56778,#56779,#56780,
#56781,#56782,#56783,#56784,#56785,#56786,#56787,#56788,#56789,#56790,#56791,
#56792,#56793,#56794,#56795,#56796,#56797,#56798,#56799,#56800)),
 .UNSPECIFIED.,.F.,.F.,.F.,(4,1,4),(4,2,1,1,1,2,1,1,1,1,1,1,1,2,1,2,1,1,
2,1,1,2,1,1,2,4),(0.081890721945263,0.462246010974744,0.969386396347385),
(0.0162979902041911,0.0679082925174644,0.0780945363950841,0.0882807802727037,
0.108653268027943,0.149398243538422,0.154611429799316,0.159824616060209,
0.165037802321103,0.170250988581997,0.191103733625573,0.211956478669149,
0.222382851190937,0.232809223712724,0.281265199287278,0.329721174861832,
0.35931187583389,0.388902576805948,0.448083978750065,0.484049840267495,
0.520015701784926,0.591947424819786,0.634833203943942,0.677718983068097,
0.763490541316409,0.884888589856318),.UNSPECIFIED.);
#158=B_SPLINE_SURFACE_WITH_KNOTS('',3,3,((#57155,#57156,#57157,#57158,#57159,
#57160,#57161,#57162,#57163,#57164,#57165,#57166,#57167,#57168,#57169,#57170,
#57171,#57172,#57173,#57174,#57175,#57176,#57177,#57178,#57179,#57180,#57181,
#57182,#57183,#57184,#57185,#57186,#57187,#57188,#57189),(#57190,#57191,
#57192,#57193,#57194,#57195,#57196,#57197,#57198,#57199,#57200,#57201,#57202,
#57203,#57204,#57205,#57206,#57207,#57208,#57209,#57210,#57211,#57212,#57213,
#57214,#57215,#57216,#57217,#57218,#57219,#57220,#57221,#57222,#57223,#57224),
(#57225,#57226,#57227,#57228,#57229,#57230,#57231,#57232,#57233,#57234,
#57235,#57236,#57237,#57238,#57239,#57240,#57241,#57242,#57243,#57244,#57245,
#57246,#57247,#57248,#57249,#57250,#57251,#57252,#57253,#57254,#57255,#57256,
#57257,#57258,#57259),(#57260,#57261,#57262,#57263,#57264,#57265,#57266,
#57267,#57268,#57269,#57270,#57271,#57272,#57273,#57274,#57275,#57276,#57277,
#57278,#57279,#57280,#57281,#57282,#57283,#57284,#57285,#57286,#57287,#57288,
#57289,#57290,#57291,#57292,#57293,#57294),(#57295,#57296,#57297,#57298,
#57299,#57300,#57301,#57302,#57303,#57304,#57305,#57306,#57307,#57308,#57309,
#57310,#57311,#57312,#57313,#57314,#57315,#57316,#57317,#57318,#57319,#57320,
#57321,#57322,#57323,#57324,#57325,#57326,#57327,#57328,#57329),(#57330,
#57331,#57332,#57333,#57334,#57335,#57336,#57337,#57338,#57339,#57340,#57341,
#57342,#57343,#57344,#57345,#57346,#57347,#57348,#57349,#57350,#57351,#57352,
#57353,#57354,#57355,#57356,#57357,#57358,#57359,#57360,#57361,#57362,#57363,
#57364)),.UNSPECIFIED.,.F.,.F.,.F.,(4,1,1,4),(4,2,1,1,1,2,1,1,1,1,1,1,2,
1,1,2,1,1,2,1,1,2,1,1,2,4),(0.0818357476916571,0.335421485070539,0.58900722244942,
0.969385828517743),(0.0162979902041911,0.0679082925174644,0.0780945363950841,
0.0882807802727037,0.108653268027943,0.149398243538422,0.154611429799316,
0.159824616060209,0.170250988581997,0.180677361103785,0.191103733625573,
0.211956478669149,0.232809223712724,0.281265199287278,0.305493187074555,
0.329721174861832,0.35931187583389,0.388902576805948,0.448083978750065,
0.484049840267495,0.520015701784926,0.591947424819786,0.634833203943942,
0.677718983068097,0.763490541316409,0.988990749040375),.UNSPECIFIED.);
#159=B_SPLINE_SURFACE_WITH_KNOTS('',3,3,((#57414,#57415,#57416,#57417),
(#57418,#57419,#57420,#57421),(#57422,#57423,#57424,#57425),(#57426,#57427,
#57428,#57429)),.UNSPECIFIED.,.F.,.F.,.F.,(4,4),(4,4),(0.,1.),(0.0769218004431789,
0.23169515901548),.UNSPECIFIED.);
#160=B_SPLINE_SURFACE_WITH_KNOTS('',3,3,((#57480,#57481,#57482,#57483),
(#57484,#57485,#57486,#57487),(#57488,#57489,#57490,#57491),(#57492,#57493,
#57494,#57495)),.UNSPECIFIED.,.F.,.F.,.F.,(4,4),(4,4),(0.,1.),(0.0769218004431759,
0.23169515901548),.UNSPECIFIED.);
#161=B_SPLINE_SURFACE_WITH_KNOTS('',3,3,((#57546,#57547,#57548,#57549),
(#57550,#57551,#57552,#57553),(#57554,#57555,#57556,#57557),(#57558,#57559,
#57560,#57561)),.UNSPECIFIED.,.F.,.F.,.F.,(4,4),(4,4),(0.,1.),(0.0769218004431517,
0.231695159015479),.UNSPECIFIED.);
#162=B_SPLINE_SURFACE_WITH_KNOTS('',3,3,((#57698,#57699,#57700,#57701),
(#57702,#57703,#57704,#57705),(#57706,#57707,#57708,#57709),(#57710,#57711,
#57712,#57713)),.UNSPECIFIED.,.F.,.F.,.F.,(4,4),(4,4),(0.,1.),(0.0769218004431787,
0.23169515901548),.UNSPECIFIED.);
#163=B_SPLINE_SURFACE_WITH_KNOTS('',3,3,((#57733,#57734,#57735,#57736),
(#57737,#57738,#57739,#57740),(#57741,#57742,#57743,#57744),(#57745,#57746,
#57747,#57748)),.UNSPECIFIED.,.F.,.F.,.F.,(4,4),(4,4),(0.,1.),(0.126990834822138,
0.281764193765889),.UNSPECIFIED.);
#164=B_SPLINE_SURFACE_WITH_KNOTS('',3,3,((#57798,#57799,#57800,#57801),
(#57802,#57803,#57804,#57805),(#57806,#57807,#57808,#57809),(#57810,#57811,
#57812,#57813)),.UNSPECIFIED.,.F.,.F.,.F.,(4,4),(4,4),(0.,1.),(0.0769218004431756,
0.231695159015479),.UNSPECIFIED.);
#165=B_SPLINE_SURFACE_WITH_KNOTS('',3,3,((#57828,#57829,#57830,#57831),
(#57832,#57833,#57834,#57835),(#57836,#57837,#57838,#57839),(#57840,#57841,
#57842,#57843)),.UNSPECIFIED.,.F.,.F.,.F.,(4,4),(4,4),(0.,1.),(0.126990834822142,
0.281764193765892),.UNSPECIFIED.);
#166=B_SPLINE_SURFACE_WITH_KNOTS('',3,3,((#57893,#57894,#57895,#57896),
(#57897,#57898,#57899,#57900),(#57901,#57902,#57903,#57904),(#57905,#57906,
#57907,#57908)),.UNSPECIFIED.,.F.,.F.,.F.,(4,4),(4,4),(0.,1.),(0.076921800443152,
0.231695159015479),.UNSPECIFIED.);
#167=B_SPLINE_SURFACE_WITH_KNOTS('',3,3,((#57954,#57955,#57956,#57957),
(#57958,#57959,#57960,#57961),(#57962,#57963,#57964,#57965),(#57966,#57967,
#57968,#57969)),.UNSPECIFIED.,.F.,.F.,.F.,(4,4),(4,4),(0.,1.),(0.0769218008186939,
0.221927025906161),.UNSPECIFIED.);
#168=B_SPLINE_SURFACE_WITH_KNOTS('',3,3,((#57980,#57981,#57982,#57983),
(#57984,#57985,#57986,#57987),(#57988,#57989,#57990,#57991),(#57992,#57993,
#57994,#57995)),.UNSPECIFIED.,.F.,.F.,.F.,(4,4),(4,4),(0.,1.),(0.12699083482214,
0.281764193752995),.UNSPECIFIED.);
#169=B_SPLINE_SURFACE_WITH_KNOTS('',3,3,((#58040,#58041,#58042,#58043),
(#58044,#58045,#58046,#58047),(#58048,#58049,#58050,#58051),(#58052,#58053,
#58054,#58055)),.UNSPECIFIED.,.F.,.F.,.F.,(4,4),(4,4),(0.,1.),(0.0769218004431788,
0.23169515901548),.UNSPECIFIED.);
#170=B_SPLINE_SURFACE_WITH_KNOTS('',3,3,((#58070,#58071,#58072,#58073),
(#58074,#58075,#58076,#58077),(#58078,#58079,#58080,#58081),(#58082,#58083,
#58084,#58085)),.UNSPECIFIED.,.F.,.F.,.F.,(4,4),(4,4),(0.,1.),(0.126990834822138,
0.281764193765889),.UNSPECIFIED.);
#171=B_SPLINE_SURFACE_WITH_KNOTS('',3,3,((#58135,#58136,#58137,#58138),
(#58139,#58140,#58141,#58142),(#58143,#58144,#58145,#58146),(#58147,#58148,
#58149,#58150)),.UNSPECIFIED.,.F.,.F.,.F.,(4,4),(4,4),(0.,1.),(0.0769218004431755,
0.231695159015479),.UNSPECIFIED.);
#172=B_SPLINE_SURFACE_WITH_KNOTS('',3,3,((#58165,#58166,#58167,#58168),
(#58169,#58170,#58171,#58172),(#58173,#58174,#58175,#58176),(#58177,#58178,
#58179,#58180)),.UNSPECIFIED.,.F.,.F.,.F.,(4,4),(4,4),(0.,1.),(0.126990834822142,
0.281764193765893),.UNSPECIFIED.);
#173=B_SPLINE_SURFACE_WITH_KNOTS('',3,3,((#58230,#58231,#58232,#58233),
(#58234,#58235,#58236,#58237),(#58238,#58239,#58240,#58241),(#58242,#58243,
#58244,#58245)),.UNSPECIFIED.,.F.,.F.,.F.,(4,4),(4,4),(0.,1.),(0.0769218004431519,
0.23169515901548),.UNSPECIFIED.);
#174=B_SPLINE_SURFACE_WITH_KNOTS('',3,3,((#58260,#58261,#58262,#58263),
(#58264,#58265,#58266,#58267),(#58268,#58269,#58270,#58271),(#58272,#58273,
#58274,#58275)),.UNSPECIFIED.,.F.,.F.,.F.,(4,4),(4,4),(0.,1.),(0.126990834822139,
0.28176419376589),.UNSPECIFIED.);
#175=B_SPLINE_SURFACE_WITH_KNOTS('',3,3,((#58289,#58290,#58291,#58292),
(#58293,#58294,#58295,#58296),(#58297,#58298,#58299,#58300),(#58301,#58302,
#58303,#58304)),.UNSPECIFIED.,.F.,.F.,.F.,(4,4),(4,4),(0.380102179090416,
1.),(0.231695159015479,0.246948509226624),.UNSPECIFIED.);
#176=B_SPLINE_SURFACE_WITH_KNOTS('',3,3,((#58322,#58323,#58324,#58325),
(#58326,#58327,#58328,#58329),(#58330,#58331,#58332,#58333),(#58334,#58335,
#58336,#58337)),.UNSPECIFIED.,.F.,.F.,.F.,(4,4),(4,4),(0.380102179090417,
1.),(0.231695159015479,0.246948509226624),.UNSPECIFIED.);
#177=B_SPLINE_SURFACE_WITH_KNOTS('',3,3,((#58355,#58356,#58357,#58358),
(#58359,#58360,#58361,#58362),(#58363,#58364,#58365,#58366),(#58367,#58368,
#58369,#58370)),.UNSPECIFIED.,.F.,.F.,.F.,(4,4),(4,4),(0.380102179090425,
1.),(0.23169515901548,0.246948509226623),.UNSPECIFIED.);
#178=B_SPLINE_SURFACE_WITH_KNOTS('',3,3,((#58388,#58389,#58390,#58391),
(#58392,#58393,#58394,#58395),(#58396,#58397,#58398,#58399),(#58400,#58401,
#58402,#58403)),.UNSPECIFIED.,.F.,.F.,.F.,(4,4),(4,4),(0.380102179090409,
1.),(0.23169515901548,0.246948509226625),.UNSPECIFIED.);
#179=B_SPLINE_SURFACE_WITH_KNOTS('',3,3,((#58421,#58422,#58423,#58424),
(#58425,#58426,#58427,#58428),(#58429,#58430,#58431,#58432),(#58433,#58434,
#58435,#58436)),.UNSPECIFIED.,.F.,.F.,.F.,(4,4),(4,4),(0.380102179090415,
1.),(0.231695159015479,0.246948509226624),.UNSPECIFIED.);
#180=B_SPLINE_SURFACE_WITH_KNOTS('',3,3,((#58454,#58455,#58456,#58457),
(#58458,#58459,#58460,#58461),(#58462,#58463,#58464,#58465),(#58466,#58467,
#58468,#58469)),.UNSPECIFIED.,.F.,.F.,.F.,(4,4),(4,4),(0.380102179090434,
1.),(0.23169515901548,0.246948509226623),.UNSPECIFIED.);
#181=B_SPLINE_SURFACE_WITH_KNOTS('',3,3,((#58487,#58488,#58489,#58490),
(#58491,#58492,#58493,#58494),(#58495,#58496,#58497,#58498),(#58499,#58500,
#58501,#58502)),.UNSPECIFIED.,.F.,.F.,.F.,(4,4),(4,4),(0.,1.),(0.12699083482214,
0.281764193765889),.UNSPECIFIED.);
#182=B_SPLINE_SURFACE_WITH_KNOTS('',3,3,((#58516,#58517,#58518,#58519),
(#58520,#58521,#58522,#58523),(#58524,#58525,#58526,#58527),(#58528,#58529,
#58530,#58531)),.UNSPECIFIED.,.F.,.F.,.F.,(4,4),(4,4),(0.380102179091578,
1.),(0.23169515901548,0.246948509226623),.UNSPECIFIED.);
#183=B_SPLINE_SURFACE_WITH_KNOTS('',3,3,((#58549,#58550,#58551,#58552),
(#58553,#58554,#58555,#58556),(#58557,#58558,#58559,#58560),(#58561,#58562,
#58563,#58564)),.UNSPECIFIED.,.F.,.F.,.F.,(4,4),(4,4),(0.,1.),(0.12699083482214,
0.28176419376589),.UNSPECIFIED.);
#184=B_SPLINE_SURFACE_WITH_KNOTS('',3,3,((#58578,#58579,#58580,#58581),
(#58582,#58583,#58584,#58585),(#58586,#58587,#58588,#58589),(#58590,#58591,
#58592,#58593)),.UNSPECIFIED.,.F.,.F.,.F.,(4,4),(4,4),(0.380102179091699,
1.),(0.23169515901548,0.246948509226624),.UNSPECIFIED.);
#185=B_SPLINE_SURFACE_WITH_KNOTS('',3,3,((#58611,#58612,#58613,#58614),
(#58615,#58616,#58617,#58618),(#58619,#58620,#58621,#58622),(#58623,#58624,
#58625,#58626)),.UNSPECIFIED.,.F.,.F.,.F.,(4,4),(4,4),(0.,1.),(0.12699083482214,
0.28176419376589),.UNSPECIFIED.);
#186=B_SPLINE_SURFACE_WITH_KNOTS('',3,3,((#58640,#58641,#58642,#58643),
(#58644,#58645,#58646,#58647),(#58648,#58649,#58650,#58651),(#58652,#58653,
#58654,#58655)),.UNSPECIFIED.,.F.,.F.,.F.,(4,4),(4,4),(0.380102179091715,
1.),(0.231695159015479,0.246948509226624),.UNSPECIFIED.);
#187=B_SPLINE_SURFACE_WITH_KNOTS('',3,3,((#58668,#58669,#58670,#58671),
(#58672,#58673,#58674,#58675),(#58676,#58677,#58678,#58679),(#58680,#58681,
#58682,#58683)),.UNSPECIFIED.,.F.,.F.,.F.,(4,4),(4,4),(0.,1.),(0.136758967931396,
0.281764193742676),.UNSPECIFIED.);
#188=B_SPLINE_SURFACE_WITH_KNOTS('',3,3,((#58688,#58689,#58690,#58691),
(#58692,#58693,#58694,#58695),(#58696,#58697,#58698,#58699),(#58700,#58701,
#58702,#58703)),.UNSPECIFIED.,.F.,.F.,.F.,(4,4),(4,4),(0.380102179091685,
1.),(0.111737484610932,0.12699083482214),.UNSPECIFIED.);
#189=B_SPLINE_SURFACE_WITH_KNOTS('',3,3,((#58713,#58714,#58715,#58716),
(#58717,#58718,#58719,#58720),(#58721,#58722,#58723,#58724),(#58725,#58726,
#58727,#58728)),.UNSPECIFIED.,.F.,.F.,.F.,(4,4),(4,4),(0.380102179091672,
1.),(0.111737484610932,0.12699083482214),.UNSPECIFIED.);
#190=B_SPLINE_SURFACE_WITH_KNOTS('',3,3,((#58738,#58739,#58740,#58741),
(#58742,#58743,#58744,#58745),(#58746,#58747,#58748,#58749),(#58750,#58751,
#58752,#58753)),.UNSPECIFIED.,.F.,.F.,.F.,(4,4),(4,4),(0.380102179091554,
1.),(0.111737484610934,0.12699083482214),.UNSPECIFIED.);
#191=B_SPLINE_SURFACE_WITH_KNOTS('',3,3,((#58763,#58764,#58765,#58766),
(#58767,#58768,#58769,#58770),(#58771,#58772,#58773,#58774),(#58775,#58776,
#58777,#58778)),.UNSPECIFIED.,.F.,.F.,.F.,(4,4),(4,4),(0.38010217909041,
1.),(0.111737484610934,0.12699083482214),.UNSPECIFIED.);
#192=B_SPLINE_SURFACE_WITH_KNOTS('',3,3,((#58783,#58784,#58785,#58786),
(#58787,#58788,#58789,#58790),(#58791,#58792,#58793,#58794),(#58795,#58796,
#58797,#58798)),.UNSPECIFIED.,.F.,.F.,.F.,(4,4),(4,4),(0.380102179090392,
1.),(0.11173748461093,0.126990834822138),.UNSPECIFIED.);
#193=B_SPLINE_SURFACE_WITH_KNOTS('',3,3,((#58808,#58809,#58810,#58811),
(#58812,#58813,#58814,#58815),(#58816,#58817,#58818,#58819),(#58820,#58821,
#58822,#58823)),.UNSPECIFIED.,.F.,.F.,.F.,(4,4),(4,4),(0.380102179090381,
1.),(0.111737484610934,0.126990834822142),.UNSPECIFIED.);
#194=B_SPLINE_SURFACE_WITH_KNOTS('',3,3,((#58833,#58834,#58835,#58836),
(#58837,#58838,#58839,#58840),(#58841,#58842,#58843,#58844),(#58845,#58846,
#58847,#58848)),.UNSPECIFIED.,.F.,.F.,.F.,(4,4),(4,4),(0.380102179090396,
1.),(0.111737484610932,0.126990834822139),.UNSPECIFIED.);
#195=B_SPLINE_SURFACE_WITH_KNOTS('',3,3,((#58858,#58859,#58860,#58861),
(#58862,#58863,#58864,#58865),(#58866,#58867,#58868,#58869),(#58870,#58871,
#58872,#58873)),.UNSPECIFIED.,.F.,.F.,.F.,(4,4),(4,4),(0.380102179090391,
1.),(0.11173748461093,0.126990834822138),.UNSPECIFIED.);
#196=B_SPLINE_SURFACE_WITH_KNOTS('',3,3,((#58883,#58884,#58885,#58886),
(#58887,#58888,#58889,#58890),(#58891,#58892,#58893,#58894),(#58895,#58896,
#58897,#58898)),.UNSPECIFIED.,.F.,.F.,.F.,(4,4),(4,4),(0.380102179090391,
1.),(0.111737484610934,0.126990834822142),.UNSPECIFIED.);
#197=FACE_BOUND('',#2305,.T.);
#198=FACE_BOUND('',#2391,.T.);
#199=FACE_BOUND('',#2395,.T.);
#200=FACE_BOUND('',#2424,.T.);
#201=FACE_BOUND('',#2515,.T.);
#202=FACE_BOUND('',#2517,.T.);
#203=FACE_BOUND('',#2583,.T.);
#204=FACE_BOUND('',#2589,.T.);
#205=FACE_BOUND('',#2595,.T.);
#206=FACE_BOUND('',#2619,.T.);
#207=FACE_BOUND('',#2624,.T.);
#208=FACE_BOUND('',#2627,.T.);
#209=FACE_BOUND('',#2630,.T.);
#210=FACE_BOUND('',#2631,.T.);
#211=FACE_BOUND('',#2632,.T.);
#212=FACE_BOUND('',#2633,.T.);
#213=FACE_BOUND('',#2634,.T.);
#214=FACE_BOUND('',#2635,.T.);
#215=FACE_BOUND('',#2636,.T.);
#216=FACE_BOUND('',#2637,.T.);
#217=FACE_BOUND('',#2638,.T.);
#218=FACE_BOUND('',#2639,.T.);
#219=FACE_BOUND('',#2646,.T.);
#220=FACE_BOUND('',#2647,.T.);
#221=FACE_BOUND('',#2648,.T.);
#222=FACE_BOUND('',#2649,.T.);
#223=FACE_BOUND('',#2650,.T.);
#224=FACE_BOUND('',#2651,.T.);
#225=FACE_BOUND('',#2652,.T.);
#226=FACE_BOUND('',#2653,.T.);
#227=FACE_BOUND('',#2654,.T.);
#228=FACE_BOUND('',#2655,.T.);
#229=FACE_BOUND('',#2864,.T.);
#230=FACE_BOUND('',#2866,.T.);
#231=FACE_BOUND('',#2871,.T.);
#232=FACE_BOUND('',#2872,.T.);
#233=FACE_BOUND('',#2873,.T.);
#234=FACE_BOUND('',#2874,.T.);
#235=FACE_BOUND('',#2875,.T.);
#236=FACE_BOUND('',#2876,.T.);
#237=FACE_BOUND('',#2877,.T.);
#238=FACE_BOUND('',#2882,.T.);
#239=FACE_BOUND('',#2887,.T.);
#240=FACE_BOUND('',#2892,.T.);
#241=FACE_BOUND('',#2922,.T.);
#242=FACE_BOUND('',#2925,.T.);
#243=FACE_BOUND('',#3069,.T.);
#244=FACE_BOUND('',#3090,.T.);
#245=FACE_BOUND('',#3095,.T.);
#246=FACE_BOUND('',#3113,.T.);
#247=FACE_BOUND('',#3114,.T.);
#248=FACE_BOUND('',#3115,.T.);
#249=FACE_BOUND('',#3117,.T.);
#250=FACE_BOUND('',#3119,.T.);
#251=FACE_BOUND('',#3125,.T.);
#252=FACE_BOUND('',#3128,.T.);
#253=FACE_BOUND('',#3129,.T.);
#254=FACE_BOUND('',#3130,.T.);
#255=FACE_BOUND('',#3131,.T.);
#256=FACE_BOUND('',#3132,.T.);
#257=FACE_BOUND('',#3133,.T.);
#258=FACE_BOUND('',#3134,.T.);
#259=FACE_BOUND('',#3137,.T.);
#260=FACE_BOUND('',#3141,.T.);
#261=FACE_BOUND('',#3142,.T.);
#262=FACE_BOUND('',#3145,.T.);
#263=FACE_BOUND('',#3146,.T.);
#264=PLANE('',#18483);
#265=PLANE('',#18485);
#266=PLANE('',#18486);
#267=PLANE('',#18487);
#268=PLANE('',#18488);
#269=PLANE('',#18489);
#270=PLANE('',#18490);
#271=PLANE('',#18491);
#272=PLANE('',#18492);
#273=PLANE('',#18493);
#274=PLANE('',#18494);
#275=PLANE('',#18495);
#276=PLANE('',#18496);
#277=PLANE('',#18497);
#278=PLANE('',#18498);
#279=PLANE('',#18499);
#280=PLANE('',#18500);
#281=PLANE('',#18501);
#282=PLANE('',#18502);
#283=PLANE('',#18503);
#284=PLANE('',#18504);
#285=PLANE('',#18505);
#286=PLANE('',#18506);
#287=PLANE('',#18507);
#288=PLANE('',#18508);
#289=PLANE('',#18509);
#290=PLANE('',#18510);
#291=PLANE('',#18511);
#292=PLANE('',#18512);
#293=PLANE('',#18513);
#294=PLANE('',#18514);
#295=PLANE('',#18515);
#296=PLANE('',#18516);
#297=PLANE('',#18517);
#298=PLANE('',#18518);
#299=PLANE('',#18519);
#300=PLANE('',#18520);
#301=PLANE('',#18521);
#302=PLANE('',#18522);
#303=PLANE('',#18523);
#304=PLANE('',#18524);
#305=PLANE('',#18525);
#306=PLANE('',#18526);
#307=PLANE('',#18527);
#308=PLANE('',#18528);
#309=PLANE('',#18529);
#310=PLANE('',#18530);
#311=PLANE('',#18531);
#312=PLANE('',#18595);
#313=PLANE('',#18602);
#314=PLANE('',#18606);
#315=PLANE('',#18617);
#316=PLANE('',#18621);
#317=PLANE('',#18629);
#318=PLANE('',#18633);
#319=PLANE('',#18641);
#320=PLANE('',#18645);
#321=PLANE('',#18653);
#322=PLANE('',#18657);
#323=PLANE('',#18665);
#324=PLANE('',#18669);
#325=PLANE('',#18686);
#326=PLANE('',#18691);
#327=PLANE('',#18696);
#328=PLANE('',#18701);
#329=PLANE('',#18706);
#330=PLANE('',#18711);
#331=PLANE('',#18716);
#332=PLANE('',#18721);
#333=PLANE('',#18726);
#334=PLANE('',#18731);
#335=PLANE('',#18736);
#336=PLANE('',#18741);
#337=PLANE('',#18752);
#338=PLANE('',#18755);
#339=PLANE('',#18760);
#340=PLANE('',#18763);
#341=PLANE('',#18768);
#342=PLANE('',#18771);
#343=PLANE('',#18776);
#344=PLANE('',#18781);
#345=PLANE('',#18786);
#346=PLANE('',#18791);
#347=PLANE('',#18796);
#348=PLANE('',#18801);
#349=PLANE('',#18806);
#350=PLANE('',#18811);
#351=PLANE('',#18816);
#352=PLANE('',#18819);
#353=PLANE('',#18825);
#354=PLANE('',#18826);
#355=PLANE('',#18831);
#356=PLANE('',#18833);
#357=PLANE('',#18834);
#358=PLANE('',#18836);
#359=PLANE('',#18837);
#360=PLANE('',#18839);
#361=PLANE('',#18840);
#362=PLANE('',#18842);
#363=PLANE('',#18843);
#364=PLANE('',#18845);
#365=PLANE('',#18846);
#366=PLANE('',#18848);
#367=PLANE('',#18849);
#368=PLANE('',#18851);
#369=PLANE('',#18852);
#370=PLANE('',#18854);
#371=PLANE('',#18855);
#372=PLANE('',#18857);
#373=PLANE('',#18858);
#374=PLANE('',#18860);
#375=PLANE('',#18861);
#376=PLANE('',#18863);
#377=PLANE('',#18864);
#378=PLANE('',#18866);
#379=PLANE('',#18867);
#380=PLANE('',#18868);
#381=PLANE('',#18869);
#382=PLANE('',#18870);
#383=PLANE('',#18871);
#384=PLANE('',#18872);
#385=PLANE('',#18873);
#386=PLANE('',#18874);
#387=PLANE('',#18875);
#388=PLANE('',#18876);
#389=PLANE('',#18877);
#390=PLANE('',#18878);
#391=PLANE('',#18879);
#392=PLANE('',#18880);
#393=PLANE('',#18881);
#394=PLANE('',#18888);
#395=PLANE('',#18898);
#396=PLANE('',#18915);
#397=PLANE('',#18917);
#398=PLANE('',#18918);
#399=PLANE('',#18919);
#400=PLANE('',#18920);
#401=PLANE('',#18929);
#402=PLANE('',#18937);
#403=PLANE('',#18939);
#404=PLANE('',#18940);
#405=PLANE('',#18942);
#406=PLANE('',#18943);
#407=PLANE('',#18951);
#408=PLANE('',#18955);
#409=PLANE('',#18956);
#410=PLANE('',#18957);
#411=PLANE('',#18981);
#412=PLANE('',#18982);
#413=PLANE('',#18983);
#414=PLANE('',#18984);
#415=PLANE('',#18985);
#416=PLANE('',#18986);
#417=PLANE('',#18987);
#418=PLANE('',#18988);
#419=PLANE('',#18989);
#420=PLANE('',#18990);
#421=PLANE('',#18991);
#422=PLANE('',#18992);
#423=PLANE('',#18993);
#424=PLANE('',#18994);
#425=PLANE('',#18995);
#426=PLANE('',#18996);
#427=PLANE('',#18997);
#428=PLANE('',#18998);
#429=PLANE('',#18999);
#430=PLANE('',#19000);
#431=PLANE('',#19001);
#432=PLANE('',#19002);
#433=PLANE('',#19003);
#434=PLANE('',#19004);
#435=PLANE('',#19005);
#436=PLANE('',#19006);
#437=PLANE('',#19007);
#438=PLANE('',#19008);
#439=PLANE('',#19009);
#440=PLANE('',#19010);
#441=PLANE('',#19011);
#442=PLANE('',#19012);
#443=PLANE('',#19013);
#444=PLANE('',#19014);
#445=PLANE('',#19015);
#446=PLANE('',#19016);
#447=PLANE('',#19017);
#448=PLANE('',#19018);
#449=PLANE('',#19019);
#450=PLANE('',#19020);
#451=PLANE('',#19021);
#452=PLANE('',#19022);
#453=PLANE('',#19023);
#454=PLANE('',#19024);
#455=PLANE('',#19025);
#456=PLANE('',#19026);
#457=PLANE('',#19027);
#458=PLANE('',#19028);
#459=PLANE('',#19029);
#460=PLANE('',#19030);
#461=PLANE('',#19031);
#462=PLANE('',#19032);
#463=PLANE('',#19033);
#464=PLANE('',#19034);
#465=PLANE('',#19035);
#466=PLANE('',#19036);
#467=PLANE('',#19037);
#468=PLANE('',#19038);
#469=PLANE('',#19039);
#470=PLANE('',#19040);
#471=PLANE('',#19041);
#472=PLANE('',#19042);
#473=PLANE('',#19043);
#474=PLANE('',#19044);
#475=PLANE('',#19045);
#476=PLANE('',#19046);
#477=PLANE('',#19047);
#478=PLANE('',#19048);
#479=PLANE('',#19049);
#480=PLANE('',#19050);
#481=PLANE('',#19051);
#482=PLANE('',#19052);
#483=PLANE('',#19053);
#484=PLANE('',#19054);
#485=PLANE('',#19055);
#486=PLANE('',#19056);
#487=PLANE('',#19057);
#488=PLANE('',#19058);
#489=PLANE('',#19059);
#490=PLANE('',#19060);
#491=PLANE('',#19061);
#492=PLANE('',#19062);
#493=PLANE('',#19063);
#494=PLANE('',#19064);
#495=PLANE('',#19065);
#496=PLANE('',#19066);
#497=PLANE('',#19067);
#498=PLANE('',#19068);
#499=PLANE('',#19069);
#500=PLANE('',#19070);
#501=PLANE('',#19071);
#502=PLANE('',#19072);
#503=PLANE('',#19073);
#504=PLANE('',#19074);
#505=PLANE('',#19075);
#506=PLANE('',#19076);
#507=PLANE('',#19077);
#508=PLANE('',#19078);
#509=PLANE('',#19079);
#510=PLANE('',#19080);
#511=PLANE('',#19081);
#512=PLANE('',#19082);
#513=PLANE('',#19083);
#514=PLANE('',#19084);
#515=PLANE('',#19085);
#516=PLANE('',#19086);
#517=PLANE('',#19087);
#518=PLANE('',#19088);
#519=PLANE('',#19089);
#520=PLANE('',#19090);
#521=PLANE('',#19091);
#522=PLANE('',#19092);
#523=PLANE('',#19093);
#524=PLANE('',#19094);
#525=PLANE('',#19095);
#526=PLANE('',#19096);
#527=PLANE('',#19097);
#528=PLANE('',#19098);
#529=PLANE('',#19099);
#530=PLANE('',#19100);
#531=PLANE('',#19101);
#532=PLANE('',#19102);
#533=PLANE('',#19103);
#534=PLANE('',#19104);
#535=PLANE('',#19105);
#536=PLANE('',#19106);
#537=PLANE('',#19107);
#538=PLANE('',#19108);
#539=PLANE('',#19109);
#540=PLANE('',#19110);
#541=PLANE('',#19111);
#542=PLANE('',#19112);
#543=PLANE('',#19113);
#544=PLANE('',#19114);
#545=PLANE('',#19115);
#546=PLANE('',#19116);
#547=PLANE('',#19117);
#548=PLANE('',#19118);
#549=PLANE('',#19119);
#550=PLANE('',#19120);
#551=PLANE('',#19121);
#552=PLANE('',#19122);
#553=PLANE('',#19123);
#554=PLANE('',#19124);
#555=PLANE('',#19125);
#556=PLANE('',#19126);
#557=PLANE('',#19127);
#558=PLANE('',#19128);
#559=PLANE('',#19129);
#560=PLANE('',#19130);
#561=PLANE('',#19131);
#562=PLANE('',#19132);
#563=PLANE('',#19133);
#564=PLANE('',#19134);
#565=PLANE('',#19135);
#566=PLANE('',#19136);
#567=PLANE('',#19137);
#568=PLANE('',#19138);
#569=PLANE('',#19139);
#570=PLANE('',#19140);
#571=PLANE('',#19141);
#572=PLANE('',#19142);
#573=PLANE('',#19143);
#574=PLANE('',#19144);
#575=PLANE('',#19145);
#576=PLANE('',#19146);
#577=PLANE('',#19147);
#578=PLANE('',#19148);
#579=PLANE('',#19149);
#580=PLANE('',#19150);
#581=PLANE('',#19151);
#582=PLANE('',#19152);
#583=PLANE('',#19153);
#584=PLANE('',#19154);
#585=PLANE('',#19155);
#586=PLANE('',#19156);
#587=PLANE('',#19157);
#588=PLANE('',#19158);
#589=PLANE('',#19159);
#590=PLANE('',#19160);
#591=PLANE('',#19162);
#592=PLANE('',#19167);
#593=PLANE('',#19171);
#594=PLANE('',#19175);
#595=PLANE('',#19179);
#596=PLANE('',#19183);
#597=PLANE('',#19187);
#598=PLANE('',#19191);
#599=PLANE('',#19193);
#600=PLANE('',#19202);
#601=PLANE('',#19210);
#602=PLANE('',#19217);
#603=PLANE('',#19225);
#604=PLANE('',#19227);
#605=PLANE('',#19228);
#606=PLANE('',#19229);
#607=PLANE('',#19230);
#608=PLANE('',#19300);
#609=PLANE('',#19304);
#610=PLANE('',#19306);
#611=PLANE('',#19310);
#612=PLANE('',#19314);
#613=PLANE('',#19318);
#614=PLANE('',#19322);
#615=PLANE('',#19326);
#616=PLANE('',#19330);
#617=PLANE('',#19333);
#618=PLANE('',#19337);
#619=PLANE('',#19341);
#620=PLANE('',#19345);
#621=PLANE('',#19349);
#622=PLANE('',#19353);
#623=PLANE('',#19359);
#624=PLANE('',#19369);
#625=PLANE('',#19370);
#626=PLANE('',#19371);
#627=PLANE('',#19372);
#628=PLANE('',#19373);
#629=PLANE('',#19374);
#630=PLANE('',#19375);
#631=PLANE('',#19376);
#632=PLANE('',#19379);
#633=PLANE('',#19380);
#634=PLANE('',#19381);
#635=PLANE('',#19382);
#636=PLANE('',#19383);
#637=PLANE('',#19384);
#638=PLANE('',#19385);
#639=PLANE('',#19386);
#640=PLANE('',#19387);
#641=PLANE('',#19388);
#642=PLANE('',#19389);
#643=PLANE('',#19390);
#644=PLANE('',#19391);
#645=PLANE('',#19392);
#646=PLANE('',#19393);
#647=PLANE('',#19394);
#648=PLANE('',#19395);
#649=PLANE('',#19396);
#650=PLANE('',#19397);
#651=PLANE('',#19398);
#652=PLANE('',#19399);
#653=PLANE('',#19422);
#654=PLANE('',#19423);
#655=PLANE('',#19424);
#656=PLANE('',#19425);
#657=PLANE('',#19426);
#658=PLANE('',#19427);
#659=PLANE('',#19428);
#660=PLANE('',#19429);
#661=PLANE('',#19431);
#662=PLANE('',#19439);
#663=PLANE('',#19441);
#664=PLANE('',#19446);
#665=PLANE('',#19448);
#666=PLANE('',#19453);
#667=PLANE('',#19455);
#668=PLANE('',#19460);
#669=PLANE('',#19462);
#670=PLANE('',#19467);
#671=PLANE('',#19476);
#672=PLANE('',#19478);
#673=PLANE('',#19488);
#674=PLANE('',#19496);
#675=PLANE('',#19503);
#676=PLANE('',#19507);
#677=PLANE('',#19514);
#678=PLANE('',#19515);
#679=PLANE('',#19516);
#680=PLANE('',#19517);
#681=PLANE('',#19518);
#682=PLANE('',#19519);
#683=PLANE('',#19520);
#684=PLANE('',#19521);
#685=PLANE('',#19522);
#686=PLANE('',#19523);
#687=PLANE('',#19524);
#688=PLANE('',#19525);
#689=PLANE('',#19526);
#690=PLANE('',#19527);
#691=PLANE('',#19528);
#692=PLANE('',#19529);
#693=PLANE('',#19530);
#694=PLANE('',#19531);
#695=PLANE('',#19532);
#696=PLANE('',#19533);
#697=PLANE('',#19534);
#698=PLANE('',#19535);
#699=PLANE('',#19536);
#700=PLANE('',#19537);
#701=PLANE('',#19538);
#702=PLANE('',#19539);
#703=PLANE('',#19540);
#704=PLANE('',#19541);
#705=PLANE('',#19542);
#706=PLANE('',#19543);
#707=PLANE('',#19544);
#708=PLANE('',#19545);
#709=PLANE('',#19546);
#710=PLANE('',#19547);
#711=PLANE('',#19548);
#712=PLANE('',#19549);
#713=PLANE('',#19550);
#714=PLANE('',#19551);
#715=PLANE('',#19552);
#716=PLANE('',#19553);
#717=PLANE('',#19554);
#718=PLANE('',#19555);
#719=PLANE('',#19556);
#720=PLANE('',#19557);
#721=PLANE('',#19558);
#722=PLANE('',#19559);
#723=PLANE('',#19560);
#724=PLANE('',#19561);
#725=PLANE('',#19562);
#726=PLANE('',#19563);
#727=PLANE('',#19564);
#728=PLANE('',#19565);
#729=PLANE('',#19566);
#730=PLANE('',#19567);
#731=PLANE('',#19568);
#732=PLANE('',#19569);
#733=PLANE('',#19570);
#734=PLANE('',#19571);
#735=PLANE('',#19572);
#736=PLANE('',#19573);
#737=PLANE('',#19574);
#738=PLANE('',#19575);
#739=PLANE('',#19576);
#740=PLANE('',#19577);
#741=PLANE('',#19578);
#742=PLANE('',#19579);
#743=PLANE('',#19580);
#744=PLANE('',#19581);
#745=PLANE('',#19582);
#746=PLANE('',#19583);
#747=PLANE('',#19584);
#748=PLANE('',#19585);
#749=PLANE('',#19586);
#750=PLANE('',#19587);
#751=PLANE('',#19588);
#752=PLANE('',#19589);
#753=PLANE('',#19590);
#754=PLANE('',#19591);
#755=PLANE('',#19592);
#756=PLANE('',#19593);
#757=PLANE('',#19594);
#758=PLANE('',#19595);
#759=PLANE('',#19596);
#760=PLANE('',#19597);
#761=PLANE('',#19598);
#762=PLANE('',#19599);
#763=PLANE('',#19600);
#764=PLANE('',#19601);
#765=PLANE('',#19602);
#766=PLANE('',#19603);
#767=PLANE('',#19604);
#768=PLANE('',#19605);
#769=PLANE('',#19606);
#770=PLANE('',#19607);
#771=PLANE('',#19608);
#772=PLANE('',#19609);
#773=PLANE('',#19610);
#774=PLANE('',#19611);
#775=PLANE('',#19612);
#776=PLANE('',#19613);
#777=PLANE('',#19614);
#778=PLANE('',#19615);
#779=PLANE('',#19616);
#780=PLANE('',#19617);
#781=PLANE('',#19618);
#782=PLANE('',#19619);
#783=PLANE('',#19620);
#784=PLANE('',#19621);
#785=PLANE('',#19622);
#786=PLANE('',#19623);
#787=PLANE('',#19624);
#788=PLANE('',#19625);
#789=PLANE('',#19626);
#790=PLANE('',#19627);
#791=PLANE('',#19628);
#792=PLANE('',#19629);
#793=PLANE('',#19630);
#794=PLANE('',#19631);
#795=PLANE('',#19632);
#796=PLANE('',#19633);
#797=PLANE('',#19634);
#798=PLANE('',#19635);
#799=PLANE('',#19636);
#800=PLANE('',#19637);
#801=PLANE('',#19638);
#802=PLANE('',#19639);
#803=PLANE('',#19640);
#804=PLANE('',#19641);
#805=PLANE('',#19642);
#806=PLANE('',#19643);
#807=PLANE('',#19644);
#808=PLANE('',#19645);
#809=PLANE('',#19646);
#810=PLANE('',#19647);
#811=PLANE('',#19648);
#812=PLANE('',#19649);
#813=PLANE('',#19650);
#814=PLANE('',#19651);
#815=PLANE('',#19652);
#816=PLANE('',#19653);
#817=PLANE('',#19654);
#818=PLANE('',#19655);
#819=PLANE('',#19656);
#820=PLANE('',#19657);
#821=PLANE('',#19658);
#822=PLANE('',#19659);
#823=PLANE('',#19660);
#824=PLANE('',#19661);
#825=PLANE('',#19662);
#826=PLANE('',#19663);
#827=CONICAL_SURFACE('',#18477,9.87862393885688,1.05560791353274);
#828=CONICAL_SURFACE('',#18481,10.3,0.540419500270582);
#829=CONICAL_SURFACE('',#18532,34.75,0.785398163397448);
#830=CONICAL_SURFACE('',#18537,34.75,0.785398163397448);
#831=CONICAL_SURFACE('',#18542,34.75,0.785398163397453);
#832=CONICAL_SURFACE('',#18547,34.75,0.785398163397448);
#833=CONICAL_SURFACE('',#18552,34.75,0.785398163397453);
#834=CONICAL_SURFACE('',#18557,34.75,0.785398163397443);
#835=CONICAL_SURFACE('',#18562,34.75,0.785398163397448);
#836=CONICAL_SURFACE('',#18567,34.75,0.785398163397456);
#837=CONICAL_SURFACE('',#18572,34.75,0.785398163397453);
#838=CONICAL_SURFACE('',#18577,34.75,0.785398163397448);
#839=CONICAL_SURFACE('',#18582,34.75,0.785398163397448);
#840=CONICAL_SURFACE('',#18587,34.75,0.785398163397453);
#841=CONICAL_SURFACE('',#18592,8.95,0.785398163397451);
#842=CONICAL_SURFACE('',#18599,8.95,0.785398163397451);
#843=CONICAL_SURFACE('',#18607,8.25,0.785398163397452);
#844=CONICAL_SURFACE('',#18610,32.75,0.785398163397439);
#845=CONICAL_SURFACE('',#18618,8.25,0.785398163397449);
#846=CONICAL_SURFACE('',#18622,32.75,0.785398163397439);
#847=CONICAL_SURFACE('',#18630,8.25,0.785398163397451);
#848=CONICAL_SURFACE('',#18634,32.75,0.785398163397439);
#849=CONICAL_SURFACE('',#18642,8.25,0.785398163397452);
#850=CONICAL_SURFACE('',#18646,32.75,0.785398163397439);
#851=CONICAL_SURFACE('',#18654,8.25,0.785398163397449);
#852=CONICAL_SURFACE('',#18658,32.75,0.785398163397439);
#853=CONICAL_SURFACE('',#18666,8.25,0.785398163397451);
#854=CONICAL_SURFACE('',#18684,32.75,0.785398163397439);
#855=CONICAL_SURFACE('',#18697,8.25,0.785398163397452);
#856=CONICAL_SURFACE('',#18699,32.75,0.785398163397439);
#857=CONICAL_SURFACE('',#18707,8.25,0.785398163397454);
#858=CONICAL_SURFACE('',#18709,32.75,0.785398163397439);
#859=CONICAL_SURFACE('',#18717,8.25,0.785398163397451);
#860=CONICAL_SURFACE('',#18719,32.75,0.785398163397439);
#861=CONICAL_SURFACE('',#18727,8.25,0.785398163397452);
#862=CONICAL_SURFACE('',#18729,32.75,0.785398163397439);
#863=CONICAL_SURFACE('',#18737,8.25,0.78539816339745);
#864=CONICAL_SURFACE('',#18739,32.75,0.785398163397439);
#865=CONICAL_SURFACE('',#18747,32.75,0.785398163397439);
#866=CONICAL_SURFACE('',#18753,8.25,0.785398163397451);
#867=CONICAL_SURFACE('',#18756,32.7,0.876058050598196);
#868=CONICAL_SURFACE('',#18770,32.7,0.876058050598196);
#869=CONICAL_SURFACE('',#18774,32.7,0.876058050598196);
#870=CONICAL_SURFACE('',#18775,32.7,0.876058050598196);
#871=CONICAL_SURFACE('',#18779,32.7,0.876058050598196);
#872=CONICAL_SURFACE('',#18780,32.7,0.876058050598196);
#873=CONICAL_SURFACE('',#18784,32.7,0.876058050598196);
#874=CONICAL_SURFACE('',#18785,32.7,0.876058050598196);
#875=CONICAL_SURFACE('',#18789,32.7,0.876058050598196);
#876=CONICAL_SURFACE('',#18790,32.7,0.876058050598196);
#877=CONICAL_SURFACE('',#18794,32.7,0.876058050598196);
#878=CONICAL_SURFACE('',#18795,32.7,0.876058050598196);
#879=CONICAL_SURFACE('',#18799,32.7,0.876058050598196);
#880=CONICAL_SURFACE('',#18800,32.7,0.876058050598196);
#881=CONICAL_SURFACE('',#18804,32.7,0.876058050598196);
#882=CONICAL_SURFACE('',#18805,32.7,0.876058050598196);
#883=CONICAL_SURFACE('',#18809,32.7,0.876058050598196);
#884=CONICAL_SURFACE('',#18810,32.7,0.876058050598196);
#885=CONICAL_SURFACE('',#18814,32.7,0.876058050598196);
#886=CONICAL_SURFACE('',#18815,32.7,0.876058050598196);
#887=CONICAL_SURFACE('',#18817,32.7,0.876058050598196);
#888=CONICAL_SURFACE('',#18818,32.7,0.876058050598196);
#889=CONICAL_SURFACE('',#18820,32.7,0.876058050598196);
#890=CONICAL_SURFACE('',#18821,32.7,0.876058050598196);
#891=CONICAL_SURFACE('',#18882,13.,1.23412150740817);
#892=CONICAL_SURFACE('',#18884,11.3,1.05165021254838);
#893=CONICAL_SURFACE('',#18885,9.,0.785398163397459);
#894=CONICAL_SURFACE('',#18886,9.,0.785398163397448);
#895=CONICAL_SURFACE('',#18890,6.7,0.785398163397446);
#896=CONICAL_SURFACE('',#18892,5.85,0.950546840812077);
#897=CONICAL_SURFACE('',#18896,5.35,0.785398163397459);
#898=CONICAL_SURFACE('',#18902,3.4,0.785398163397415);
#899=CONICAL_SURFACE('',#18906,3.2,1.24904577239829);
#900=CONICAL_SURFACE('',#18910,3.2,1.10714871779408);
#901=CONICAL_SURFACE('',#18913,3.25,0.785398163397441);
#902=CONICAL_SURFACE('',#18922,8.4,0.785398163397446);
#903=CONICAL_SURFACE('',#18927,8.35,0.982793723247329);
#904=CONICAL_SURFACE('',#18931,3.6575,0.7936624380571);
#905=CONICAL_SURFACE('',#18935,3.6575,0.7936624380571);
#906=CONICAL_SURFACE('',#18949,16.9,0.785398163397449);
#907=CONICAL_SURFACE('',#18952,16.9,0.785398163397448);
#908=CONICAL_SURFACE('',#18963,2.75,0.785398163397449);
#909=CONICAL_SURFACE('',#18967,2.75,0.785398163397448);
#910=CONICAL_SURFACE('',#18968,2.75,0.785398163397449);
#911=CONICAL_SURFACE('',#18972,2.75,0.785398163397448);
#912=CONICAL_SURFACE('',#18973,2.75,0.785398163397449);
#913=CONICAL_SURFACE('',#18977,2.75,0.785398163397448);
#914=CONICAL_SURFACE('',#18978,1.1,0.785398163397448);
#915=CONICAL_SURFACE('',#19197,5.65,0.785398163397449);
#916=CONICAL_SURFACE('',#19204,8.4,0.785398163397446);
#917=CONICAL_SURFACE('',#19208,8.4,0.785398163397446);
#918=CONICAL_SURFACE('',#19212,7.7,0.785398163397448);
#919=CONICAL_SURFACE('',#19215,7.45,0.785398163397448);
#920=CONICAL_SURFACE('',#19219,3.6575,0.7936624380571);
#921=CONICAL_SURFACE('',#19223,3.6575,0.7936624380571);
#922=CONICAL_SURFACE('',#19234,38.7702137424955,0.582952270254907);
#923=CONICAL_SURFACE('',#19267,38.7702137424955,0.582952270254903);
#924=CONICAL_SURFACE('',#19269,38.7702137424955,0.582952270254907);
#925=CONICAL_SURFACE('',#19271,38.7702137424955,0.582952270254917);
#926=CONICAL_SURFACE('',#19273,38.7702137424955,0.582952270254906);
#927=CONICAL_SURFACE('',#19275,38.7702137424955,0.582952270254903);
#928=CONICAL_SURFACE('',#19277,38.7702137424955,0.582952270254906);
#929=CONICAL_SURFACE('',#19279,38.7702137424955,0.582952270254907);
#930=CONICAL_SURFACE('',#19281,38.7702137424955,0.582952270254906);
#931=CONICAL_SURFACE('',#19283,38.7702137424955,0.582952270254906);
#932=CONICAL_SURFACE('',#19285,38.7702137424955,0.582952270254902);
#933=CONICAL_SURFACE('',#19287,38.7702137424955,0.582952270254911);
#934=CONICAL_SURFACE('',#19289,38.7702137424955,0.582952270254907);
#935=CONICAL_SURFACE('',#19291,38.7702137424955,0.582952270254902);
#936=CONICAL_SURFACE('',#19293,3.675,0.785398163397447);
#937=CONICAL_SURFACE('',#19302,3.675,0.785398163397451);
#938=CONICAL_SURFACE('',#19308,38.3,1.16590454050981);
#939=CONICAL_SURFACE('',#19312,38.3,1.16590454050981);
#940=CONICAL_SURFACE('',#19316,38.3,1.16590454050981);
#941=CONICAL_SURFACE('',#19320,38.3,1.16590454050981);
#942=CONICAL_SURFACE('',#19324,38.3,1.16590454050981);
#943=CONICAL_SURFACE('',#19328,38.3,1.16590454050981);
#944=CONICAL_SURFACE('',#19332,38.3,1.16590454050981);
#945=CONICAL_SURFACE('',#19335,38.3,1.16590454050981);
#946=CONICAL_SURFACE('',#19339,38.3,1.16590454050981);
#947=CONICAL_SURFACE('',#19343,38.3,1.16590454050981);
#948=CONICAL_SURFACE('',#19347,38.3,1.16590454050981);
#949=CONICAL_SURFACE('',#19351,38.3,1.16590454050981);
#950=CONICAL_SURFACE('',#19355,38.3,1.16590454050981);
#951=CONICAL_SURFACE('',#19361,38.75,0.785398163397447);
#952=CONICAL_SURFACE('',#19362,38.3,1.16590454050981);
#953=CONICAL_SURFACE('',#19363,8.95,1.19028994968254);
#954=CONICAL_SURFACE('',#19367,8.4,0.785398163397447);
#955=CONICAL_SURFACE('',#19377,5.3,0.862170054667227);
#956=CONICAL_SURFACE('',#19409,5.3,0.862170054667227);
#957=CONICAL_SURFACE('',#19410,5.3,0.862170054667227);
#958=CONICAL_SURFACE('',#19411,5.3,0.862170054667227);
#959=CONICAL_SURFACE('',#19412,5.3,0.862170054667227);
#960=CONICAL_SURFACE('',#19413,5.3,0.862170054667227);
#961=CONICAL_SURFACE('',#19414,5.3,0.862170054667227);
#962=CONICAL_SURFACE('',#19415,5.3,0.862170054667227);
#963=CONICAL_SURFACE('',#19416,5.3,0.862170054667227);
#964=CONICAL_SURFACE('',#19417,3.8,0.785398163397448);
#965=CONICAL_SURFACE('',#19419,3.8,0.785398163397448);
#966=CONICAL_SURFACE('',#19433,6.35,0.785398163397449);
#967=CONICAL_SURFACE('',#19437,6.25,1.19028994968253);
#968=CONICAL_SURFACE('',#19482,8.6,0.785398163397449);
#969=CONICAL_SURFACE('',#19486,8.6,0.785398163397448);
#970=CONICAL_SURFACE('',#19490,5.67,0.78539816339745);
#971=CONICAL_SURFACE('',#19494,5.67,0.785398163397451);
#972=CONICAL_SURFACE('',#19498,0.650000000000001,0.785398163397449);
#973=CONICAL_SURFACE('',#19505,0.650000000000001,0.785398163397449);
#974=CONICAL_SURFACE('',#19509,0.650000000000001,0.785398163397449);
#975=CONICAL_SURFACE('',#19513,0.650000000000001,0.785398163397449);
#976=(
BOUNDED_CURVE()
B_SPLINE_CURVE(5,(#24658,#24659,#24660,#24661,#24662,#24663,#24664,#24665,
#24666,#24667,#24668),.UNSPECIFIED.,.F.,.F.)
B_SPLINE_CURVE_WITH_KNOTS((6,1,1,1,1,1,6),(0.167063732147151,0.2,0.24,0.28,
0.32,0.36,0.378267291341468),.UNSPECIFIED.)
CURVE()
GEOMETRIC_REPRESENTATION_ITEM()
RATIONAL_B_SPLINE_CURVE((1.,1.,1.,1.,1.,1.,1.,1.,1.,1.,1.))
REPRESENTATION_ITEM('')
);
#977=(
BOUNDED_CURVE()
B_SPLINE_CURVE(5,(#24696,#24697,#24698,#24699,#24700,#24701),
 .UNSPECIFIED.,.F.,.F.)
B_SPLINE_CURVE_WITH_KNOTS((6,6),(0.,0.0177013282315284),.UNSPECIFIED.)
CURVE()
GEOMETRIC_REPRESENTATION_ITEM()
RATIONAL_B_SPLINE_CURVE((1.,1.,1.,1.,1.,1.))
REPRESENTATION_ITEM('')
);
#978=(
BOUNDED_CURVE()
B_SPLINE_CURVE(2,(#32858,#32859,#32860),.UNSPECIFIED.,.F.,.F.)
B_SPLINE_CURVE_WITH_KNOTS((3,3),(0.0642390630877484,0.159883011113203),
 .UNSPECIFIED.)
CURVE()
GEOMETRIC_REPRESENTATION_ITEM()
RATIONAL_B_SPLINE_CURVE((1.00013237845317,1.00016634217764,1.00000799154408))
REPRESENTATION_ITEM('')
);
#979=(
BOUNDED_CURVE()
B_SPLINE_CURVE(2,(#32864,#32865,#32866),.UNSPECIFIED.,.F.,.F.)
B_SPLINE_CURVE_WITH_KNOTS((3,3),(0.000526061815849738,0.0490373321941988),
 .UNSPECIFIED.)
CURVE()
GEOMETRIC_REPRESENTATION_ITEM()
RATIONAL_B_SPLINE_CURVE((1.00000140604824,1.00006598064969,1.00008344962655))
REPRESENTATION_ITEM('')
);
#980=(
BOUNDED_CURVE()
B_SPLINE_CURVE(2,(#32868,#32869,#32870),.UNSPECIFIED.,.F.,.F.)
B_SPLINE_CURVE_WITH_KNOTS((3,3),(0.0729556909351875,0.123986559684229),
 .UNSPECIFIED.)
CURVE()
GEOMETRIC_REPRESENTATION_ITEM()
RATIONAL_B_SPLINE_CURVE((1.00116052526037,1.0009929348209,1.00002308400869))
REPRESENTATION_ITEM('')
);
#981=(
BOUNDED_CURVE()
B_SPLINE_CURVE(2,(#32886,#32887,#32888),.UNSPECIFIED.,.F.,.F.)
B_SPLINE_CURVE_WITH_KNOTS((3,3),(0.0378274750358814,0.0817111642791895),
 .UNSPECIFIED.)
CURVE()
GEOMETRIC_REPRESENTATION_ITEM()
RATIONAL_B_SPLINE_CURVE((1.01190199115935,1.01846995640957,1.02425882037767))
REPRESENTATION_ITEM('')
);
#982=(
BOUNDED_CURVE()
B_SPLINE_CURVE(2,(#32894,#32895,#32896),.UNSPECIFIED.,.F.,.F.)
B_SPLINE_CURVE_WITH_KNOTS((3,3),(0.0850178447349258,0.133529115174433),
 .UNSPECIFIED.)
CURVE()
GEOMETRIC_REPRESENTATION_ITEM()
RATIONAL_B_SPLINE_CURVE((1.00008344962585,1.00006598064918,1.00000140604823))
REPRESENTATION_ITEM('')
);
#983=(
BOUNDED_CURVE()
B_SPLINE_CURVE(2,(#32917,#32918,#32919),.UNSPECIFIED.,.F.,.F.)
B_SPLINE_CURVE_WITH_KNOTS((3,3),(0.00295018481962982,0.0985937601702449),
 .UNSPECIFIED.)
CURVE()
GEOMETRIC_REPRESENTATION_ITEM()
RATIONAL_B_SPLINE_CURVE((1.00000995626948,1.00016837897441,1.00013448693778))
REPRESENTATION_ITEM('')
);
#984=(
BOUNDED_CURVE()
B_SPLINE_CURVE(2,(#32922,#32923,#32924),.UNSPECIFIED.,.F.,.F.)
B_SPLINE_CURVE_WITH_KNOTS((3,3),(0.000473184985766772,0.0515065306432952),
 .UNSPECIFIED.)
CURVE()
GEOMETRIC_REPRESENTATION_ITEM()
RATIONAL_B_SPLINE_CURVE((1.00001807280714,1.00098893623079,1.00115754364118))
REPRESENTATION_ITEM('')
);
#985=(
BOUNDED_CURVE()
B_SPLINE_CURVE(2,(#32929,#32930,#32931),.UNSPECIFIED.,.F.,.F.)
B_SPLINE_CURVE_WITH_KNOTS((3,3),(0.072955690935184,0.123986559684228),
 .UNSPECIFIED.)
CURVE()
GEOMETRIC_REPRESENTATION_ITEM()
RATIONAL_B_SPLINE_CURVE((1.00116052526042,1.00099293482093,1.00002308400869))
REPRESENTATION_ITEM('')
);
#986=(
BOUNDED_CURVE()
B_SPLINE_CURVE(2,(#32941,#32942,#32943),.UNSPECIFIED.,.F.,.F.)
B_SPLINE_CURVE_WITH_KNOTS((3,3),(0.0642390630877414,0.159883011113205),
 .UNSPECIFIED.)
CURVE()
GEOMETRIC_REPRESENTATION_ITEM()
RATIONAL_B_SPLINE_CURVE((1.00013237845415,1.00016634217886,1.00000799154414))
REPRESENTATION_ITEM('')
);
#987=(
BOUNDED_CURVE()
B_SPLINE_CURVE(2,(#32946,#32947,#32948),.UNSPECIFIED.,.F.,.F.)
B_SPLINE_CURVE_WITH_KNOTS((3,3),(0.000526061815844321,0.0490373321941647),
 .UNSPECIFIED.)
CURVE()
GEOMETRIC_REPRESENTATION_ITEM()
RATIONAL_B_SPLINE_CURVE((1.00000140604826,1.00006598065031,1.00008344962734))
REPRESENTATION_ITEM('')
);
#988=(
BOUNDED_CURVE()
B_SPLINE_CURVE(2,(#32954,#32955,#32956),.UNSPECIFIED.,.F.,.F.)
B_SPLINE_CURVE_WITH_KNOTS((3,3),(0.0850178447349365,0.133529115174432),
 .UNSPECIFIED.)
CURVE()
GEOMETRIC_REPRESENTATION_ITEM()
RATIONAL_B_SPLINE_CURVE((1.00008344962713,1.0000659806502,1.00000140604825))
REPRESENTATION_ITEM('')
);
#989=(
BOUNDED_CURVE()
B_SPLINE_CURVE(2,(#32977,#32978,#32979),.UNSPECIFIED.,.F.,.F.)
B_SPLINE_CURVE_WITH_KNOTS((3,3),(0.0029501848132628,0.0985937601638959),
 .UNSPECIFIED.)
CURVE()
GEOMETRIC_REPRESENTATION_ITEM()
RATIONAL_B_SPLINE_CURVE((1.00000995626947,1.00016837897463,1.00013448693795))
REPRESENTATION_ITEM('')
);
#990=(
BOUNDED_CURVE()
B_SPLINE_CURVE(2,(#32982,#32983,#32984),.UNSPECIFIED.,.F.,.F.)
B_SPLINE_CURVE_WITH_KNOTS((3,3),(0.000473184985766719,0.0515065306433004),
 .UNSPECIFIED.)
CURVE()
GEOMETRIC_REPRESENTATION_ITEM()
RATIONAL_B_SPLINE_CURVE((1.00001807280713,1.00098893623043,1.00115754364076))
REPRESENTATION_ITEM('')
);
#991=(
BOUNDED_CURVE()
B_SPLINE_CURVE(2,(#32989,#32990,#32991),.UNSPECIFIED.,.F.,.F.)
B_SPLINE_CURVE_WITH_KNOTS((3,3),(0.0729556909351876,0.123986559684229),
 .UNSPECIFIED.)
CURVE()
GEOMETRIC_REPRESENTATION_ITEM()
RATIONAL_B_SPLINE_CURVE((1.00116052526059,1.00099293482108,1.0000230840087))
REPRESENTATION_ITEM('')
);
#992=(
BOUNDED_CURVE()
B_SPLINE_CURVE(2,(#33001,#33002,#33003),.UNSPECIFIED.,.F.,.F.)
B_SPLINE_CURVE_WITH_KNOTS((3,3),(0.0642390630877381,0.159883011113203),
 .UNSPECIFIED.)
CURVE()
GEOMETRIC_REPRESENTATION_ITEM()
RATIONAL_B_SPLINE_CURVE((1.00013237845351,1.00016634217805,1.0000079915441))
REPRESENTATION_ITEM('')
);
#993=(
BOUNDED_CURVE()
B_SPLINE_CURVE(2,(#33006,#33007,#33008),.UNSPECIFIED.,.F.,.F.)
B_SPLINE_CURVE_WITH_KNOTS((3,3),(0.000526061815846924,0.0490373321942014),
 .UNSPECIFIED.)
CURVE()
GEOMETRIC_REPRESENTATION_ITEM()
RATIONAL_B_SPLINE_CURVE((1.00000140604824,1.00006598064965,1.0000834496265))
REPRESENTATION_ITEM('')
);
#994=(
BOUNDED_CURVE()
B_SPLINE_CURVE(2,(#33014,#33015,#33016),.UNSPECIFIED.,.F.,.F.)
B_SPLINE_CURVE_WITH_KNOTS((3,3),(0.0850178447349793,0.133529115174434),
 .UNSPECIFIED.)
CURVE()
GEOMETRIC_REPRESENTATION_ITEM()
RATIONAL_B_SPLINE_CURVE((1.00008344962783,1.00006598065075,1.00000140604826))
REPRESENTATION_ITEM('')
);
#995=(
BOUNDED_CURVE()
B_SPLINE_CURVE(2,(#33037,#33038,#33039),.UNSPECIFIED.,.F.,.F.)
B_SPLINE_CURVE_WITH_KNOTS((3,3),(0.00295018481782719,0.0985937601684328),
 .UNSPECIFIED.)
CURVE()
GEOMETRIC_REPRESENTATION_ITEM()
RATIONAL_B_SPLINE_CURVE((1.00000995626944,1.00016837897378,1.00013448693728))
REPRESENTATION_ITEM('')
);
#996=(
BOUNDED_CURVE()
B_SPLINE_CURVE(2,(#33042,#33043,#33044),.UNSPECIFIED.,.F.,.F.)
B_SPLINE_CURVE_WITH_KNOTS((3,3),(0.00047318498576828,0.0515065306432978),
 .UNSPECIFIED.)
CURVE()
GEOMETRIC_REPRESENTATION_ITEM()
RATIONAL_B_SPLINE_CURVE((1.00001807280714,1.00098893623049,1.00115754364084))
REPRESENTATION_ITEM('')
);
#997=(
BOUNDED_CURVE()
B_SPLINE_CURVE(2,(#33049,#33050,#33051),.UNSPECIFIED.,.F.,.F.)
B_SPLINE_CURVE_WITH_KNOTS((3,3),(0.0729556909351862,0.123986559684229),
 .UNSPECIFIED.)
CURVE()
GEOMETRIC_REPRESENTATION_ITEM()
RATIONAL_B_SPLINE_CURVE((1.00116052526039,1.00099293482091,1.00002308400869))
REPRESENTATION_ITEM('')
);
#998=(
BOUNDED_CURVE()
B_SPLINE_CURVE(2,(#33061,#33062,#33063),.UNSPECIFIED.,.F.,.F.)
B_SPLINE_CURVE_WITH_KNOTS((3,3),(0.0642390630877591,0.159883011113204),
 .UNSPECIFIED.)
CURVE()
GEOMETRIC_REPRESENTATION_ITEM()
RATIONAL_B_SPLINE_CURVE((1.00013237845324,1.00016634217771,1.00000799154408))
REPRESENTATION_ITEM('')
);
#999=(
BOUNDED_CURVE()
B_SPLINE_CURVE(2,(#33066,#33067,#33068),.UNSPECIFIED.,.F.,.F.)
B_SPLINE_CURVE_WITH_KNOTS((3,3),(0.000526061815843999,0.0490373321941597),
 .UNSPECIFIED.)
CURVE()
GEOMETRIC_REPRESENTATION_ITEM()
RATIONAL_B_SPLINE_CURVE((1.00000140604825,1.00006598065026,1.00008344962727))
REPRESENTATION_ITEM('')
);
#1000=(
BOUNDED_CURVE()
B_SPLINE_CURVE(2,(#33074,#33075,#33076),.UNSPECIFIED.,.F.,.F.)
B_SPLINE_CURVE_WITH_KNOTS((3,3),(0.085017844734947,0.133529115174433),
 .UNSPECIFIED.)
CURVE()
GEOMETRIC_REPRESENTATION_ITEM()
RATIONAL_B_SPLINE_CURVE((1.00008344962705,1.00006598065013,1.00000140604825))
REPRESENTATION_ITEM('')
);
#1001=(
BOUNDED_CURVE()
B_SPLINE_CURVE(2,(#33097,#33098,#33099),.UNSPECIFIED.,.F.,.F.)
B_SPLINE_CURVE_WITH_KNOTS((3,3),(0.00295018481896423,0.0985937601695785),
 .UNSPECIFIED.)
CURVE()
GEOMETRIC_REPRESENTATION_ITEM()
RATIONAL_B_SPLINE_CURVE((1.00000995626949,1.00016837897465,1.00013448693797))
REPRESENTATION_ITEM('')
);
#1002=(
BOUNDED_CURVE()
B_SPLINE_CURVE(2,(#33102,#33103,#33104),.UNSPECIFIED.,.F.,.F.)
B_SPLINE_CURVE_WITH_KNOTS((3,3),(0.000473184985764736,0.0515065306432933),
 .UNSPECIFIED.)
CURVE()
GEOMETRIC_REPRESENTATION_ITEM()
RATIONAL_B_SPLINE_CURVE((1.00001807280714,1.00098893623083,1.00115754364123))
REPRESENTATION_ITEM('')
);
#1003=(
BOUNDED_CURVE()
B_SPLINE_CURVE(2,(#33109,#33110,#33111),.UNSPECIFIED.,.F.,.F.)
B_SPLINE_CURVE_WITH_KNOTS((3,3),(0.0729556909351823,0.123986559684223),
 .UNSPECIFIED.)
CURVE()
GEOMETRIC_REPRESENTATION_ITEM()
RATIONAL_B_SPLINE_CURVE((1.0011605252602,1.00099293482075,1.00002308400869))
REPRESENTATION_ITEM('')
);
#1004=(
BOUNDED_CURVE()
B_SPLINE_CURVE(2,(#33121,#33122,#33123),.UNSPECIFIED.,.F.,.F.)
B_SPLINE_CURVE_WITH_KNOTS((3,3),(0.0642390630877405,0.159883011113205),
 .UNSPECIFIED.)
CURVE()
GEOMETRIC_REPRESENTATION_ITEM()
RATIONAL_B_SPLINE_CURVE((1.0001323784534,1.00016634217792,1.00000799154409))
REPRESENTATION_ITEM('')
);
#1005=(
BOUNDED_CURVE()
B_SPLINE_CURVE(2,(#33126,#33127,#33128),.UNSPECIFIED.,.F.,.F.)
B_SPLINE_CURVE_WITH_KNOTS((3,3),(0.000526061815841318,0.0490373321941963),
 .UNSPECIFIED.)
CURVE()
GEOMETRIC_REPRESENTATION_ITEM()
RATIONAL_B_SPLINE_CURVE((1.00000140604824,1.00006598064947,1.00008344962627))
REPRESENTATION_ITEM('')
);
#1006=(
BOUNDED_CURVE()
B_SPLINE_CURVE(2,(#33134,#33135,#33136),.UNSPECIFIED.,.F.,.F.)
B_SPLINE_CURVE_WITH_KNOTS((3,3),(0.0850178447349235,0.133529115174428),
 .UNSPECIFIED.)
CURVE()
GEOMETRIC_REPRESENTATION_ITEM()
RATIONAL_B_SPLINE_CURVE((1.00008344962713,1.0000659806502,1.00000140604825))
REPRESENTATION_ITEM('')
);
#1007=(
BOUNDED_CURVE()
B_SPLINE_CURVE(2,(#33157,#33158,#33159),.UNSPECIFIED.,.F.,.F.)
B_SPLINE_CURVE_WITH_KNOTS((3,3),(0.00295018482096791,0.0985937601715863),
 .UNSPECIFIED.)
CURVE()
GEOMETRIC_REPRESENTATION_ITEM()
RATIONAL_B_SPLINE_CURVE((1.00000995626946,1.00016837897397,1.00013448693743))
REPRESENTATION_ITEM('')
);
#1008=(
BOUNDED_CURVE()
B_SPLINE_CURVE(2,(#33162,#33163,#33164),.UNSPECIFIED.,.F.,.F.)
B_SPLINE_CURVE_WITH_KNOTS((3,3),(0.000474651750499241,0.0515079945407172),
 .UNSPECIFIED.)
CURVE()
GEOMETRIC_REPRESENTATION_ITEM()
RATIONAL_B_SPLINE_CURVE((1.0000181290019,1.00098899015283,1.00115759524465))
REPRESENTATION_ITEM('')
);
#1009=(
BOUNDED_CURVE()
B_SPLINE_CURVE(2,(#33169,#33170,#33171),.UNSPECIFIED.,.F.,.F.)
B_SPLINE_CURVE_WITH_KNOTS((3,3),(0.73383872017312,0.777722409416427),
 .UNSPECIFIED.)
CURVE()
GEOMETRIC_REPRESENTATION_ITEM()
RATIONAL_B_SPLINE_CURVE((1.02425882037767,1.01846995640957,1.01190199115935))
REPRESENTATION_ITEM('')
);
#1010=(
BOUNDED_CURVE()
B_SPLINE_CURVE(2,(#33208,#33209,#33210),.UNSPECIFIED.,.F.,.F.)
B_SPLINE_CURVE_WITH_KNOTS((3,3),(0.000478034212987197,0.0489893198676105),
 .UNSPECIFIED.)
CURVE()
GEOMETRIC_REPRESENTATION_ITEM()
RATIONAL_B_SPLINE_CURVE((1.00000127717582,1.00006584948475,1.00008331617371))
REPRESENTATION_ITEM('')
);
#1011=(
BOUNDED_CURVE()
B_SPLINE_CURVE(2,(#33214,#33215,#33216),.UNSPECIFIED.,.F.,.F.)
B_SPLINE_CURVE_WITH_KNOTS((3,3),(0.0849651357209515,0.133476420621903),
 .UNSPECIFIED.)
CURVE()
GEOMETRIC_REPRESENTATION_ITEM()
RATIONAL_B_SPLINE_CURVE((1.00008331617332,1.00006584948388,1.00000127717582))
REPRESENTATION_ITEM('')
);
#1012=(
BOUNDED_CURVE()
B_SPLINE_CURVE(2,(#33225,#33226,#33227),.UNSPECIFIED.,.F.,.F.)
B_SPLINE_CURVE_WITH_KNOTS((3,3),(0.0642390630877396,0.159883011113208),
 .UNSPECIFIED.)
CURVE()
GEOMETRIC_REPRESENTATION_ITEM()
RATIONAL_B_SPLINE_CURVE((1.00013237845388,1.00016634217853,1.00000799154412))
REPRESENTATION_ITEM('')
);
#1013=(
BOUNDED_CURVE()
B_SPLINE_CURVE(2,(#33261,#33262,#33263),.UNSPECIFIED.,.F.,.F.)
B_SPLINE_CURVE_WITH_KNOTS((3,3),(0.0850174365043124,0.13352847207702),
 .UNSPECIFIED.)
CURVE()
GEOMETRIC_REPRESENTATION_ITEM()
RATIONAL_B_SPLINE_CURVE((1.00008336789045,1.00006587559557,1.00000127768044))
REPRESENTATION_ITEM('')
);
#1014=(
BOUNDED_CURVE()
B_SPLINE_CURVE(2,(#33266,#33267,#33268),.UNSPECIFIED.,.F.,.F.)
B_SPLINE_CURVE_WITH_KNOTS((3,3),(0.0029501848107848,0.0985937601613831),
 .UNSPECIFIED.)
CURVE()
GEOMETRIC_REPRESENTATION_ITEM()
RATIONAL_B_SPLINE_CURVE((1.00000995626935,1.00016837897274,1.00013448693644))
REPRESENTATION_ITEM('')
);
#1015=(
BOUNDED_CURVE()
B_SPLINE_CURVE(2,(#33283,#33284,#33285),.UNSPECIFIED.,.F.,.F.)
B_SPLINE_CURVE_WITH_KNOTS((3,3),(0.00295018481829096,0.0985937601689052),
 .UNSPECIFIED.)
CURVE()
GEOMETRIC_REPRESENTATION_ITEM()
RATIONAL_B_SPLINE_CURVE((1.00000995626949,1.00016837897471,1.00013448693802))
REPRESENTATION_ITEM('')
);
#1016=(
BOUNDED_CURVE()
B_SPLINE_CURVE(2,(#33288,#33289,#33290),.UNSPECIFIED.,.F.,.F.)
B_SPLINE_CURVE_WITH_KNOTS((3,3),(0.000474646853444211,0.0515079897376496),
 .UNSPECIFIED.)
CURVE()
GEOMETRIC_REPRESENTATION_ITEM()
RATIONAL_B_SPLINE_CURVE((1.00001812881482,1.00098899000409,1.00115759513441))
REPRESENTATION_ITEM('')
);
#1017=(
BOUNDED_CURVE()
B_SPLINE_CURVE(2,(#33295,#33296,#33297),.UNSPECIFIED.,.F.,.F.)
B_SPLINE_CURVE_WITH_KNOTS((3,3),(0.733838720173112,0.777722409416418),
 .UNSPECIFIED.)
CURVE()
GEOMETRIC_REPRESENTATION_ITEM()
RATIONAL_B_SPLINE_CURVE((1.02425882037767,1.01846995640957,1.01190199115935))
REPRESENTATION_ITEM('')
);
#1018=(
BOUNDED_CURVE()
B_SPLINE_CURVE(2,(#33304,#33305,#33306),.UNSPECIFIED.,.F.,.F.)
B_SPLINE_CURVE_WITH_KNOTS((3,3),(0.000478034212982558,0.0489893198675958),
 .UNSPECIFIED.)
CURVE()
GEOMETRIC_REPRESENTATION_ITEM()
RATIONAL_B_SPLINE_CURVE((1.00000127717582,1.00006584948482,1.0000833161738))
REPRESENTATION_ITEM('')
);
#1019=(
BOUNDED_CURVE()
B_SPLINE_CURVE(2,(#33310,#33311,#33312),.UNSPECIFIED.,.F.,.F.)
B_SPLINE_CURVE_WITH_KNOTS((3,3),(0.084965135720964,0.133476420621902),
 .UNSPECIFIED.)
CURVE()
GEOMETRIC_REPRESENTATION_ITEM()
RATIONAL_B_SPLINE_CURVE((1.00008331617392,1.00006584948435,1.00000127717583))
REPRESENTATION_ITEM('')
);
#1020=(
BOUNDED_CURVE()
B_SPLINE_CURVE(2,(#33321,#33322,#33323),.UNSPECIFIED.,.F.,.F.)
B_SPLINE_CURVE_WITH_KNOTS((3,3),(0.0642390630877467,0.159883011113209),
 .UNSPECIFIED.)
CURVE()
GEOMETRIC_REPRESENTATION_ITEM()
RATIONAL_B_SPLINE_CURVE((1.00013237845391,1.00016634217857,1.00000799154412))
REPRESENTATION_ITEM('')
);
#1021=(
BOUNDED_CURVE()
B_SPLINE_CURVE(2,(#33339,#33340,#33341),.UNSPECIFIED.,.F.,.F.)
B_SPLINE_CURVE_WITH_KNOTS((3,3),(0.00295018480947799,0.0985937601601038),
 .UNSPECIFIED.)
CURVE()
GEOMETRIC_REPRESENTATION_ITEM()
RATIONAL_B_SPLINE_CURVE((1.00000995626944,1.00016837897428,1.00013448693767))
REPRESENTATION_ITEM('')
);
#1022=(
BOUNDED_CURVE()
B_SPLINE_CURVE(2,(#33344,#33345,#33346),.UNSPECIFIED.,.F.,.F.)
B_SPLINE_CURVE_WITH_KNOTS((3,3),(0.000474646853447348,0.0515079897376581),
 .UNSPECIFIED.)
CURVE()
GEOMETRIC_REPRESENTATION_ITEM()
RATIONAL_B_SPLINE_CURVE((1.00001812881482,1.00098899000384,1.00115759513413))
REPRESENTATION_ITEM('')
);
#1023=(
BOUNDED_CURVE()
B_SPLINE_CURVE(2,(#33351,#33352,#33353),.UNSPECIFIED.,.F.,.F.)
B_SPLINE_CURVE_WITH_KNOTS((3,3),(0.733838720173119,0.777722409416428),
 .UNSPECIFIED.)
CURVE()
GEOMETRIC_REPRESENTATION_ITEM()
RATIONAL_B_SPLINE_CURVE((1.02425882037767,1.01846995640957,1.01190199115935))
REPRESENTATION_ITEM('')
);
#1024=(
BOUNDED_CURVE()
B_SPLINE_CURVE(2,(#33360,#33361,#33362),.UNSPECIFIED.,.F.,.F.)
B_SPLINE_CURVE_WITH_KNOTS((3,3),(0.00047803421298473,0.0489893198675923),
 .UNSPECIFIED.)
CURVE()
GEOMETRIC_REPRESENTATION_ITEM()
RATIONAL_B_SPLINE_CURVE((1.00000127717583,1.00006584948522,1.00008331617429))
REPRESENTATION_ITEM('')
);
#1025=(
BOUNDED_CURVE()
B_SPLINE_CURVE(2,(#33366,#33367,#33368),.UNSPECIFIED.,.F.,.F.)
B_SPLINE_CURVE_WITH_KNOTS((3,3),(0.0849651357209518,0.133476420621905),
 .UNSPECIFIED.)
CURVE()
GEOMETRIC_REPRESENTATION_ITEM()
RATIONAL_B_SPLINE_CURVE((1.00008331617313,1.00006584948373,1.00000127717582))
REPRESENTATION_ITEM('')
);
#1026=(
BOUNDED_CURVE()
B_SPLINE_CURVE(2,(#33377,#33378,#33379),.UNSPECIFIED.,.F.,.F.)
B_SPLINE_CURVE_WITH_KNOTS((3,3),(0.0642390630877352,0.15988301111321),
 .UNSPECIFIED.)
CURVE()
GEOMETRIC_REPRESENTATION_ITEM()
RATIONAL_B_SPLINE_CURVE((1.00013237845418,1.0001663421789,1.00000799154414))
REPRESENTATION_ITEM('')
);
#1027=(
BOUNDED_CURVE()
B_SPLINE_CURVE(2,(#33395,#33396,#33397),.UNSPECIFIED.,.F.,.F.)
B_SPLINE_CURVE_WITH_KNOTS((3,3),(0.00295018481006126,0.0985937601607044),
 .UNSPECIFIED.)
CURVE()
GEOMETRIC_REPRESENTATION_ITEM()
RATIONAL_B_SPLINE_CURVE((1.00000995626951,1.00016837897535,1.00013448693852))
REPRESENTATION_ITEM('')
);
#1028=(
BOUNDED_CURVE()
B_SPLINE_CURVE(2,(#33400,#33401,#33402),.UNSPECIFIED.,.F.,.F.)
B_SPLINE_CURVE_WITH_KNOTS((3,3),(0.000474646853442338,0.0515079897376532),
 .UNSPECIFIED.)
CURVE()
GEOMETRIC_REPRESENTATION_ITEM()
RATIONAL_B_SPLINE_CURVE((1.00001812881482,1.00098899000395,1.00115759513426))
REPRESENTATION_ITEM('')
);
#1029=(
BOUNDED_CURVE()
B_SPLINE_CURVE(2,(#33407,#33408,#33409),.UNSPECIFIED.,.F.,.F.)
B_SPLINE_CURVE_WITH_KNOTS((3,3),(0.733838720173123,0.777722409416431),
 .UNSPECIFIED.)
CURVE()
GEOMETRIC_REPRESENTATION_ITEM()
RATIONAL_B_SPLINE_CURVE((1.02425882037767,1.01846995640957,1.01190199115935))
REPRESENTATION_ITEM('')
);
#1030=(
BOUNDED_CURVE()
B_SPLINE_CURVE(2,(#33416,#33417,#33418),.UNSPECIFIED.,.F.,.F.)
B_SPLINE_CURVE_WITH_KNOTS((3,3),(0.000478034212989242,0.0489893198676443),
 .UNSPECIFIED.)
CURVE()
GEOMETRIC_REPRESENTATION_ITEM()
RATIONAL_B_SPLINE_CURVE((1.0000012771758,1.00006584948372,1.0000833161724))
REPRESENTATION_ITEM('')
);
#1031=(
BOUNDED_CURVE()
B_SPLINE_CURVE(2,(#33422,#33423,#33424),.UNSPECIFIED.,.F.,.F.)
B_SPLINE_CURVE_WITH_KNOTS((3,3),(0.0849651357209273,0.133476420621905),
 .UNSPECIFIED.)
CURVE()
GEOMETRIC_REPRESENTATION_ITEM()
RATIONAL_B_SPLINE_CURVE((1.00008331617315,1.00006584948374,1.00000127717582))
REPRESENTATION_ITEM('')
);
#1032=(
BOUNDED_CURVE()
B_SPLINE_CURVE(2,(#33433,#33434,#33435),.UNSPECIFIED.,.F.,.F.)
B_SPLINE_CURVE_WITH_KNOTS((3,3),(0.0642390630877532,0.159883011113204),
 .UNSPECIFIED.)
CURVE()
GEOMETRIC_REPRESENTATION_ITEM()
RATIONAL_B_SPLINE_CURVE((1.00013237845329,1.00016634217778,1.00000799154408))
REPRESENTATION_ITEM('')
);
#1033=(
BOUNDED_CURVE()
B_SPLINE_CURVE(2,(#33451,#33452,#33453),.UNSPECIFIED.,.F.,.F.)
B_SPLINE_CURVE_WITH_KNOTS((3,3),(0.00295018481501485,0.0985937601656302),
 .UNSPECIFIED.)
CURVE()
GEOMETRIC_REPRESENTATION_ITEM()
RATIONAL_B_SPLINE_CURVE((1.00000995626945,1.0001683789741,1.00013448693753))
REPRESENTATION_ITEM('')
);
#1034=(
BOUNDED_CURVE()
B_SPLINE_CURVE(2,(#33456,#33457,#33458),.UNSPECIFIED.,.F.,.F.)
B_SPLINE_CURVE_WITH_KNOTS((3,3),(0.000474646853444173,0.0515079897376518),
 .UNSPECIFIED.)
CURVE()
GEOMETRIC_REPRESENTATION_ITEM()
RATIONAL_B_SPLINE_CURVE((1.00001812881482,1.00098899000411,1.00115759513444))
REPRESENTATION_ITEM('')
);
#1035=(
BOUNDED_CURVE()
B_SPLINE_CURVE(2,(#33463,#33464,#33465),.UNSPECIFIED.,.F.,.F.)
B_SPLINE_CURVE_WITH_KNOTS((3,3),(0.733838720173153,0.777722409416459),
 .UNSPECIFIED.)
CURVE()
GEOMETRIC_REPRESENTATION_ITEM()
RATIONAL_B_SPLINE_CURVE((1.02425882037767,1.01846995640957,1.01190199115935))
REPRESENTATION_ITEM('')
);
#1036=(
BOUNDED_CURVE()
B_SPLINE_CURVE(2,(#33472,#33473,#33474),.UNSPECIFIED.,.F.,.F.)
B_SPLINE_CURVE_WITH_KNOTS((3,3),(0.000478034212985405,0.0489893198675976),
 .UNSPECIFIED.)
CURVE()
GEOMETRIC_REPRESENTATION_ITEM()
RATIONAL_B_SPLINE_CURVE((1.00000127717583,1.00006584948535,1.00008331617446))
REPRESENTATION_ITEM('')
);
#1037=(
BOUNDED_CURVE()
B_SPLINE_CURVE(2,(#33478,#33479,#33480),.UNSPECIFIED.,.F.,.F.)
B_SPLINE_CURVE_WITH_KNOTS((3,3),(0.0849651357209773,0.133476420621906),
 .UNSPECIFIED.)
CURVE()
GEOMETRIC_REPRESENTATION_ITEM()
RATIONAL_B_SPLINE_CURVE((1.00008331617476,1.00006584948501,1.00000127717584))
REPRESENTATION_ITEM('')
);
#1038=(
BOUNDED_CURVE()
B_SPLINE_CURVE(2,(#33489,#33490,#33491),.UNSPECIFIED.,.F.,.F.)
B_SPLINE_CURVE_WITH_KNOTS((3,3),(0.0642390630877643,0.159883011113209),
 .UNSPECIFIED.)
CURVE()
GEOMETRIC_REPRESENTATION_ITEM()
RATIONAL_B_SPLINE_CURVE((1.00013237845267,1.000166342177,1.00000799154405))
REPRESENTATION_ITEM('')
);
#1039=(
BOUNDED_CURVE()
B_SPLINE_CURVE(2,(#33507,#33508,#33509),.UNSPECIFIED.,.F.,.F.)
B_SPLINE_CURVE_WITH_KNOTS((3,3),(0.00295018481095983,0.0985937601615901),
 .UNSPECIFIED.)
CURVE()
GEOMETRIC_REPRESENTATION_ITEM()
RATIONAL_B_SPLINE_CURVE((1.00000995626948,1.00016837897492,1.00013448693818))
REPRESENTATION_ITEM('')
);
#1040=(
BOUNDED_CURVE()
B_SPLINE_CURVE(2,(#33512,#33513,#33514),.UNSPECIFIED.,.F.,.F.)
B_SPLINE_CURVE_WITH_KNOTS((3,3),(0.000474646853443493,0.0515079897376577),
 .UNSPECIFIED.)
CURVE()
GEOMETRIC_REPRESENTATION_ITEM()
RATIONAL_B_SPLINE_CURVE((1.00001812881482,1.00098899000373,1.00115759513399))
REPRESENTATION_ITEM('')
);
#1041=(
BOUNDED_CURVE()
B_SPLINE_CURVE(2,(#33519,#33520,#33521),.UNSPECIFIED.,.F.,.F.)
B_SPLINE_CURVE_WITH_KNOTS((3,3),(0.733838720173112,0.77772240941642),
 .UNSPECIFIED.)
CURVE()
GEOMETRIC_REPRESENTATION_ITEM()
RATIONAL_B_SPLINE_CURVE((1.02425882037767,1.01846995640957,1.01190199115935))
REPRESENTATION_ITEM('')
);
#1042=(
BOUNDED_CURVE()
B_SPLINE_CURVE(2,(#33528,#33529,#33530),.UNSPECIFIED.,.F.,.F.)
B_SPLINE_CURVE_WITH_KNOTS((3,3),(0.000478034212986085,0.0489893198676214),
 .UNSPECIFIED.)
CURVE()
GEOMETRIC_REPRESENTATION_ITEM()
RATIONAL_B_SPLINE_CURVE((1.00000127717582,1.00006584948496,1.00008331617397))
REPRESENTATION_ITEM('')
);
#1043=(
BOUNDED_CURVE()
B_SPLINE_CURVE(2,(#33534,#33535,#33536),.UNSPECIFIED.,.F.,.F.)
B_SPLINE_CURVE_WITH_KNOTS((3,3),(0.0849651357209684,0.133476420621907),
 .UNSPECIFIED.)
CURVE()
GEOMETRIC_REPRESENTATION_ITEM()
RATIONAL_B_SPLINE_CURVE((1.00008331617452,1.00006584948482,1.00000127717584))
REPRESENTATION_ITEM('')
);
#1044=(
BOUNDED_CURVE()
B_SPLINE_CURVE(2,(#33545,#33546,#33547),.UNSPECIFIED.,.F.,.F.)
B_SPLINE_CURVE_WITH_KNOTS((3,3),(0.0642390630877575,0.159883011113204),
 .UNSPECIFIED.)
CURVE()
GEOMETRIC_REPRESENTATION_ITEM()
RATIONAL_B_SPLINE_CURVE((1.00013237845349,1.00016634217804,1.0000079915441))
REPRESENTATION_ITEM('')
);
#1045=(
BOUNDED_CURVE()
B_SPLINE_CURVE(2,(#33569,#33570,#33571),.UNSPECIFIED.,.F.,.F.)
B_SPLINE_CURVE_WITH_KNOTS((3,3),(0.000478034212987892,0.0489893198676202),
 .UNSPECIFIED.)
CURVE()
GEOMETRIC_REPRESENTATION_ITEM()
RATIONAL_B_SPLINE_CURVE((1.00000127717582,1.00006584948477,1.00008331617373))
REPRESENTATION_ITEM('')
);
#1046=(
BOUNDED_CURVE()
B_SPLINE_CURVE(2,(#33586,#33587,#33588),.UNSPECIFIED.,.F.,.F.)
B_SPLINE_CURVE_WITH_KNOTS((3,3),(0.002950184815266,0.0985937601658534),
 .UNSPECIFIED.)
CURVE()
GEOMETRIC_REPRESENTATION_ITEM()
RATIONAL_B_SPLINE_CURVE((1.00000995626939,1.00016837897316,1.00013448693678))
REPRESENTATION_ITEM('')
);
#1047=(
BOUNDED_CURVE()
B_SPLINE_CURVE(2,(#33591,#33592,#33593),.UNSPECIFIED.,.F.,.F.)
B_SPLINE_CURVE_WITH_KNOTS((3,3),(0.000474646853442315,0.051507989737653),
 .UNSPECIFIED.)
CURVE()
GEOMETRIC_REPRESENTATION_ITEM()
RATIONAL_B_SPLINE_CURVE((1.00001812881482,1.00098899000397,1.00115759513428))
REPRESENTATION_ITEM('')
);
#1048=(
BOUNDED_CURVE()
B_SPLINE_CURVE(2,(#33597,#33598,#33599),.UNSPECIFIED.,.F.,.F.)
B_SPLINE_CURVE_WITH_KNOTS((3,3),(0.733838720173123,0.777722409416431),
 .UNSPECIFIED.)
CURVE()
GEOMETRIC_REPRESENTATION_ITEM()
RATIONAL_B_SPLINE_CURVE((1.02425882037767,1.01846995640957,1.01190199115935))
REPRESENTATION_ITEM('')
);
#1049=(
BOUNDED_CURVE()
B_SPLINE_CURVE(2,(#33603,#33604,#33605),.UNSPECIFIED.,.F.,.F.)
B_SPLINE_CURVE_WITH_KNOTS((3,3),(0.0642390630877507,0.159883011113205),
 .UNSPECIFIED.)
CURVE()
GEOMETRIC_REPRESENTATION_ITEM()
RATIONAL_B_SPLINE_CURVE((1.00013237845344,1.00016634217798,1.00000799154409))
REPRESENTATION_ITEM('')
);
#1050=(
BOUNDED_CURVE()
B_SPLINE_CURVE(2,(#43966,#43967,#43968),.UNSPECIFIED.,.F.,.F.)
B_SPLINE_CURVE_WITH_KNOTS((3,3),(0.,0.00144737940428136),.UNSPECIFIED.)
CURVE()
GEOMETRIC_REPRESENTATION_ITEM()
RATIONAL_B_SPLINE_CURVE((1.,1.00001544417762,1.00003081080475))
REPRESENTATION_ITEM('')
);
#1051=(
BOUNDED_CURVE()
B_SPLINE_CURVE(2,(#43981,#43982,#43983),.UNSPECIFIED.,.F.,.F.)
B_SPLINE_CURVE_WITH_KNOTS((3,3),(0.575043800428103,0.576491179832384),
 .UNSPECIFIED.)
CURVE()
GEOMETRIC_REPRESENTATION_ITEM()
RATIONAL_B_SPLINE_CURVE((1.00003081080475,1.00001544417762,1.))
REPRESENTATION_ITEM('')
);
#1052=(
BOUNDED_CURVE()
B_SPLINE_CURVE(2,(#43997,#43998,#43999),.UNSPECIFIED.,.F.,.F.)
B_SPLINE_CURVE_WITH_KNOTS((3,3),(0.575043800428102,0.576491179832384),
 .UNSPECIFIED.)
CURVE()
GEOMETRIC_REPRESENTATION_ITEM()
RATIONAL_B_SPLINE_CURVE((1.00003081080475,1.00001544417762,1.))
REPRESENTATION_ITEM('')
);
#1053=(
BOUNDED_CURVE()
B_SPLINE_CURVE(2,(#44003,#44004,#44005),.UNSPECIFIED.,.F.,.F.)
B_SPLINE_CURVE_WITH_KNOTS((3,3),(0.,0.00144737940428207),.UNSPECIFIED.)
CURVE()
GEOMETRIC_REPRESENTATION_ITEM()
RATIONAL_B_SPLINE_CURVE((1.,1.00001544417762,1.00003081080475))
REPRESENTATION_ITEM('')
);
#1054=(
BOUNDED_CURVE()
B_SPLINE_CURVE(5,(#47338,#47339,#47340,#47341,#47342,#47343,#47344,#47345,
#47346,#47347,#47348,#47349,#47350,#47351,#47352,#47353,#47354),
 .UNSPECIFIED.,.F.,.F.)
B_SPLINE_CURVE_WITH_KNOTS((6,1,1,1,1,1,1,1,1,1,1,1,6),(0.422875935222759,
0.44,0.48,0.52,0.56,0.6,0.64,0.68,0.72,0.76,0.8,0.84,0.867889296212967),
 .UNSPECIFIED.)
CURVE()
GEOMETRIC_REPRESENTATION_ITEM()
RATIONAL_B_SPLINE_CURVE((1.,1.,1.,1.,1.,1.,1.,1.,1.,1.,1.,1.,1.,1.,1.,1.,
1.))
REPRESENTATION_ITEM('')
);
#1055=(
BOUNDED_CURVE()
B_SPLINE_CURVE(5,(#56525,#56526,#56527,#56528,#56529,#56530,#56531,#56532),
 .UNSPECIFIED.,.F.,.F.)
B_SPLINE_CURVE_WITH_KNOTS((6,1,1,6),(0.904281576377558,0.92,0.96,1.),
 .UNSPECIFIED.)
CURVE()
GEOMETRIC_REPRESENTATION_ITEM()
RATIONAL_B_SPLINE_CURVE((1.,1.,1.,1.,1.,1.,1.,1.))
REPRESENTATION_ITEM('')
);
#1056=(
BOUNDED_CURVE()
B_SPLINE_CURVE(2,(#57584,#57585,#57586),.UNSPECIFIED.,.F.,.F.)
B_SPLINE_CURVE_WITH_KNOTS((3,3),(0.111972083330786,0.162414552121297),
 .UNSPECIFIED.)
CURVE()
GEOMETRIC_REPRESENTATION_ITEM()
RATIONAL_B_SPLINE_CURVE((1.01528943481759,1.01635902992211,1.01528943481759))
REPRESENTATION_ITEM('')
);
#1057=(
BOUNDED_CURVE()
B_SPLINE_CURVE(2,(#57594,#57595,#57596),.UNSPECIFIED.,.F.,.F.)
B_SPLINE_CURVE_WITH_KNOTS((3,3),(0.09935665845201,0.231695159015479),
 .UNSPECIFIED.)
CURVE()
GEOMETRIC_REPRESENTATION_ITEM()
RATIONAL_B_SPLINE_CURVE((1.02178152598816,1.03072985007612,1.02487304850091))
REPRESENTATION_ITEM('')
);
#1058=(
BOUNDED_CURVE()
B_SPLINE_CURVE(2,(#57598,#57599,#57600),.UNSPECIFIED.,.F.,.F.)
B_SPLINE_CURVE_WITH_KNOTS((3,3),(0.154087551415272,0.195687290922671),
 .UNSPECIFIED.)
CURVE()
GEOMETRIC_REPRESENTATION_ITEM()
RATIONAL_B_SPLINE_CURVE((1.01731872616523,1.01669262938109,1.01446617353995))
REPRESENTATION_ITEM('')
);
#1059=(
BOUNDED_CURVE()
B_SPLINE_CURVE(2,(#57613,#57614,#57615),.UNSPECIFIED.,.F.,.F.)
B_SPLINE_CURVE_WITH_KNOTS((3,3),(0.126990834822139,0.259329335387418),
 .UNSPECIFIED.)
CURVE()
GEOMETRIC_REPRESENTATION_ITEM()
RATIONAL_B_SPLINE_CURVE((1.02487304850069,1.03072985007626,1.02178152598826))
REPRESENTATION_ITEM('')
);
#1060=(
BOUNDED_CURVE()
B_SPLINE_CURVE(2,(#57617,#57618,#57619),.UNSPECIFIED.,.F.,.F.)
B_SPLINE_CURVE_WITH_KNOTS((3,3),(0.09935665845201,0.23169515901548),
 .UNSPECIFIED.)
CURVE()
GEOMETRIC_REPRESENTATION_ITEM()
RATIONAL_B_SPLINE_CURVE((1.02178152598816,1.03072985007612,1.02487304850091))
REPRESENTATION_ITEM('')
);
#1061=(
BOUNDED_CURVE()
B_SPLINE_CURVE(2,(#57621,#57622,#57623),.UNSPECIFIED.,.F.,.F.)
B_SPLINE_CURVE_WITH_KNOTS((3,3),(0.111972083330787,0.162414552121298),
 .UNSPECIFIED.)
CURVE()
GEOMETRIC_REPRESENTATION_ITEM()
RATIONAL_B_SPLINE_CURVE((1.01528943481758,1.01635902992211,1.01528943481758))
REPRESENTATION_ITEM('')
);
#1062=(
BOUNDED_CURVE()
B_SPLINE_CURVE(2,(#57625,#57626,#57627),.UNSPECIFIED.,.F.,.F.)
B_SPLINE_CURVE_WITH_KNOTS((3,3),(0.126990834822138,0.259329335387416),
 .UNSPECIFIED.)
CURVE()
GEOMETRIC_REPRESENTATION_ITEM()
RATIONAL_B_SPLINE_CURVE((1.02487304850069,1.03072985007626,1.02178152598826))
REPRESENTATION_ITEM('')
);
#1063=(
BOUNDED_CURVE()
B_SPLINE_CURVE(2,(#57629,#57630,#57631),.UNSPECIFIED.,.F.,.F.)
B_SPLINE_CURVE_WITH_KNOTS((3,3),(0.0799382874584893,0.121538026965825),
 .UNSPECIFIED.)
CURVE()
GEOMETRIC_REPRESENTATION_ITEM()
RATIONAL_B_SPLINE_CURVE((1.01446617353996,1.0166926293811,1.01731872616524))
REPRESENTATION_ITEM('')
);
#1064=(
BOUNDED_SURFACE()
B_SPLINE_SURFACE(5,2,((#24386,#24387,#24388,#24389,#24390,#24391,#24392,
#24393,#24394),(#24395,#24396,#24397,#24398,#24399,#24400,#24401,#24402,
#24403),(#24404,#24405,#24406,#24407,#24408,#24409,#24410,#24411,#24412),
(#24413,#24414,#24415,#24416,#24417,#24418,#24419,#24420,#24421),(#24422,
#24423,#24424,#24425,#24426,#24427,#24428,#24429,#24430),(#24431,#24432,
#24433,#24434,#24435,#24436,#24437,#24438,#24439),(#24440,#24441,#24442,
#24443,#24444,#24445,#24446,#24447,#24448),(#24449,#24450,#24451,#24452,
#24453,#24454,#24455,#24456,#24457),(#24458,#24459,#24460,#24461,#24462,
#24463,#24464,#24465,#24466),(#24467,#24468,#24469,#24470,#24471,#24472,
#24473,#24474,#24475),(#24476,#24477,#24478,#24479,#24480,#24481,#24482,
#24483,#24484),(#24485,#24486,#24487,#24488,#24489,#24490,#24491,#24492,
#24493),(#24494,#24495,#24496,#24497,#24498,#24499,#24500,#24501,#24502),
(#24503,#24504,#24505,#24506,#24507,#24508,#24509,#24510,#24511),(#24512,
#24513,#24514,#24515,#24516,#24517,#24518,#24519,#24520),(#24521,#24522,
#24523,#24524,#24525,#24526,#24527,#24528,#24529),(#24530,#24531,#24532,
#24533,#24534,#24535,#24536,#24537,#24538),(#24539,#24540,#24541,#24542,
#24543,#24544,#24545,#24546,#24547),(#24548,#24549,#24550,#24551,#24552,
#24553,#24554,#24555,#24556),(#24557,#24558,#24559,#24560,#24561,#24562,
#24563,#24564,#24565),(#24566,#24567,#24568,#24569,#24570,#24571,#24572,
#24573,#24574),(#24575,#24576,#24577,#24578,#24579,#24580,#24581,#24582,
#24583),(#24584,#24585,#24586,#24587,#24588,#24589,#24590,#24591,#24592),
(#24593,#24594,#24595,#24596,#24597,#24598,#24599,#24600,#24601),(#24602,
#24603,#24604,#24605,#24606,#24607,#24608,#24609,#24610),(#24611,#24612,
#24613,#24614,#24615,#24616,#24617,#24618,#24619),(#24620,#24621,#24622,
#24623,#24624,#24625,#24626,#24627,#24628),(#24629,#24630,#24631,#24632,
#24633,#24634,#24635,#24636,#24637),(#24638,#24639,#24640,#24641,#24642,
#24643,#24644,#24645,#24646),(#24647,#24648,#24649,#24650,#24651,#24652,
#24653,#24654,#24655)),.UNSPECIFIED.,.F.,.T.,.F.)
B_SPLINE_SURFACE_WITH_KNOTS((6,1,1,1,1,1,1,1,1,1,1,1,1,1,1,1,1,1,1,1,1,
1,1,1,1,6),(3,2,2,2,3),(-1.,-0.96,-0.92,-0.88,-0.84,-0.8,-0.76,-0.72,-0.68,
-0.64,-0.6,-0.56,-0.52,-0.48,-0.44,-0.4,-0.36,-0.32,-0.28,-0.24,-0.2,-0.16,
-0.12,-0.08,-0.04,0.),(0.,1.5707963267949,3.14159265358979,4.71238898038469,
6.28318530717959),.UNSPECIFIED.)
GEOMETRIC_REPRESENTATION_ITEM()
RATIONAL_B_SPLINE_SURFACE(((1.,0.707106781186548,1.,0.707106781186548,1.,
0.707106781186548,1.,0.707106781186548,1.),(1.,0.707106781186548,1.,0.707106781186548,
1.,0.707106781186548,1.,0.707106781186548,1.),(1.,0.707106781186548,1.,
0.707106781186548,1.,0.707106781186548,1.,0.707106781186548,1.),(1.,0.707106781186548,
1.,0.707106781186548,1.,0.707106781186548,1.,0.707106781186548,1.),(1.,
0.707106781186548,1.,0.707106781186548,1.,0.707106781186548,1.,0.707106781186548,
1.),(1.,0.707106781186548,1.,0.707106781186548,1.,0.707106781186548,1.,
0.707106781186548,1.),(1.,0.707106781186548,1.,0.707106781186548,1.,0.707106781186548,
1.,0.707106781186548,1.),(1.,0.707106781186548,1.,0.707106781186548,1.,
0.707106781186548,1.,0.707106781186548,1.),(1.,0.707106781186548,1.,0.707106781186548,
1.,0.707106781186548,1.,0.707106781186548,1.),(1.,0.707106781186548,1.,
0.707106781186548,1.,0.707106781186548,1.,0.707106781186548,1.),(1.,0.707106781186548,
1.,0.707106781186548,1.,0.707106781186548,1.,0.707106781186548,1.),(1.,
0.707106781186548,1.,0.707106781186548,1.,0.707106781186548,1.,0.707106781186548,
1.),(1.,0.707106781186548,1.,0.707106781186548,1.,0.707106781186548,1.,
0.707106781186548,1.),(1.,0.707106781186548,1.,0.707106781186548,1.,0.707106781186548,
1.,0.707106781186548,1.),(1.,0.707106781186548,1.,0.707106781186548,1.,
0.707106781186548,1.,0.707106781186548,1.),(1.,0.707106781186548,1.,0.707106781186548,
1.,0.707106781186548,1.,0.707106781186548,1.),(1.,0.707106781186548,1.,
0.707106781186548,1.,0.707106781186548,1.,0.707106781186548,1.),(1.,0.707106781186548,
1.,0.707106781186548,1.,0.707106781186548,1.,0.707106781186548,1.),(1.,
0.707106781186548,1.,0.707106781186548,1.,0.707106781186548,1.,0.707106781186548,
1.),(1.,0.707106781186548,1.,0.707106781186548,1.,0.707106781186548,1.,
0.707106781186548,1.),(1.,0.707106781186548,1.,0.707106781186548,1.,0.707106781186548,
1.,0.707106781186548,1.),(1.,0.707106781186548,1.,0.707106781186548,1.,
0.707106781186548,1.,0.707106781186548,1.),(1.,0.707106781186548,1.,0.707106781186548,
1.,0.707106781186548,1.,0.707106781186548,1.),(1.,0.707106781186548,1.,
0.707106781186548,1.,0.707106781186548,1.,0.707106781186548,1.),(1.,0.707106781186548,
1.,0.707106781186548,1.,0.707106781186548,1.,0.707106781186548,1.),(1.,
0.707106781186548,1.,0.707106781186548,1.,0.707106781186548,1.,0.707106781186548,
1.),(1.,0.707106781186548,1.,0.707106781186548,1.,0.707106781186548,1.,
0.707106781186548,1.),(1.,0.707106781186548,1.,0.707106781186548,1.,0.707106781186548,
1.,0.707106781186548,1.),(1.,0.707106781186548,1.,0.707106781186548,1.,
0.707106781186548,1.,0.707106781186548,1.),(1.,0.707106781186548,1.,0.707106781186548,
1.,0.707106781186548,1.,0.707106781186548,1.)))
REPRESENTATION_ITEM('')
SURFACE()
);
#1065=(
BOUNDED_SURFACE()
B_SPLINE_SURFACE(5,2,((#34945,#34946,#34947,#34948,#34949,#34950,#34951,
#34952,#34953),(#34954,#34955,#34956,#34957,#34958,#34959,#34960,#34961,
#34962),(#34963,#34964,#34965,#34966,#34967,#34968,#34969,#34970,#34971),
(#34972,#34973,#34974,#34975,#34976,#34977,#34978,#34979,#34980),(#34981,
#34982,#34983,#34984,#34985,#34986,#34987,#34988,#34989),(#34990,#34991,
#34992,#34993,#34994,#34995,#34996,#34997,#34998),(#34999,#35000,#35001,
#35002,#35003,#35004,#35005,#35006,#35007),(#35008,#35009,#35010,#35011,
#35012,#35013,#35014,#35015,#35016),(#35017,#35018,#35019,#35020,#35021,
#35022,#35023,#35024,#35025),(#35026,#35027,#35028,#35029,#35030,#35031,
#35032,#35033,#35034),(#35035,#35036,#35037,#35038,#35039,#35040,#35041,
#35042,#35043),(#35044,#35045,#35046,#35047,#35048,#35049,#35050,#35051,
#35052),(#35053,#35054,#35055,#35056,#35057,#35058,#35059,#35060,#35061),
(#35062,#35063,#35064,#35065,#35066,#35067,#35068,#35069,#35070),(#35071,
#35072,#35073,#35074,#35075,#35076,#35077,#35078,#35079),(#35080,#35081,
#35082,#35083,#35084,#35085,#35086,#35087,#35088),(#35089,#35090,#35091,
#35092,#35093,#35094,#35095,#35096,#35097),(#35098,#35099,#35100,#35101,
#35102,#35103,#35104,#35105,#35106),(#35107,#35108,#35109,#35110,#35111,
#35112,#35113,#35114,#35115),(#35116,#35117,#35118,#35119,#35120,#35121,
#35122,#35123,#35124),(#35125,#35126,#35127,#35128,#35129,#35130,#35131,
#35132,#35133),(#35134,#35135,#35136,#35137,#35138,#35139,#35140,#35141,
#35142),(#35143,#35144,#35145,#35146,#35147,#35148,#35149,#35150,#35151),
(#35152,#35153,#35154,#35155,#35156,#35157,#35158,#35159,#35160),(#35161,
#35162,#35163,#35164,#35165,#35166,#35167,#35168,#35169),(#35170,#35171,
#35172,#35173,#35174,#35175,#35176,#35177,#35178),(#35179,#35180,#35181,
#35182,#35183,#35184,#35185,#35186,#35187),(#35188,#35189,#35190,#35191,
#35192,#35193,#35194,#35195,#35196),(#35197,#35198,#35199,#35200,#35201,
#35202,#35203,#35204,#35205),(#35206,#35207,#35208,#35209,#35210,#35211,
#35212,#35213,#35214)),.UNSPECIFIED.,.F.,.T.,.F.)
B_SPLINE_SURFACE_WITH_KNOTS((6,1,1,1,1,1,1,1,1,1,1,1,1,1,1,1,1,1,1,1,1,
1,1,1,1,6),(3,2,2,2,3),(-1.,-0.96,-0.92,-0.88,-0.84,-0.8,-0.76,-0.72,-0.68,
-0.64,-0.6,-0.56,-0.52,-0.48,-0.44,-0.4,-0.36,-0.32,-0.28,-0.24,-0.2,-0.16,
-0.12,-0.08,-0.04,0.),(0.,1.5707963267949,3.14159265358979,4.71238898038469,
6.28318530717959),.UNSPECIFIED.)
GEOMETRIC_REPRESENTATION_ITEM()
RATIONAL_B_SPLINE_SURFACE(((1.,0.707106781186548,1.,0.707106781186548,1.,
0.707106781186548,1.,0.707106781186548,1.),(1.,0.707106781186548,1.,0.707106781186548,
1.,0.707106781186548,1.,0.707106781186548,1.),(1.,0.707106781186548,1.,
0.707106781186548,1.,0.707106781186548,1.,0.707106781186548,1.),(1.,0.707106781186548,
1.,0.707106781186548,1.,0.707106781186548,1.,0.707106781186548,1.),(1.,
0.707106781186548,1.,0.707106781186548,1.,0.707106781186548,1.,0.707106781186548,
1.),(1.,0.707106781186548,1.,0.707106781186548,1.,0.707106781186548,1.,
0.707106781186548,1.),(1.,0.707106781186548,1.,0.707106781186548,1.,0.707106781186548,
1.,0.707106781186548,1.),(1.,0.707106781186548,1.,0.707106781186548,1.,
0.707106781186548,1.,0.707106781186548,1.),(1.,0.707106781186548,1.,0.707106781186548,
1.,0.707106781186548,1.,0.707106781186548,1.),(1.,0.707106781186548,1.,
0.707106781186548,1.,0.707106781186548,1.,0.707106781186548,1.),(1.,0.707106781186548,
1.,0.707106781186548,1.,0.707106781186548,1.,0.707106781186548,1.),(1.,
0.707106781186548,1.,0.707106781186548,1.,0.707106781186548,1.,0.707106781186548,
1.),(1.,0.707106781186548,1.,0.707106781186548,1.,0.707106781186548,1.,
0.707106781186548,1.),(1.,0.707106781186548,1.,0.707106781186548,1.,0.707106781186548,
1.,0.707106781186548,1.),(1.,0.707106781186548,1.,0.707106781186548,1.,
0.707106781186548,1.,0.707106781186548,1.),(1.,0.707106781186548,1.,0.707106781186548,
1.,0.707106781186548,1.,0.707106781186548,1.),(1.,0.707106781186548,1.,
0.707106781186548,1.,0.707106781186548,1.,0.707106781186548,1.),(1.,0.707106781186548,
1.,0.707106781186548,1.,0.707106781186548,1.,0.707106781186548,1.),(1.,
0.707106781186548,1.,0.707106781186548,1.,0.707106781186548,1.,0.707106781186548,
1.),(1.,0.707106781186548,1.,0.707106781186548,1.,0.707106781186548,1.,
0.707106781186548,1.),(1.,0.707106781186548,1.,0.707106781186548,1.,0.707106781186548,
1.,0.707106781186548,1.),(1.,0.707106781186548,1.,0.707106781186548,1.,
0.707106781186548,1.,0.707106781186548,1.),(1.,0.707106781186548,1.,0.707106781186548,
1.,0.707106781186548,1.,0.707106781186548,1.),(1.,0.707106781186548,1.,
0.707106781186548,1.,0.707106781186548,1.,0.707106781186548,1.),(1.,0.707106781186548,
1.,0.707106781186548,1.,0.707106781186548,1.,0.707106781186548,1.),(1.,
0.707106781186548,1.,0.707106781186548,1.,0.707106781186548,1.,0.707106781186548,
1.),(1.,0.707106781186548,1.,0.707106781186548,1.,0.707106781186548,1.,
0.707106781186548,1.),(1.,0.707106781186548,1.,0.707106781186548,1.,0.707106781186548,
1.,0.707106781186548,1.),(1.,0.707106781186548,1.,0.707106781186548,1.,
0.707106781186548,1.,0.707106781186548,1.),(1.,0.707106781186548,1.,0.707106781186548,
1.,0.707106781186548,1.,0.707106781186548,1.)))
REPRESENTATION_ITEM('')
SURFACE()
);
#1066=(
BOUNDED_SURFACE()
B_SPLINE_SURFACE(5,2,((#35519,#35520,#35521,#35522,#35523,#35524,#35525,
#35526,#35527,#35528,#35529),(#35530,#35531,#35532,#35533,#35534,#35535,
#35536,#35537,#35538,#35539,#35540),(#35541,#35542,#35543,#35544,#35545,
#35546,#35547,#35548,#35549,#35550,#35551),(#35552,#35553,#35554,#35555,
#35556,#35557,#35558,#35559,#35560,#35561,#35562),(#35563,#35564,#35565,
#35566,#35567,#35568,#35569,#35570,#35571,#35572,#35573),(#35574,#35575,
#35576,#35577,#35578,#35579,#35580,#35581,#35582,#35583,#35584),(#35585,
#35586,#35587,#35588,#35589,#35590,#35591,#35592,#35593,#35594,#35595),
(#35596,#35597,#35598,#35599,#35600,#35601,#35602,#35603,#35604,#35605,
#35606),(#35607,#35608,#35609,#35610,#35611,#35612,#35613,#35614,#35615,
#35616,#35617),(#35618,#35619,#35620,#35621,#35622,#35623,#35624,#35625,
#35626,#35627,#35628),(#35629,#35630,#35631,#35632,#35633,#35634,#35635,
#35636,#35637,#35638,#35639),(#35640,#35641,#35642,#35643,#35644,#35645,
#35646,#35647,#35648,#35649,#35650),(#35651,#35652,#35653,#35654,#35655,
#35656,#35657,#35658,#35659,#35660,#35661),(#35662,#35663,#35664,#35665,
#35666,#35667,#35668,#35669,#35670,#35671,#35672),(#35673,#35674,#35675,
#35676,#35677,#35678,#35679,#35680,#35681,#35682,#35683),(#35684,#35685,
#35686,#35687,#35688,#35689,#35690,#35691,#35692,#35693,#35694),(#35695,
#35696,#35697,#35698,#35699,#35700,#35701,#35702,#35703,#35704,#35705),
(#35706,#35707,#35708,#35709,#35710,#35711,#35712,#35713,#35714,#35715,
#35716),(#35717,#35718,#35719,#35720,#35721,#35722,#35723,#35724,#35725,
#35726,#35727),(#35728,#35729,#35730,#35731,#35732,#35733,#35734,#35735,
#35736,#35737,#35738),(#35739,#35740,#35741,#35742,#35743,#35744,#35745,
#35746,#35747,#35748,#35749),(#35750,#35751,#35752,#35753,#35754,#35755,
#35756,#35757,#35758,#35759,#35760),(#35761,#35762,#35763,#35764,#35765,
#35766,#35767,#35768,#35769,#35770,#35771),(#35772,#35773,#35774,#35775,
#35776,#35777,#35778,#35779,#35780,#35781,#35782),(#35783,#35784,#35785,
#35786,#35787,#35788,#35789,#35790,#35791,#35792,#35793)),.UNSPECIFIED.,
 .F.,.T.,.F.)
B_SPLINE_SURFACE_WITH_KNOTS((6,1,1,1,1,1,1,1,1,1,1,1,1,1,1,1,1,1,1,1,6),
(3,2,2,2,2,3),(-1.,-0.95,-0.9,-0.85,-0.8,-0.75,-0.7,-0.65,-0.6,-0.55,-0.5,
-0.45,-0.4,-0.35,-0.3,-0.25,-0.2,-0.15,-0.1,-0.05,0.),(-0.0491117278067552,
0.,1.5707963267949,3.14159265358979,4.71238898038469,6.23407357937283),
 .UNSPECIFIED.)
GEOMETRIC_REPRESENTATION_ITEM()
RATIONAL_B_SPLINE_SURFACE(((0.982257720483865,0.990842547952629,1.,0.707106781186548,
1.,0.707106781186548,1.,0.707106781186548,1.,0.716264233233919,0.982257720483865),
(0.982257720483865,0.990842547952629,1.,0.707106781186548,1.,0.707106781186548,
1.,0.707106781186548,1.,0.716264233233919,0.982257720483865),(0.982257720483865,
0.990842547952629,1.,0.707106781186548,1.,0.707106781186548,1.,0.707106781186548,
1.,0.716264233233919,0.982257720483865),(0.982257720483865,0.990842547952629,
1.,0.707106781186548,1.,0.707106781186548,1.,0.707106781186548,1.,0.716264233233919,
0.982257720483865),(0.982257720483865,0.990842547952629,1.,0.707106781186548,
1.,0.707106781186548,1.,0.707106781186548,1.,0.716264233233919,0.982257720483865),
(0.982257720483865,0.990842547952629,1.,0.707106781186548,1.,0.707106781186548,
1.,0.707106781186548,1.,0.716264233233919,0.982257720483865),(0.982257720483865,
0.990842547952629,1.,0.707106781186548,1.,0.707106781186548,1.,0.707106781186548,
1.,0.716264233233919,0.982257720483865),(0.982257720483865,0.990842547952629,
1.,0.707106781186548,1.,0.707106781186548,1.,0.707106781186548,1.,0.716264233233919,
0.982257720483865),(0.982257720483865,0.990842547952629,1.,0.707106781186548,
1.,0.707106781186548,1.,0.707106781186548,1.,0.716264233233919,0.982257720483865),
(0.982257720483865,0.990842547952629,1.,0.707106781186548,1.,0.707106781186548,
1.,0.707106781186548,1.,0.716264233233919,0.982257720483865),(0.982257720483865,
0.990842547952629,1.,0.707106781186548,1.,0.707106781186548,1.,0.707106781186548,
1.,0.716264233233919,0.982257720483865),(0.982257720483865,0.990842547952629,
1.,0.707106781186548,1.,0.707106781186548,1.,0.707106781186548,1.,0.716264233233919,
0.982257720483865),(0.982257720483865,0.990842547952629,1.,0.707106781186548,
1.,0.707106781186548,1.,0.707106781186548,1.,0.716264233233919,0.982257720483865),
(0.982257720483865,0.990842547952629,1.,0.707106781186548,1.,0.707106781186548,
1.,0.707106781186548,1.,0.716264233233919,0.982257720483865),(0.982257720483865,
0.990842547952629,1.,0.707106781186548,1.,0.707106781186548,1.,0.707106781186548,
1.,0.716264233233919,0.982257720483865),(0.982257720483865,0.990842547952629,
1.,0.707106781186548,1.,0.707106781186548,1.,0.707106781186548,1.,0.716264233233919,
0.982257720483865),(0.982257720483865,0.990842547952629,1.,0.707106781186548,
1.,0.707106781186548,1.,0.707106781186548,1.,0.716264233233919,0.982257720483865),
(0.982257720483865,0.990842547952629,1.,0.707106781186548,1.,0.707106781186548,
1.,0.707106781186548,1.,0.716264233233919,0.982257720483865),(0.982257720483865,
0.990842547952629,1.,0.707106781186548,1.,0.707106781186548,1.,0.707106781186548,
1.,0.716264233233919,0.982257720483865),(0.982257720483865,0.990842547952629,
1.,0.707106781186548,1.,0.707106781186548,1.,0.707106781186548,1.,0.716264233233919,
0.982257720483865),(0.982257720483865,0.990842547952629,1.,0.707106781186548,
1.,0.707106781186548,1.,0.707106781186548,1.,0.716264233233919,0.982257720483865),
(0.982257720483865,0.990842547952629,1.,0.707106781186548,1.,0.707106781186548,
1.,0.707106781186548,1.,0.716264233233919,0.982257720483865),(0.982257720483865,
0.990842547952629,1.,0.707106781186548,1.,0.707106781186548,1.,0.707106781186548,
1.,0.716264233233919,0.982257720483865),(0.982257720483865,0.990842547952629,
1.,0.707106781186548,1.,0.707106781186548,1.,0.707106781186548,1.,0.716264233233919,
0.982257720483865),(0.982257720483865,0.990842547952629,1.,0.707106781186548,
1.,0.707106781186548,1.,0.707106781186548,1.,0.716264233233919,0.982257720483865)))
REPRESENTATION_ITEM('')
SURFACE()
);
#1067=(
BOUNDED_SURFACE()
B_SPLINE_SURFACE(5,2,((#36028,#36029,#36030,#36031,#36032,#36033,#36034,
#36035,#36036,#36037,#36038),(#36039,#36040,#36041,#36042,#36043,#36044,
#36045,#36046,#36047,#36048,#36049),(#36050,#36051,#36052,#36053,#36054,
#36055,#36056,#36057,#36058,#36059,#36060),(#36061,#36062,#36063,#36064,
#36065,#36066,#36067,#36068,#36069,#36070,#36071),(#36072,#36073,#36074,
#36075,#36076,#36077,#36078,#36079,#36080,#36081,#36082),(#36083,#36084,
#36085,#36086,#36087,#36088,#36089,#36090,#36091,#36092,#36093),(#36094,
#36095,#36096,#36097,#36098,#36099,#36100,#36101,#36102,#36103,#36104),
(#36105,#36106,#36107,#36108,#36109,#36110,#36111,#36112,#36113,#36114,
#36115),(#36116,#36117,#36118,#36119,#36120,#36121,#36122,#36123,#36124,
#36125,#36126),(#36127,#36128,#36129,#36130,#36131,#36132,#36133,#36134,
#36135,#36136,#36137),(#36138,#36139,#36140,#36141,#36142,#36143,#36144,
#36145,#36146,#36147,#36148),(#36149,#36150,#36151,#36152,#36153,#36154,
#36155,#36156,#36157,#36158,#36159),(#36160,#36161,#36162,#36163,#36164,
#36165,#36166,#36167,#36168,#36169,#36170),(#36171,#36172,#36173,#36174,
#36175,#36176,#36177,#36178,#36179,#36180,#36181),(#36182,#36183,#36184,
#36185,#36186,#36187,#36188,#36189,#36190,#36191,#36192),(#36193,#36194,
#36195,#36196,#36197,#36198,#36199,#36200,#36201,#36202,#36203),(#36204,
#36205,#36206,#36207,#36208,#36209,#36210,#36211,#36212,#36213,#36214),
(#36215,#36216,#36217,#36218,#36219,#36220,#36221,#36222,#36223,#36224,
#36225),(#36226,#36227,#36228,#36229,#36230,#36231,#36232,#36233,#36234,
#36235,#36236),(#36237,#36238,#36239,#36240,#36241,#36242,#36243,#36244,
#36245,#36246,#36247),(#36248,#36249,#36250,#36251,#36252,#36253,#36254,
#36255,#36256,#36257,#36258),(#36259,#36260,#36261,#36262,#36263,#36264,
#36265,#36266,#36267,#36268,#36269),(#36270,#36271,#36272,#36273,#36274,
#36275,#36276,#36277,#36278,#36279,#36280),(#36281,#36282,#36283,#36284,
#36285,#36286,#36287,#36288,#36289,#36290,#36291),(#36292,#36293,#36294,
#36295,#36296,#36297,#36298,#36299,#36300,#36301,#36302)),.UNSPECIFIED.,
 .F.,.T.,.F.)
B_SPLINE_SURFACE_WITH_KNOTS((6,1,1,1,1,1,1,1,1,1,1,1,1,1,1,1,1,1,1,1,6),
(3,2,2,2,2,3),(-1.,-0.95,-0.9,-0.85,-0.8,-0.75,-0.7,-0.65,-0.6,-0.55,-0.5,
-0.45,-0.4,-0.35,-0.3,-0.25,-0.2,-0.15,-0.1,-0.05,0.),(-0.0491117278067552,
0.,1.5707963267949,3.14159265358979,4.71238898038469,6.23407357937283),
 .UNSPECIFIED.)
GEOMETRIC_REPRESENTATION_ITEM()
RATIONAL_B_SPLINE_SURFACE(((0.982257720483865,0.990842547952629,1.,0.707106781186548,
1.,0.707106781186548,1.,0.707106781186548,1.,0.716264233233919,0.982257720483865),
(0.982257720483865,0.990842547952629,1.,0.707106781186548,1.,0.707106781186548,
1.,0.707106781186548,1.,0.716264233233919,0.982257720483865),(0.982257720483865,
0.990842547952629,1.,0.707106781186548,1.,0.707106781186548,1.,0.707106781186548,
1.,0.716264233233919,0.982257720483865),(0.982257720483865,0.990842547952629,
1.,0.707106781186548,1.,0.707106781186548,1.,0.707106781186548,1.,0.716264233233919,
0.982257720483865),(0.982257720483865,0.990842547952629,1.,0.707106781186548,
1.,0.707106781186548,1.,0.707106781186548,1.,0.716264233233919,0.982257720483865),
(0.982257720483865,0.990842547952629,1.,0.707106781186548,1.,0.707106781186548,
1.,0.707106781186548,1.,0.716264233233919,0.982257720483865),(0.982257720483865,
0.990842547952629,1.,0.707106781186548,1.,0.707106781186548,1.,0.707106781186548,
1.,0.716264233233919,0.982257720483865),(0.982257720483865,0.990842547952629,
1.,0.707106781186548,1.,0.707106781186548,1.,0.707106781186548,1.,0.716264233233919,
0.982257720483865),(0.982257720483865,0.990842547952629,1.,0.707106781186548,
1.,0.707106781186548,1.,0.707106781186548,1.,0.716264233233919,0.982257720483865),
(0.982257720483865,0.990842547952629,1.,0.707106781186548,1.,0.707106781186548,
1.,0.707106781186548,1.,0.716264233233919,0.982257720483865),(0.982257720483865,
0.990842547952629,1.,0.707106781186548,1.,0.707106781186548,1.,0.707106781186548,
1.,0.716264233233919,0.982257720483865),(0.982257720483865,0.990842547952629,
1.,0.707106781186548,1.,0.707106781186548,1.,0.707106781186548,1.,0.716264233233919,
0.982257720483865),(0.982257720483865,0.990842547952629,1.,0.707106781186548,
1.,0.707106781186548,1.,0.707106781186548,1.,0.716264233233919,0.982257720483865),
(0.982257720483865,0.990842547952629,1.,0.707106781186548,1.,0.707106781186548,
1.,0.707106781186548,1.,0.716264233233919,0.982257720483865),(0.982257720483865,
0.990842547952629,1.,0.707106781186548,1.,0.707106781186548,1.,0.707106781186548,
1.,0.716264233233919,0.982257720483865),(0.982257720483865,0.990842547952629,
1.,0.707106781186548,1.,0.707106781186548,1.,0.707106781186548,1.,0.716264233233919,
0.982257720483865),(0.982257720483865,0.990842547952629,1.,0.707106781186548,
1.,0.707106781186548,1.,0.707106781186548,1.,0.716264233233919,0.982257720483865),
(0.982257720483865,0.990842547952629,1.,0.707106781186548,1.,0.707106781186548,
1.,0.707106781186548,1.,0.716264233233919,0.982257720483865),(0.982257720483865,
0.990842547952629,1.,0.707106781186548,1.,0.707106781186548,1.,0.707106781186548,
1.,0.716264233233919,0.982257720483865),(0.982257720483865,0.990842547952629,
1.,0.707106781186548,1.,0.707106781186548,1.,0.707106781186548,1.,0.716264233233919,
0.982257720483865),(0.982257720483865,0.990842547952629,1.,0.707106781186548,
1.,0.707106781186548,1.,0.707106781186548,1.,0.716264233233919,0.982257720483865),
(0.982257720483865,0.990842547952629,1.,0.707106781186548,1.,0.707106781186548,
1.,0.707106781186548,1.,0.716264233233919,0.982257720483865),(0.982257720483865,
0.990842547952629,1.,0.707106781186548,1.,0.707106781186548,1.,0.707106781186548,
1.,0.716264233233919,0.982257720483865),(0.982257720483865,0.990842547952629,
1.,0.707106781186548,1.,0.707106781186548,1.,0.707106781186548,1.,0.716264233233919,
0.982257720483865),(0.982257720483865,0.990842547952629,1.,0.707106781186548,
1.,0.707106781186548,1.,0.707106781186548,1.,0.716264233233919,0.982257720483865)))
REPRESENTATION_ITEM('')
SURFACE()
);
#1068=(
BOUNDED_SURFACE()
B_SPLINE_SURFACE(5,2,((#36547,#36548,#36549,#36550,#36551,#36552,#36553,
#36554,#36555,#36556,#36557),(#36558,#36559,#36560,#36561,#36562,#36563,
#36564,#36565,#36566,#36567,#36568),(#36569,#36570,#36571,#36572,#36573,
#36574,#36575,#36576,#36577,#36578,#36579),(#36580,#36581,#36582,#36583,
#36584,#36585,#36586,#36587,#36588,#36589,#36590),(#36591,#36592,#36593,
#36594,#36595,#36596,#36597,#36598,#36599,#36600,#36601),(#36602,#36603,
#36604,#36605,#36606,#36607,#36608,#36609,#36610,#36611,#36612),(#36613,
#36614,#36615,#36616,#36617,#36618,#36619,#36620,#36621,#36622,#36623),
(#36624,#36625,#36626,#36627,#36628,#36629,#36630,#36631,#36632,#36633,
#36634),(#36635,#36636,#36637,#36638,#36639,#36640,#36641,#36642,#36643,
#36644,#36645),(#36646,#36647,#36648,#36649,#36650,#36651,#36652,#36653,
#36654,#36655,#36656),(#36657,#36658,#36659,#36660,#36661,#36662,#36663,
#36664,#36665,#36666,#36667),(#36668,#36669,#36670,#36671,#36672,#36673,
#36674,#36675,#36676,#36677,#36678),(#36679,#36680,#36681,#36682,#36683,
#36684,#36685,#36686,#36687,#36688,#36689),(#36690,#36691,#36692,#36693,
#36694,#36695,#36696,#36697,#36698,#36699,#36700),(#36701,#36702,#36703,
#36704,#36705,#36706,#36707,#36708,#36709,#36710,#36711),(#36712,#36713,
#36714,#36715,#36716,#36717,#36718,#36719,#36720,#36721,#36722),(#36723,
#36724,#36725,#36726,#36727,#36728,#36729,#36730,#36731,#36732,#36733),
(#36734,#36735,#36736,#36737,#36738,#36739,#36740,#36741,#36742,#36743,
#36744),(#36745,#36746,#36747,#36748,#36749,#36750,#36751,#36752,#36753,
#36754,#36755),(#36756,#36757,#36758,#36759,#36760,#36761,#36762,#36763,
#36764,#36765,#36766),(#36767,#36768,#36769,#36770,#36771,#36772,#36773,
#36774,#36775,#36776,#36777),(#36778,#36779,#36780,#36781,#36782,#36783,
#36784,#36785,#36786,#36787,#36788),(#36789,#36790,#36791,#36792,#36793,
#36794,#36795,#36796,#36797,#36798,#36799),(#36800,#36801,#36802,#36803,
#36804,#36805,#36806,#36807,#36808,#36809,#36810),(#36811,#36812,#36813,
#36814,#36815,#36816,#36817,#36818,#36819,#36820,#36821)),.UNSPECIFIED.,
 .F.,.T.,.F.)
B_SPLINE_SURFACE_WITH_KNOTS((6,1,1,1,1,1,1,1,1,1,1,1,1,1,1,1,1,1,1,1,6),
(3,2,2,2,2,3),(-1.,-0.95,-0.9,-0.85,-0.8,-0.75,-0.7,-0.65,-0.6,-0.55,-0.5,
-0.45,-0.4,-0.35,-0.3,-0.25,-0.2,-0.15,-0.1,-0.05,0.),(-0.0491117278067552,
0.,1.5707963267949,3.14159265358979,4.71238898038469,6.23407357937283),
 .UNSPECIFIED.)
GEOMETRIC_REPRESENTATION_ITEM()
RATIONAL_B_SPLINE_SURFACE(((0.982257720483865,0.990842547952629,1.,0.707106781186548,
1.,0.707106781186548,1.,0.707106781186548,1.,0.716264233233919,0.982257720483865),
(0.982257720483865,0.990842547952629,1.,0.707106781186548,1.,0.707106781186548,
1.,0.707106781186548,1.,0.716264233233919,0.982257720483865),(0.982257720483865,
0.990842547952629,1.,0.707106781186548,1.,0.707106781186548,1.,0.707106781186548,
1.,0.716264233233919,0.982257720483865),(0.982257720483865,0.990842547952629,
1.,0.707106781186548,1.,0.707106781186548,1.,0.707106781186548,1.,0.716264233233919,
0.982257720483865),(0.982257720483865,0.990842547952629,1.,0.707106781186548,
1.,0.707106781186548,1.,0.707106781186548,1.,0.716264233233919,0.982257720483865),
(0.982257720483865,0.990842547952629,1.,0.707106781186548,1.,0.707106781186548,
1.,0.707106781186548,1.,0.716264233233919,0.982257720483865),(0.982257720483865,
0.990842547952629,1.,0.707106781186548,1.,0.707106781186548,1.,0.707106781186548,
1.,0.716264233233919,0.982257720483865),(0.982257720483865,0.990842547952629,
1.,0.707106781186548,1.,0.707106781186548,1.,0.707106781186548,1.,0.716264233233919,
0.982257720483865),(0.982257720483865,0.990842547952629,1.,0.707106781186548,
1.,0.707106781186548,1.,0.707106781186548,1.,0.716264233233919,0.982257720483865),
(0.982257720483865,0.990842547952629,1.,0.707106781186548,1.,0.707106781186548,
1.,0.707106781186548,1.,0.716264233233919,0.982257720483865),(0.982257720483865,
0.990842547952629,1.,0.707106781186548,1.,0.707106781186548,1.,0.707106781186548,
1.,0.716264233233919,0.982257720483865),(0.982257720483865,0.990842547952629,
1.,0.707106781186548,1.,0.707106781186548,1.,0.707106781186548,1.,0.716264233233919,
0.982257720483865),(0.982257720483865,0.990842547952629,1.,0.707106781186548,
1.,0.707106781186548,1.,0.707106781186548,1.,0.716264233233919,0.982257720483865),
(0.982257720483865,0.990842547952629,1.,0.707106781186548,1.,0.707106781186548,
1.,0.707106781186548,1.,0.716264233233919,0.982257720483865),(0.982257720483865,
0.990842547952629,1.,0.707106781186548,1.,0.707106781186548,1.,0.707106781186548,
1.,0.716264233233919,0.982257720483865),(0.982257720483865,0.990842547952629,
1.,0.707106781186548,1.,0.707106781186548,1.,0.707106781186548,1.,0.716264233233919,
0.982257720483865),(0.982257720483865,0.990842547952629,1.,0.707106781186548,
1.,0.707106781186548,1.,0.707106781186548,1.,0.716264233233919,0.982257720483865),
(0.982257720483865,0.990842547952629,1.,0.707106781186548,1.,0.707106781186548,
1.,0.707106781186548,1.,0.716264233233919,0.982257720483865),(0.982257720483865,
0.990842547952629,1.,0.707106781186548,1.,0.707106781186548,1.,0.707106781186548,
1.,0.716264233233919,0.982257720483865),(0.982257720483865,0.990842547952629,
1.,0.707106781186548,1.,0.707106781186548,1.,0.707106781186548,1.,0.716264233233919,
0.982257720483865),(0.982257720483865,0.990842547952629,1.,0.707106781186548,
1.,0.707106781186548,1.,0.707106781186548,1.,0.716264233233919,0.982257720483865),
(0.982257720483865,0.990842547952629,1.,0.707106781186548,1.,0.707106781186548,
1.,0.707106781186548,1.,0.716264233233919,0.982257720483865),(0.982257720483865,
0.990842547952629,1.,0.707106781186548,1.,0.707106781186548,1.,0.707106781186548,
1.,0.716264233233919,0.982257720483865),(0.982257720483865,0.990842547952629,
1.,0.707106781186548,1.,0.707106781186548,1.,0.707106781186548,1.,0.716264233233919,
0.982257720483865),(0.982257720483865,0.990842547952629,1.,0.707106781186548,
1.,0.707106781186548,1.,0.707106781186548,1.,0.716264233233919,0.982257720483865)))
REPRESENTATION_ITEM('')
SURFACE()
);
#1069=(
BOUNDED_SURFACE()
B_SPLINE_SURFACE(5,2,((#37046,#37047,#37048,#37049,#37050,#37051,#37052,
#37053,#37054,#37055,#37056),(#37057,#37058,#37059,#37060,#37061,#37062,
#37063,#37064,#37065,#37066,#37067),(#37068,#37069,#37070,#37071,#37072,
#37073,#37074,#37075,#37076,#37077,#37078),(#37079,#37080,#37081,#37082,
#37083,#37084,#37085,#37086,#37087,#37088,#37089),(#37090,#37091,#37092,
#37093,#37094,#37095,#37096,#37097,#37098,#37099,#37100),(#37101,#37102,
#37103,#37104,#37105,#37106,#37107,#37108,#37109,#37110,#37111),(#37112,
#37113,#37114,#37115,#37116,#37117,#37118,#37119,#37120,#37121,#37122),
(#37123,#37124,#37125,#37126,#37127,#37128,#37129,#37130,#37131,#37132,
#37133),(#37134,#37135,#37136,#37137,#37138,#37139,#37140,#37141,#37142,
#37143,#37144),(#37145,#37146,#37147,#37148,#37149,#37150,#37151,#37152,
#37153,#37154,#37155),(#37156,#37157,#37158,#37159,#37160,#37161,#37162,
#37163,#37164,#37165,#37166),(#37167,#37168,#37169,#37170,#37171,#37172,
#37173,#37174,#37175,#37176,#37177),(#37178,#37179,#37180,#37181,#37182,
#37183,#37184,#37185,#37186,#37187,#37188),(#37189,#37190,#37191,#37192,
#37193,#37194,#37195,#37196,#37197,#37198,#37199),(#37200,#37201,#37202,
#37203,#37204,#37205,#37206,#37207,#37208,#37209,#37210),(#37211,#37212,
#37213,#37214,#37215,#37216,#37217,#37218,#37219,#37220,#37221),(#37222,
#37223,#37224,#37225,#37226,#37227,#37228,#37229,#37230,#37231,#37232),
(#37233,#37234,#37235,#37236,#37237,#37238,#37239,#37240,#37241,#37242,
#37243),(#37244,#37245,#37246,#37247,#37248,#37249,#37250,#37251,#37252,
#37253,#37254),(#37255,#37256,#37257,#37258,#37259,#37260,#37261,#37262,
#37263,#37264,#37265),(#37266,#37267,#37268,#37269,#37270,#37271,#37272,
#37273,#37274,#37275,#37276),(#37277,#37278,#37279,#37280,#37281,#37282,
#37283,#37284,#37285,#37286,#37287),(#37288,#37289,#37290,#37291,#37292,
#37293,#37294,#37295,#37296,#37297,#37298),(#37299,#37300,#37301,#37302,
#37303,#37304,#37305,#37306,#37307,#37308,#37309),(#37310,#37311,#37312,
#37313,#37314,#37315,#37316,#37317,#37318,#37319,#37320)),.UNSPECIFIED.,
 .F.,.T.,.F.)
B_SPLINE_SURFACE_WITH_KNOTS((6,1,1,1,1,1,1,1,1,1,1,1,1,1,1,1,1,1,1,1,6),
(3,2,2,2,2,3),(-1.,-0.95,-0.9,-0.85,-0.8,-0.75,-0.7,-0.65,-0.6,-0.55,-0.5,
-0.45,-0.4,-0.35,-0.3,-0.25,-0.2,-0.15,-0.1,-0.05,0.),(-0.0491117278067552,
0.,1.5707963267949,3.14159265358979,4.71238898038469,6.23407357937283),
 .UNSPECIFIED.)
GEOMETRIC_REPRESENTATION_ITEM()
RATIONAL_B_SPLINE_SURFACE(((0.982257720483865,0.990842547952629,1.,0.707106781186548,
1.,0.707106781186548,1.,0.707106781186548,1.,0.716264233233919,0.982257720483865),
(0.982257720483865,0.990842547952629,1.,0.707106781186548,1.,0.707106781186548,
1.,0.707106781186548,1.,0.716264233233919,0.982257720483865),(0.982257720483865,
0.990842547952629,1.,0.707106781186548,1.,0.707106781186548,1.,0.707106781186548,
1.,0.716264233233919,0.982257720483865),(0.982257720483865,0.990842547952629,
1.,0.707106781186548,1.,0.707106781186548,1.,0.707106781186548,1.,0.716264233233919,
0.982257720483865),(0.982257720483865,0.990842547952629,1.,0.707106781186548,
1.,0.707106781186548,1.,0.707106781186548,1.,0.716264233233919,0.982257720483865),
(0.982257720483865,0.990842547952629,1.,0.707106781186548,1.,0.707106781186548,
1.,0.707106781186548,1.,0.716264233233919,0.982257720483865),(0.982257720483865,
0.990842547952629,1.,0.707106781186548,1.,0.707106781186548,1.,0.707106781186548,
1.,0.716264233233919,0.982257720483865),(0.982257720483865,0.990842547952629,
1.,0.707106781186548,1.,0.707106781186548,1.,0.707106781186548,1.,0.716264233233919,
0.982257720483865),(0.982257720483865,0.990842547952629,1.,0.707106781186548,
1.,0.707106781186548,1.,0.707106781186548,1.,0.716264233233919,0.982257720483865),
(0.982257720483865,0.990842547952629,1.,0.707106781186548,1.,0.707106781186548,
1.,0.707106781186548,1.,0.716264233233919,0.982257720483865),(0.982257720483865,
0.990842547952629,1.,0.707106781186548,1.,0.707106781186548,1.,0.707106781186548,
1.,0.716264233233919,0.982257720483865),(0.982257720483865,0.990842547952629,
1.,0.707106781186548,1.,0.707106781186548,1.,0.707106781186548,1.,0.716264233233919,
0.982257720483865),(0.982257720483865,0.990842547952629,1.,0.707106781186548,
1.,0.707106781186548,1.,0.707106781186548,1.,0.716264233233919,0.982257720483865),
(0.982257720483865,0.990842547952629,1.,0.707106781186548,1.,0.707106781186548,
1.,0.707106781186548,1.,0.716264233233919,0.982257720483865),(0.982257720483865,
0.990842547952629,1.,0.707106781186548,1.,0.707106781186548,1.,0.707106781186548,
1.,0.716264233233919,0.982257720483865),(0.982257720483865,0.990842547952629,
1.,0.707106781186548,1.,0.707106781186548,1.,0.707106781186548,1.,0.716264233233919,
0.982257720483865),(0.982257720483865,0.990842547952629,1.,0.707106781186548,
1.,0.707106781186548,1.,0.707106781186548,1.,0.716264233233919,0.982257720483865),
(0.982257720483865,0.990842547952629,1.,0.707106781186548,1.,0.707106781186548,
1.,0.707106781186548,1.,0.716264233233919,0.982257720483865),(0.982257720483865,
0.990842547952629,1.,0.707106781186548,1.,0.707106781186548,1.,0.707106781186548,
1.,0.716264233233919,0.982257720483865),(0.982257720483865,0.990842547952629,
1.,0.707106781186548,1.,0.707106781186548,1.,0.707106781186548,1.,0.716264233233919,
0.982257720483865),(0.982257720483865,0.990842547952629,1.,0.707106781186548,
1.,0.707106781186548,1.,0.707106781186548,1.,0.716264233233919,0.982257720483865),
(0.982257720483865,0.990842547952629,1.,0.707106781186548,1.,0.707106781186548,
1.,0.707106781186548,1.,0.716264233233919,0.982257720483865),(0.982257720483865,
0.990842547952629,1.,0.707106781186548,1.,0.707106781186548,1.,0.707106781186548,
1.,0.716264233233919,0.982257720483865),(0.982257720483865,0.990842547952629,
1.,0.707106781186548,1.,0.707106781186548,1.,0.707106781186548,1.,0.716264233233919,
0.982257720483865),(0.982257720483865,0.990842547952629,1.,0.707106781186548,
1.,0.707106781186548,1.,0.707106781186548,1.,0.716264233233919,0.982257720483865)))
REPRESENTATION_ITEM('')
SURFACE()
);
#1070=(
BOUNDED_SURFACE()
B_SPLINE_SURFACE(5,2,((#37555,#37556,#37557,#37558,#37559,#37560,#37561,
#37562,#37563,#37564,#37565),(#37566,#37567,#37568,#37569,#37570,#37571,
#37572,#37573,#37574,#37575,#37576),(#37577,#37578,#37579,#37580,#37581,
#37582,#37583,#37584,#37585,#37586,#37587),(#37588,#37589,#37590,#37591,
#37592,#37593,#37594,#37595,#37596,#37597,#37598),(#37599,#37600,#37601,
#37602,#37603,#37604,#37605,#37606,#37607,#37608,#37609),(#37610,#37611,
#37612,#37613,#37614,#37615,#37616,#37617,#37618,#37619,#37620),(#37621,
#37622,#37623,#37624,#37625,#37626,#37627,#37628,#37629,#37630,#37631),
(#37632,#37633,#37634,#37635,#37636,#37637,#37638,#37639,#37640,#37641,
#37642),(#37643,#37644,#37645,#37646,#37647,#37648,#37649,#37650,#37651,
#37652,#37653),(#37654,#37655,#37656,#37657,#37658,#37659,#37660,#37661,
#37662,#37663,#37664),(#37665,#37666,#37667,#37668,#37669,#37670,#37671,
#37672,#37673,#37674,#37675),(#37676,#37677,#37678,#37679,#37680,#37681,
#37682,#37683,#37684,#37685,#37686),(#37687,#37688,#37689,#37690,#37691,
#37692,#37693,#37694,#37695,#37696,#37697),(#37698,#37699,#37700,#37701,
#37702,#37703,#37704,#37705,#37706,#37707,#37708),(#37709,#37710,#37711,
#37712,#37713,#37714,#37715,#37716,#37717,#37718,#37719),(#37720,#37721,
#37722,#37723,#37724,#37725,#37726,#37727,#37728,#37729,#37730),(#37731,
#37732,#37733,#37734,#37735,#37736,#37737,#37738,#37739,#37740,#37741),
(#37742,#37743,#37744,#37745,#37746,#37747,#37748,#37749,#37750,#37751,
#37752),(#37753,#37754,#37755,#37756,#37757,#37758,#37759,#37760,#37761,
#37762,#37763),(#37764,#37765,#37766,#37767,#37768,#37769,#37770,#37771,
#37772,#37773,#37774),(#37775,#37776,#37777,#37778,#37779,#37780,#37781,
#37782,#37783,#37784,#37785),(#37786,#37787,#37788,#37789,#37790,#37791,
#37792,#37793,#37794,#37795,#37796),(#37797,#37798,#37799,#37800,#37801,
#37802,#37803,#37804,#37805,#37806,#37807),(#37808,#37809,#37810,#37811,
#37812,#37813,#37814,#37815,#37816,#37817,#37818),(#37819,#37820,#37821,
#37822,#37823,#37824,#37825,#37826,#37827,#37828,#37829)),.UNSPECIFIED.,
 .F.,.T.,.F.)
B_SPLINE_SURFACE_WITH_KNOTS((6,1,1,1,1,1,1,1,1,1,1,1,1,1,1,1,1,1,1,1,6),
(3,2,2,2,2,3),(-1.,-0.95,-0.9,-0.85,-0.8,-0.75,-0.7,-0.65,-0.6,-0.55,-0.5,
-0.45,-0.4,-0.35,-0.3,-0.25,-0.2,-0.15,-0.1,-0.05,0.),(-0.0491117278067552,
0.,1.5707963267949,3.14159265358979,4.71238898038469,6.23407357937283),
 .UNSPECIFIED.)
GEOMETRIC_REPRESENTATION_ITEM()
RATIONAL_B_SPLINE_SURFACE(((0.982257720483865,0.990842547952629,1.,0.707106781186548,
1.,0.707106781186548,1.,0.707106781186548,1.,0.716264233233919,0.982257720483865),
(0.982257720483865,0.990842547952629,1.,0.707106781186548,1.,0.707106781186548,
1.,0.707106781186548,1.,0.716264233233919,0.982257720483865),(0.982257720483865,
0.990842547952629,1.,0.707106781186548,1.,0.707106781186548,1.,0.707106781186548,
1.,0.716264233233919,0.982257720483865),(0.982257720483865,0.990842547952629,
1.,0.707106781186548,1.,0.707106781186548,1.,0.707106781186548,1.,0.716264233233919,
0.982257720483865),(0.982257720483865,0.990842547952629,1.,0.707106781186548,
1.,0.707106781186548,1.,0.707106781186548,1.,0.716264233233919,0.982257720483865),
(0.982257720483865,0.990842547952629,1.,0.707106781186548,1.,0.707106781186548,
1.,0.707106781186548,1.,0.716264233233919,0.982257720483865),(0.982257720483865,
0.990842547952629,1.,0.707106781186548,1.,0.707106781186548,1.,0.707106781186548,
1.,0.716264233233919,0.982257720483865),(0.982257720483865,0.990842547952629,
1.,0.707106781186548,1.,0.707106781186548,1.,0.707106781186548,1.,0.716264233233919,
0.982257720483865),(0.982257720483865,0.990842547952629,1.,0.707106781186548,
1.,0.707106781186548,1.,0.707106781186548,1.,0.716264233233919,0.982257720483865),
(0.982257720483865,0.990842547952629,1.,0.707106781186548,1.,0.707106781186548,
1.,0.707106781186548,1.,0.716264233233919,0.982257720483865),(0.982257720483865,
0.990842547952629,1.,0.707106781186548,1.,0.707106781186548,1.,0.707106781186548,
1.,0.716264233233919,0.982257720483865),(0.982257720483865,0.990842547952629,
1.,0.707106781186548,1.,0.707106781186548,1.,0.707106781186548,1.,0.716264233233919,
0.982257720483865),(0.982257720483865,0.990842547952629,1.,0.707106781186548,
1.,0.707106781186548,1.,0.707106781186548,1.,0.716264233233919,0.982257720483865),
(0.982257720483865,0.990842547952629,1.,0.707106781186548,1.,0.707106781186548,
1.,0.707106781186548,1.,0.716264233233919,0.982257720483865),(0.982257720483865,
0.990842547952629,1.,0.707106781186548,1.,0.707106781186548,1.,0.707106781186548,
1.,0.716264233233919,0.982257720483865),(0.982257720483865,0.990842547952629,
1.,0.707106781186548,1.,0.707106781186548,1.,0.707106781186548,1.,0.716264233233919,
0.982257720483865),(0.982257720483865,0.990842547952629,1.,0.707106781186548,
1.,0.707106781186548,1.,0.707106781186548,1.,0.716264233233919,0.982257720483865),
(0.982257720483865,0.990842547952629,1.,0.707106781186548,1.,0.707106781186548,
1.,0.707106781186548,1.,0.716264233233919,0.982257720483865),(0.982257720483865,
0.990842547952629,1.,0.707106781186548,1.,0.707106781186548,1.,0.707106781186548,
1.,0.716264233233919,0.982257720483865),(0.982257720483865,0.990842547952629,
1.,0.707106781186548,1.,0.707106781186548,1.,0.707106781186548,1.,0.716264233233919,
0.982257720483865),(0.982257720483865,0.990842547952629,1.,0.707106781186548,
1.,0.707106781186548,1.,0.707106781186548,1.,0.716264233233919,0.982257720483865),
(0.982257720483865,0.990842547952629,1.,0.707106781186548,1.,0.707106781186548,
1.,0.707106781186548,1.,0.716264233233919,0.982257720483865),(0.982257720483865,
0.990842547952629,1.,0.707106781186548,1.,0.707106781186548,1.,0.707106781186548,
1.,0.716264233233919,0.982257720483865),(0.982257720483865,0.990842547952629,
1.,0.707106781186548,1.,0.707106781186548,1.,0.707106781186548,1.,0.716264233233919,
0.982257720483865),(0.982257720483865,0.990842547952629,1.,0.707106781186548,
1.,0.707106781186548,1.,0.707106781186548,1.,0.716264233233919,0.982257720483865)))
REPRESENTATION_ITEM('')
SURFACE()
);
#1071=(
BOUNDED_SURFACE()
B_SPLINE_SURFACE(5,2,((#38074,#38075,#38076,#38077,#38078,#38079,#38080,
#38081,#38082,#38083,#38084),(#38085,#38086,#38087,#38088,#38089,#38090,
#38091,#38092,#38093,#38094,#38095),(#38096,#38097,#38098,#38099,#38100,
#38101,#38102,#38103,#38104,#38105,#38106),(#38107,#38108,#38109,#38110,
#38111,#38112,#38113,#38114,#38115,#38116,#38117),(#38118,#38119,#38120,
#38121,#38122,#38123,#38124,#38125,#38126,#38127,#38128),(#38129,#38130,
#38131,#38132,#38133,#38134,#38135,#38136,#38137,#38138,#38139),(#38140,
#38141,#38142,#38143,#38144,#38145,#38146,#38147,#38148,#38149,#38150),
(#38151,#38152,#38153,#38154,#38155,#38156,#38157,#38158,#38159,#38160,
#38161),(#38162,#38163,#38164,#38165,#38166,#38167,#38168,#38169,#38170,
#38171,#38172),(#38173,#38174,#38175,#38176,#38177,#38178,#38179,#38180,
#38181,#38182,#38183),(#38184,#38185,#38186,#38187,#38188,#38189,#38190,
#38191,#38192,#38193,#38194),(#38195,#38196,#38197,#38198,#38199,#38200,
#38201,#38202,#38203,#38204,#38205),(#38206,#38207,#38208,#38209,#38210,
#38211,#38212,#38213,#38214,#38215,#38216),(#38217,#38218,#38219,#38220,
#38221,#38222,#38223,#38224,#38225,#38226,#38227),(#38228,#38229,#38230,
#38231,#38232,#38233,#38234,#38235,#38236,#38237,#38238),(#38239,#38240,
#38241,#38242,#38243,#38244,#38245,#38246,#38247,#38248,#38249),(#38250,
#38251,#38252,#38253,#38254,#38255,#38256,#38257,#38258,#38259,#38260),
(#38261,#38262,#38263,#38264,#38265,#38266,#38267,#38268,#38269,#38270,
#38271),(#38272,#38273,#38274,#38275,#38276,#38277,#38278,#38279,#38280,
#38281,#38282),(#38283,#38284,#38285,#38286,#38287,#38288,#38289,#38290,
#38291,#38292,#38293),(#38294,#38295,#38296,#38297,#38298,#38299,#38300,
#38301,#38302,#38303,#38304),(#38305,#38306,#38307,#38308,#38309,#38310,
#38311,#38312,#38313,#38314,#38315),(#38316,#38317,#38318,#38319,#38320,
#38321,#38322,#38323,#38324,#38325,#38326),(#38327,#38328,#38329,#38330,
#38331,#38332,#38333,#38334,#38335,#38336,#38337),(#38338,#38339,#38340,
#38341,#38342,#38343,#38344,#38345,#38346,#38347,#38348)),.UNSPECIFIED.,
 .F.,.T.,.F.)
B_SPLINE_SURFACE_WITH_KNOTS((6,1,1,1,1,1,1,1,1,1,1,1,1,1,1,1,1,1,1,1,6),
(3,2,2,2,2,3),(-1.,-0.95,-0.9,-0.85,-0.8,-0.75,-0.7,-0.65,-0.6,-0.55,-0.5,
-0.45,-0.4,-0.35,-0.3,-0.25,-0.2,-0.15,-0.1,-0.05,0.),(-0.0491117278067552,
0.,1.5707963267949,3.14159265358979,4.71238898038469,6.23407357937283),
 .UNSPECIFIED.)
GEOMETRIC_REPRESENTATION_ITEM()
RATIONAL_B_SPLINE_SURFACE(((0.982257720483865,0.990842547952629,1.,0.707106781186548,
1.,0.707106781186548,1.,0.707106781186548,1.,0.716264233233919,0.982257720483865),
(0.982257720483865,0.990842547952629,1.,0.707106781186548,1.,0.707106781186548,
1.,0.707106781186548,1.,0.716264233233919,0.982257720483865),(0.982257720483865,
0.990842547952629,1.,0.707106781186548,1.,0.707106781186548,1.,0.707106781186548,
1.,0.716264233233919,0.982257720483865),(0.982257720483865,0.990842547952629,
1.,0.707106781186548,1.,0.707106781186548,1.,0.707106781186548,1.,0.716264233233919,
0.982257720483865),(0.982257720483865,0.990842547952629,1.,0.707106781186548,
1.,0.707106781186548,1.,0.707106781186548,1.,0.716264233233919,0.982257720483865),
(0.982257720483865,0.990842547952629,1.,0.707106781186548,1.,0.707106781186548,
1.,0.707106781186548,1.,0.716264233233919,0.982257720483865),(0.982257720483865,
0.990842547952629,1.,0.707106781186548,1.,0.707106781186548,1.,0.707106781186548,
1.,0.716264233233919,0.982257720483865),(0.982257720483865,0.990842547952629,
1.,0.707106781186548,1.,0.707106781186548,1.,0.707106781186548,1.,0.716264233233919,
0.982257720483865),(0.982257720483865,0.990842547952629,1.,0.707106781186548,
1.,0.707106781186548,1.,0.707106781186548,1.,0.716264233233919,0.982257720483865),
(0.982257720483865,0.990842547952629,1.,0.707106781186548,1.,0.707106781186548,
1.,0.707106781186548,1.,0.716264233233919,0.982257720483865),(0.982257720483865,
0.990842547952629,1.,0.707106781186548,1.,0.707106781186548,1.,0.707106781186548,
1.,0.716264233233919,0.982257720483865),(0.982257720483865,0.990842547952629,
1.,0.707106781186548,1.,0.707106781186548,1.,0.707106781186548,1.,0.716264233233919,
0.982257720483865),(0.982257720483865,0.990842547952629,1.,0.707106781186548,
1.,0.707106781186548,1.,0.707106781186548,1.,0.716264233233919,0.982257720483865),
(0.982257720483865,0.990842547952629,1.,0.707106781186548,1.,0.707106781186548,
1.,0.707106781186548,1.,0.716264233233919,0.982257720483865),(0.982257720483865,
0.990842547952629,1.,0.707106781186548,1.,0.707106781186548,1.,0.707106781186548,
1.,0.716264233233919,0.982257720483865),(0.982257720483865,0.990842547952629,
1.,0.707106781186548,1.,0.707106781186548,1.,0.707106781186548,1.,0.716264233233919,
0.982257720483865),(0.982257720483865,0.990842547952629,1.,0.707106781186548,
1.,0.707106781186548,1.,0.707106781186548,1.,0.716264233233919,0.982257720483865),
(0.982257720483865,0.990842547952629,1.,0.707106781186548,1.,0.707106781186548,
1.,0.707106781186548,1.,0.716264233233919,0.982257720483865),(0.982257720483865,
0.990842547952629,1.,0.707106781186548,1.,0.707106781186548,1.,0.707106781186548,
1.,0.716264233233919,0.982257720483865),(0.982257720483865,0.990842547952629,
1.,0.707106781186548,1.,0.707106781186548,1.,0.707106781186548,1.,0.716264233233919,
0.982257720483865),(0.982257720483865,0.990842547952629,1.,0.707106781186548,
1.,0.707106781186548,1.,0.707106781186548,1.,0.716264233233919,0.982257720483865),
(0.982257720483865,0.990842547952629,1.,0.707106781186548,1.,0.707106781186548,
1.,0.707106781186548,1.,0.716264233233919,0.982257720483865),(0.982257720483865,
0.990842547952629,1.,0.707106781186548,1.,0.707106781186548,1.,0.707106781186548,
1.,0.716264233233919,0.982257720483865),(0.982257720483865,0.990842547952629,
1.,0.707106781186548,1.,0.707106781186548,1.,0.707106781186548,1.,0.716264233233919,
0.982257720483865),(0.982257720483865,0.990842547952629,1.,0.707106781186548,
1.,0.707106781186548,1.,0.707106781186548,1.,0.716264233233919,0.982257720483865)))
REPRESENTATION_ITEM('')
SURFACE()
);
#1072=(
BOUNDED_SURFACE()
B_SPLINE_SURFACE(5,2,((#38573,#38574,#38575,#38576,#38577,#38578,#38579,
#38580,#38581,#38582,#38583),(#38584,#38585,#38586,#38587,#38588,#38589,
#38590,#38591,#38592,#38593,#38594),(#38595,#38596,#38597,#38598,#38599,
#38600,#38601,#38602,#38603,#38604,#38605),(#38606,#38607,#38608,#38609,
#38610,#38611,#38612,#38613,#38614,#38615,#38616),(#38617,#38618,#38619,
#38620,#38621,#38622,#38623,#38624,#38625,#38626,#38627),(#38628,#38629,
#38630,#38631,#38632,#38633,#38634,#38635,#38636,#38637,#38638),(#38639,
#38640,#38641,#38642,#38643,#38644,#38645,#38646,#38647,#38648,#38649),
(#38650,#38651,#38652,#38653,#38654,#38655,#38656,#38657,#38658,#38659,
#38660),(#38661,#38662,#38663,#38664,#38665,#38666,#38667,#38668,#38669,
#38670,#38671),(#38672,#38673,#38674,#38675,#38676,#38677,#38678,#38679,
#38680,#38681,#38682),(#38683,#38684,#38685,#38686,#38687,#38688,#38689,
#38690,#38691,#38692,#38693),(#38694,#38695,#38696,#38697,#38698,#38699,
#38700,#38701,#38702,#38703,#38704),(#38705,#38706,#38707,#38708,#38709,
#38710,#38711,#38712,#38713,#38714,#38715),(#38716,#38717,#38718,#38719,
#38720,#38721,#38722,#38723,#38724,#38725,#38726),(#38727,#38728,#38729,
#38730,#38731,#38732,#38733,#38734,#38735,#38736,#38737),(#38738,#38739,
#38740,#38741,#38742,#38743,#38744,#38745,#38746,#38747,#38748),(#38749,
#38750,#38751,#38752,#38753,#38754,#38755,#38756,#38757,#38758,#38759),
(#38760,#38761,#38762,#38763,#38764,#38765,#38766,#38767,#38768,#38769,
#38770),(#38771,#38772,#38773,#38774,#38775,#38776,#38777,#38778,#38779,
#38780,#38781),(#38782,#38783,#38784,#38785,#38786,#38787,#38788,#38789,
#38790,#38791,#38792),(#38793,#38794,#38795,#38796,#38797,#38798,#38799,
#38800,#38801,#38802,#38803),(#38804,#38805,#38806,#38807,#38808,#38809,
#38810,#38811,#38812,#38813,#38814),(#38815,#38816,#38817,#38818,#38819,
#38820,#38821,#38822,#38823,#38824,#38825),(#38826,#38827,#38828,#38829,
#38830,#38831,#38832,#38833,#38834,#38835,#38836),(#38837,#38838,#38839,
#38840,#38841,#38842,#38843,#38844,#38845,#38846,#38847)),.UNSPECIFIED.,
 .F.,.T.,.F.)
B_SPLINE_SURFACE_WITH_KNOTS((6,1,1,1,1,1,1,1,1,1,1,1,1,1,1,1,1,1,1,1,6),
(3,2,2,2,2,3),(-1.,-0.95,-0.9,-0.85,-0.8,-0.75,-0.7,-0.65,-0.6,-0.55,-0.5,
-0.45,-0.4,-0.35,-0.3,-0.25,-0.2,-0.15,-0.1,-0.05,0.),(-0.0491117278067552,
0.,1.5707963267949,3.14159265358979,4.71238898038469,6.23407357937283),
 .UNSPECIFIED.)
GEOMETRIC_REPRESENTATION_ITEM()
RATIONAL_B_SPLINE_SURFACE(((0.982257720483865,0.990842547952629,1.,0.707106781186548,
1.,0.707106781186548,1.,0.707106781186548,1.,0.716264233233919,0.982257720483865),
(0.982257720483865,0.990842547952629,1.,0.707106781186548,1.,0.707106781186548,
1.,0.707106781186548,1.,0.716264233233919,0.982257720483865),(0.982257720483865,
0.990842547952629,1.,0.707106781186548,1.,0.707106781186548,1.,0.707106781186548,
1.,0.716264233233919,0.982257720483865),(0.982257720483865,0.990842547952629,
1.,0.707106781186548,1.,0.707106781186548,1.,0.707106781186548,1.,0.716264233233919,
0.982257720483865),(0.982257720483865,0.990842547952629,1.,0.707106781186548,
1.,0.707106781186548,1.,0.707106781186548,1.,0.716264233233919,0.982257720483865),
(0.982257720483865,0.990842547952629,1.,0.707106781186548,1.,0.707106781186548,
1.,0.707106781186548,1.,0.716264233233919,0.982257720483865),(0.982257720483865,
0.990842547952629,1.,0.707106781186548,1.,0.707106781186548,1.,0.707106781186548,
1.,0.716264233233919,0.982257720483865),(0.982257720483865,0.990842547952629,
1.,0.707106781186548,1.,0.707106781186548,1.,0.707106781186548,1.,0.716264233233919,
0.982257720483865),(0.982257720483865,0.990842547952629,1.,0.707106781186548,
1.,0.707106781186548,1.,0.707106781186548,1.,0.716264233233919,0.982257720483865),
(0.982257720483865,0.990842547952629,1.,0.707106781186548,1.,0.707106781186548,
1.,0.707106781186548,1.,0.716264233233919,0.982257720483865),(0.982257720483865,
0.990842547952629,1.,0.707106781186548,1.,0.707106781186548,1.,0.707106781186548,
1.,0.716264233233919,0.982257720483865),(0.982257720483865,0.990842547952629,
1.,0.707106781186548,1.,0.707106781186548,1.,0.707106781186548,1.,0.716264233233919,
0.982257720483865),(0.982257720483865,0.990842547952629,1.,0.707106781186548,
1.,0.707106781186548,1.,0.707106781186548,1.,0.716264233233919,0.982257720483865),
(0.982257720483865,0.990842547952629,1.,0.707106781186548,1.,0.707106781186548,
1.,0.707106781186548,1.,0.716264233233919,0.982257720483865),(0.982257720483865,
0.990842547952629,1.,0.707106781186548,1.,0.707106781186548,1.,0.707106781186548,
1.,0.716264233233919,0.982257720483865),(0.982257720483865,0.990842547952629,
1.,0.707106781186548,1.,0.707106781186548,1.,0.707106781186548,1.,0.716264233233919,
0.982257720483865),(0.982257720483865,0.990842547952629,1.,0.707106781186548,
1.,0.707106781186548,1.,0.707106781186548,1.,0.716264233233919,0.982257720483865),
(0.982257720483865,0.990842547952629,1.,0.707106781186548,1.,0.707106781186548,
1.,0.707106781186548,1.,0.716264233233919,0.982257720483865),(0.982257720483865,
0.990842547952629,1.,0.707106781186548,1.,0.707106781186548,1.,0.707106781186548,
1.,0.716264233233919,0.982257720483865),(0.982257720483865,0.990842547952629,
1.,0.707106781186548,1.,0.707106781186548,1.,0.707106781186548,1.,0.716264233233919,
0.982257720483865),(0.982257720483865,0.990842547952629,1.,0.707106781186548,
1.,0.707106781186548,1.,0.707106781186548,1.,0.716264233233919,0.982257720483865),
(0.982257720483865,0.990842547952629,1.,0.707106781186548,1.,0.707106781186548,
1.,0.707106781186548,1.,0.716264233233919,0.982257720483865),(0.982257720483865,
0.990842547952629,1.,0.707106781186548,1.,0.707106781186548,1.,0.707106781186548,
1.,0.716264233233919,0.982257720483865),(0.982257720483865,0.990842547952629,
1.,0.707106781186548,1.,0.707106781186548,1.,0.707106781186548,1.,0.716264233233919,
0.982257720483865),(0.982257720483865,0.990842547952629,1.,0.707106781186548,
1.,0.707106781186548,1.,0.707106781186548,1.,0.716264233233919,0.982257720483865)))
REPRESENTATION_ITEM('')
SURFACE()
);
#1073=(
BOUNDED_SURFACE()
B_SPLINE_SURFACE(5,2,((#39082,#39083,#39084,#39085,#39086,#39087,#39088,
#39089,#39090,#39091,#39092),(#39093,#39094,#39095,#39096,#39097,#39098,
#39099,#39100,#39101,#39102,#39103),(#39104,#39105,#39106,#39107,#39108,
#39109,#39110,#39111,#39112,#39113,#39114),(#39115,#39116,#39117,#39118,
#39119,#39120,#39121,#39122,#39123,#39124,#39125),(#39126,#39127,#39128,
#39129,#39130,#39131,#39132,#39133,#39134,#39135,#39136),(#39137,#39138,
#39139,#39140,#39141,#39142,#39143,#39144,#39145,#39146,#39147),(#39148,
#39149,#39150,#39151,#39152,#39153,#39154,#39155,#39156,#39157,#39158),
(#39159,#39160,#39161,#39162,#39163,#39164,#39165,#39166,#39167,#39168,
#39169),(#39170,#39171,#39172,#39173,#39174,#39175,#39176,#39177,#39178,
#39179,#39180),(#39181,#39182,#39183,#39184,#39185,#39186,#39187,#39188,
#39189,#39190,#39191),(#39192,#39193,#39194,#39195,#39196,#39197,#39198,
#39199,#39200,#39201,#39202),(#39203,#39204,#39205,#39206,#39207,#39208,
#39209,#39210,#39211,#39212,#39213),(#39214,#39215,#39216,#39217,#39218,
#39219,#39220,#39221,#39222,#39223,#39224),(#39225,#39226,#39227,#39228,
#39229,#39230,#39231,#39232,#39233,#39234,#39235),(#39236,#39237,#39238,
#39239,#39240,#39241,#39242,#39243,#39244,#39245,#39246),(#39247,#39248,
#39249,#39250,#39251,#39252,#39253,#39254,#39255,#39256,#39257),(#39258,
#39259,#39260,#39261,#39262,#39263,#39264,#39265,#39266,#39267,#39268),
(#39269,#39270,#39271,#39272,#39273,#39274,#39275,#39276,#39277,#39278,
#39279),(#39280,#39281,#39282,#39283,#39284,#39285,#39286,#39287,#39288,
#39289,#39290),(#39291,#39292,#39293,#39294,#39295,#39296,#39297,#39298,
#39299,#39300,#39301),(#39302,#39303,#39304,#39305,#39306,#39307,#39308,
#39309,#39310,#39311,#39312),(#39313,#39314,#39315,#39316,#39317,#39318,
#39319,#39320,#39321,#39322,#39323),(#39324,#39325,#39326,#39327,#39328,
#39329,#39330,#39331,#39332,#39333,#39334),(#39335,#39336,#39337,#39338,
#39339,#39340,#39341,#39342,#39343,#39344,#39345),(#39346,#39347,#39348,
#39349,#39350,#39351,#39352,#39353,#39354,#39355,#39356)),.UNSPECIFIED.,
 .F.,.T.,.F.)
B_SPLINE_SURFACE_WITH_KNOTS((6,1,1,1,1,1,1,1,1,1,1,1,1,1,1,1,1,1,1,1,6),
(3,2,2,2,2,3),(-1.,-0.95,-0.9,-0.85,-0.8,-0.75,-0.7,-0.65,-0.6,-0.55,-0.5,
-0.45,-0.4,-0.35,-0.3,-0.25,-0.2,-0.15,-0.1,-0.05,0.),(-0.0491117278067552,
0.,1.5707963267949,3.14159265358979,4.71238898038469,6.23407357937283),
 .UNSPECIFIED.)
GEOMETRIC_REPRESENTATION_ITEM()
RATIONAL_B_SPLINE_SURFACE(((0.982257720483865,0.990842547952629,1.,0.707106781186548,
1.,0.707106781186548,1.,0.707106781186548,1.,0.716264233233919,0.982257720483865),
(0.982257720483865,0.990842547952629,1.,0.707106781186548,1.,0.707106781186548,
1.,0.707106781186548,1.,0.716264233233919,0.982257720483865),(0.982257720483865,
0.990842547952629,1.,0.707106781186548,1.,0.707106781186548,1.,0.707106781186548,
1.,0.716264233233919,0.982257720483865),(0.982257720483865,0.990842547952629,
1.,0.707106781186548,1.,0.707106781186548,1.,0.707106781186548,1.,0.716264233233919,
0.982257720483865),(0.982257720483865,0.990842547952629,1.,0.707106781186548,
1.,0.707106781186548,1.,0.707106781186548,1.,0.716264233233919,0.982257720483865),
(0.982257720483865,0.990842547952629,1.,0.707106781186548,1.,0.707106781186548,
1.,0.707106781186548,1.,0.716264233233919,0.982257720483865),(0.982257720483865,
0.990842547952629,1.,0.707106781186548,1.,0.707106781186548,1.,0.707106781186548,
1.,0.716264233233919,0.982257720483865),(0.982257720483865,0.990842547952629,
1.,0.707106781186548,1.,0.707106781186548,1.,0.707106781186548,1.,0.716264233233919,
0.982257720483865),(0.982257720483865,0.990842547952629,1.,0.707106781186548,
1.,0.707106781186548,1.,0.707106781186548,1.,0.716264233233919,0.982257720483865),
(0.982257720483865,0.990842547952629,1.,0.707106781186548,1.,0.707106781186548,
1.,0.707106781186548,1.,0.716264233233919,0.982257720483865),(0.982257720483865,
0.990842547952629,1.,0.707106781186548,1.,0.707106781186548,1.,0.707106781186548,
1.,0.716264233233919,0.982257720483865),(0.982257720483865,0.990842547952629,
1.,0.707106781186548,1.,0.707106781186548,1.,0.707106781186548,1.,0.716264233233919,
0.982257720483865),(0.982257720483865,0.990842547952629,1.,0.707106781186548,
1.,0.707106781186548,1.,0.707106781186548,1.,0.716264233233919,0.982257720483865),
(0.982257720483865,0.990842547952629,1.,0.707106781186548,1.,0.707106781186548,
1.,0.707106781186548,1.,0.716264233233919,0.982257720483865),(0.982257720483865,
0.990842547952629,1.,0.707106781186548,1.,0.707106781186548,1.,0.707106781186548,
1.,0.716264233233919,0.982257720483865),(0.982257720483865,0.990842547952629,
1.,0.707106781186548,1.,0.707106781186548,1.,0.707106781186548,1.,0.716264233233919,
0.982257720483865),(0.982257720483865,0.990842547952629,1.,0.707106781186548,
1.,0.707106781186548,1.,0.707106781186548,1.,0.716264233233919,0.982257720483865),
(0.982257720483865,0.990842547952629,1.,0.707106781186548,1.,0.707106781186548,
1.,0.707106781186548,1.,0.716264233233919,0.982257720483865),(0.982257720483865,
0.990842547952629,1.,0.707106781186548,1.,0.707106781186548,1.,0.707106781186548,
1.,0.716264233233919,0.982257720483865),(0.982257720483865,0.990842547952629,
1.,0.707106781186548,1.,0.707106781186548,1.,0.707106781186548,1.,0.716264233233919,
0.982257720483865),(0.982257720483865,0.990842547952629,1.,0.707106781186548,
1.,0.707106781186548,1.,0.707106781186548,1.,0.716264233233919,0.982257720483865),
(0.982257720483865,0.990842547952629,1.,0.707106781186548,1.,0.707106781186548,
1.,0.707106781186548,1.,0.716264233233919,0.982257720483865),(0.982257720483865,
0.990842547952629,1.,0.707106781186548,1.,0.707106781186548,1.,0.707106781186548,
1.,0.716264233233919,0.982257720483865),(0.982257720483865,0.990842547952629,
1.,0.707106781186548,1.,0.707106781186548,1.,0.707106781186548,1.,0.716264233233919,
0.982257720483865),(0.982257720483865,0.990842547952629,1.,0.707106781186548,
1.,0.707106781186548,1.,0.707106781186548,1.,0.716264233233919,0.982257720483865)))
REPRESENTATION_ITEM('')
SURFACE()
);
#1074=(
BOUNDED_SURFACE()
B_SPLINE_SURFACE(5,2,((#39601,#39602,#39603,#39604,#39605,#39606,#39607,
#39608,#39609,#39610,#39611),(#39612,#39613,#39614,#39615,#39616,#39617,
#39618,#39619,#39620,#39621,#39622),(#39623,#39624,#39625,#39626,#39627,
#39628,#39629,#39630,#39631,#39632,#39633),(#39634,#39635,#39636,#39637,
#39638,#39639,#39640,#39641,#39642,#39643,#39644),(#39645,#39646,#39647,
#39648,#39649,#39650,#39651,#39652,#39653,#39654,#39655),(#39656,#39657,
#39658,#39659,#39660,#39661,#39662,#39663,#39664,#39665,#39666),(#39667,
#39668,#39669,#39670,#39671,#39672,#39673,#39674,#39675,#39676,#39677),
(#39678,#39679,#39680,#39681,#39682,#39683,#39684,#39685,#39686,#39687,
#39688),(#39689,#39690,#39691,#39692,#39693,#39694,#39695,#39696,#39697,
#39698,#39699),(#39700,#39701,#39702,#39703,#39704,#39705,#39706,#39707,
#39708,#39709,#39710),(#39711,#39712,#39713,#39714,#39715,#39716,#39717,
#39718,#39719,#39720,#39721),(#39722,#39723,#39724,#39725,#39726,#39727,
#39728,#39729,#39730,#39731,#39732),(#39733,#39734,#39735,#39736,#39737,
#39738,#39739,#39740,#39741,#39742,#39743),(#39744,#39745,#39746,#39747,
#39748,#39749,#39750,#39751,#39752,#39753,#39754),(#39755,#39756,#39757,
#39758,#39759,#39760,#39761,#39762,#39763,#39764,#39765),(#39766,#39767,
#39768,#39769,#39770,#39771,#39772,#39773,#39774,#39775,#39776),(#39777,
#39778,#39779,#39780,#39781,#39782,#39783,#39784,#39785,#39786,#39787),
(#39788,#39789,#39790,#39791,#39792,#39793,#39794,#39795,#39796,#39797,
#39798),(#39799,#39800,#39801,#39802,#39803,#39804,#39805,#39806,#39807,
#39808,#39809),(#39810,#39811,#39812,#39813,#39814,#39815,#39816,#39817,
#39818,#39819,#39820),(#39821,#39822,#39823,#39824,#39825,#39826,#39827,
#39828,#39829,#39830,#39831),(#39832,#39833,#39834,#39835,#39836,#39837,
#39838,#39839,#39840,#39841,#39842),(#39843,#39844,#39845,#39846,#39847,
#39848,#39849,#39850,#39851,#39852,#39853),(#39854,#39855,#39856,#39857,
#39858,#39859,#39860,#39861,#39862,#39863,#39864),(#39865,#39866,#39867,
#39868,#39869,#39870,#39871,#39872,#39873,#39874,#39875)),.UNSPECIFIED.,
 .F.,.T.,.F.)
B_SPLINE_SURFACE_WITH_KNOTS((6,1,1,1,1,1,1,1,1,1,1,1,1,1,1,1,1,1,1,1,6),
(3,2,2,2,2,3),(-1.,-0.95,-0.9,-0.85,-0.8,-0.75,-0.7,-0.65,-0.6,-0.55,-0.5,
-0.45,-0.4,-0.35,-0.3,-0.25,-0.2,-0.15,-0.1,-0.05,0.),(-0.0491117278067552,
0.,1.5707963267949,3.14159265358979,4.71238898038469,6.23407357937283),
 .UNSPECIFIED.)
GEOMETRIC_REPRESENTATION_ITEM()
RATIONAL_B_SPLINE_SURFACE(((0.982257720483865,0.990842547952629,1.,0.707106781186548,
1.,0.707106781186548,1.,0.707106781186548,1.,0.716264233233919,0.982257720483865),
(0.982257720483865,0.990842547952629,1.,0.707106781186548,1.,0.707106781186548,
1.,0.707106781186548,1.,0.716264233233919,0.982257720483865),(0.982257720483865,
0.990842547952629,1.,0.707106781186548,1.,0.707106781186548,1.,0.707106781186548,
1.,0.716264233233919,0.982257720483865),(0.982257720483865,0.990842547952629,
1.,0.707106781186548,1.,0.707106781186548,1.,0.707106781186548,1.,0.716264233233919,
0.982257720483865),(0.982257720483865,0.990842547952629,1.,0.707106781186548,
1.,0.707106781186548,1.,0.707106781186548,1.,0.716264233233919,0.982257720483865),
(0.982257720483865,0.990842547952629,1.,0.707106781186548,1.,0.707106781186548,
1.,0.707106781186548,1.,0.716264233233919,0.982257720483865),(0.982257720483865,
0.990842547952629,1.,0.707106781186548,1.,0.707106781186548,1.,0.707106781186548,
1.,0.716264233233919,0.982257720483865),(0.982257720483865,0.990842547952629,
1.,0.707106781186548,1.,0.707106781186548,1.,0.707106781186548,1.,0.716264233233919,
0.982257720483865),(0.982257720483865,0.990842547952629,1.,0.707106781186548,
1.,0.707106781186548,1.,0.707106781186548,1.,0.716264233233919,0.982257720483865),
(0.982257720483865,0.990842547952629,1.,0.707106781186548,1.,0.707106781186548,
1.,0.707106781186548,1.,0.716264233233919,0.982257720483865),(0.982257720483865,
0.990842547952629,1.,0.707106781186548,1.,0.707106781186548,1.,0.707106781186548,
1.,0.716264233233919,0.982257720483865),(0.982257720483865,0.990842547952629,
1.,0.707106781186548,1.,0.707106781186548,1.,0.707106781186548,1.,0.716264233233919,
0.982257720483865),(0.982257720483865,0.990842547952629,1.,0.707106781186548,
1.,0.707106781186548,1.,0.707106781186548,1.,0.716264233233919,0.982257720483865),
(0.982257720483865,0.990842547952629,1.,0.707106781186548,1.,0.707106781186548,
1.,0.707106781186548,1.,0.716264233233919,0.982257720483865),(0.982257720483865,
0.990842547952629,1.,0.707106781186548,1.,0.707106781186548,1.,0.707106781186548,
1.,0.716264233233919,0.982257720483865),(0.982257720483865,0.990842547952629,
1.,0.707106781186548,1.,0.707106781186548,1.,0.707106781186548,1.,0.716264233233919,
0.982257720483865),(0.982257720483865,0.990842547952629,1.,0.707106781186548,
1.,0.707106781186548,1.,0.707106781186548,1.,0.716264233233919,0.982257720483865),
(0.982257720483865,0.990842547952629,1.,0.707106781186548,1.,0.707106781186548,
1.,0.707106781186548,1.,0.716264233233919,0.982257720483865),(0.982257720483865,
0.990842547952629,1.,0.707106781186548,1.,0.707106781186548,1.,0.707106781186548,
1.,0.716264233233919,0.982257720483865),(0.982257720483865,0.990842547952629,
1.,0.707106781186548,1.,0.707106781186548,1.,0.707106781186548,1.,0.716264233233919,
0.982257720483865),(0.982257720483865,0.990842547952629,1.,0.707106781186548,
1.,0.707106781186548,1.,0.707106781186548,1.,0.716264233233919,0.982257720483865),
(0.982257720483865,0.990842547952629,1.,0.707106781186548,1.,0.707106781186548,
1.,0.707106781186548,1.,0.716264233233919,0.982257720483865),(0.982257720483865,
0.990842547952629,1.,0.707106781186548,1.,0.707106781186548,1.,0.707106781186548,
1.,0.716264233233919,0.982257720483865),(0.982257720483865,0.990842547952629,
1.,0.707106781186548,1.,0.707106781186548,1.,0.707106781186548,1.,0.716264233233919,
0.982257720483865),(0.982257720483865,0.990842547952629,1.,0.707106781186548,
1.,0.707106781186548,1.,0.707106781186548,1.,0.716264233233919,0.982257720483865)))
REPRESENTATION_ITEM('')
SURFACE()
);
#1075=(
BOUNDED_SURFACE()
B_SPLINE_SURFACE(5,2,((#40110,#40111,#40112,#40113,#40114,#40115,#40116,
#40117,#40118,#40119,#40120),(#40121,#40122,#40123,#40124,#40125,#40126,
#40127,#40128,#40129,#40130,#40131),(#40132,#40133,#40134,#40135,#40136,
#40137,#40138,#40139,#40140,#40141,#40142),(#40143,#40144,#40145,#40146,
#40147,#40148,#40149,#40150,#40151,#40152,#40153),(#40154,#40155,#40156,
#40157,#40158,#40159,#40160,#40161,#40162,#40163,#40164),(#40165,#40166,
#40167,#40168,#40169,#40170,#40171,#40172,#40173,#40174,#40175),(#40176,
#40177,#40178,#40179,#40180,#40181,#40182,#40183,#40184,#40185,#40186),
(#40187,#40188,#40189,#40190,#40191,#40192,#40193,#40194,#40195,#40196,
#40197),(#40198,#40199,#40200,#40201,#40202,#40203,#40204,#40205,#40206,
#40207,#40208),(#40209,#40210,#40211,#40212,#40213,#40214,#40215,#40216,
#40217,#40218,#40219),(#40220,#40221,#40222,#40223,#40224,#40225,#40226,
#40227,#40228,#40229,#40230),(#40231,#40232,#40233,#40234,#40235,#40236,
#40237,#40238,#40239,#40240,#40241),(#40242,#40243,#40244,#40245,#40246,
#40247,#40248,#40249,#40250,#40251,#40252),(#40253,#40254,#40255,#40256,
#40257,#40258,#40259,#40260,#40261,#40262,#40263),(#40264,#40265,#40266,
#40267,#40268,#40269,#40270,#40271,#40272,#40273,#40274),(#40275,#40276,
#40277,#40278,#40279,#40280,#40281,#40282,#40283,#40284,#40285),(#40286,
#40287,#40288,#40289,#40290,#40291,#40292,#40293,#40294,#40295,#40296),
(#40297,#40298,#40299,#40300,#40301,#40302,#40303,#40304,#40305,#40306,
#40307),(#40308,#40309,#40310,#40311,#40312,#40313,#40314,#40315,#40316,
#40317,#40318),(#40319,#40320,#40321,#40322,#40323,#40324,#40325,#40326,
#40327,#40328,#40329),(#40330,#40331,#40332,#40333,#40334,#40335,#40336,
#40337,#40338,#40339,#40340),(#40341,#40342,#40343,#40344,#40345,#40346,
#40347,#40348,#40349,#40350,#40351),(#40352,#40353,#40354,#40355,#40356,
#40357,#40358,#40359,#40360,#40361,#40362),(#40363,#40364,#40365,#40366,
#40367,#40368,#40369,#40370,#40371,#40372,#40373),(#40374,#40375,#40376,
#40377,#40378,#40379,#40380,#40381,#40382,#40383,#40384)),.UNSPECIFIED.,
 .F.,.T.,.F.)
B_SPLINE_SURFACE_WITH_KNOTS((6,1,1,1,1,1,1,1,1,1,1,1,1,1,1,1,1,1,1,1,6),
(3,2,2,2,2,3),(-1.,-0.95,-0.9,-0.85,-0.8,-0.75,-0.7,-0.65,-0.6,-0.55,-0.5,
-0.45,-0.4,-0.35,-0.3,-0.25,-0.2,-0.15,-0.1,-0.05,0.),(-0.0491117278067552,
0.,1.5707963267949,3.14159265358979,4.71238898038469,6.23407357937283),
 .UNSPECIFIED.)
GEOMETRIC_REPRESENTATION_ITEM()
RATIONAL_B_SPLINE_SURFACE(((0.982257720483865,0.990842547952629,1.,0.707106781186548,
1.,0.707106781186548,1.,0.707106781186548,1.,0.716264233233919,0.982257720483865),
(0.982257720483865,0.990842547952629,1.,0.707106781186548,1.,0.707106781186548,
1.,0.707106781186548,1.,0.716264233233919,0.982257720483865),(0.982257720483865,
0.990842547952629,1.,0.707106781186548,1.,0.707106781186548,1.,0.707106781186548,
1.,0.716264233233919,0.982257720483865),(0.982257720483865,0.990842547952629,
1.,0.707106781186548,1.,0.707106781186548,1.,0.707106781186548,1.,0.716264233233919,
0.982257720483865),(0.982257720483865,0.990842547952629,1.,0.707106781186548,
1.,0.707106781186548,1.,0.707106781186548,1.,0.716264233233919,0.982257720483865),
(0.982257720483865,0.990842547952629,1.,0.707106781186548,1.,0.707106781186548,
1.,0.707106781186548,1.,0.716264233233919,0.982257720483865),(0.982257720483865,
0.990842547952629,1.,0.707106781186548,1.,0.707106781186548,1.,0.707106781186548,
1.,0.716264233233919,0.982257720483865),(0.982257720483865,0.990842547952629,
1.,0.707106781186548,1.,0.707106781186548,1.,0.707106781186548,1.,0.716264233233919,
0.982257720483865),(0.982257720483865,0.990842547952629,1.,0.707106781186548,
1.,0.707106781186548,1.,0.707106781186548,1.,0.716264233233919,0.982257720483865),
(0.982257720483865,0.990842547952629,1.,0.707106781186548,1.,0.707106781186548,
1.,0.707106781186548,1.,0.716264233233919,0.982257720483865),(0.982257720483865,
0.990842547952629,1.,0.707106781186548,1.,0.707106781186548,1.,0.707106781186548,
1.,0.716264233233919,0.982257720483865),(0.982257720483865,0.990842547952629,
1.,0.707106781186548,1.,0.707106781186548,1.,0.707106781186548,1.,0.716264233233919,
0.982257720483865),(0.982257720483865,0.990842547952629,1.,0.707106781186548,
1.,0.707106781186548,1.,0.707106781186548,1.,0.716264233233919,0.982257720483865),
(0.982257720483865,0.990842547952629,1.,0.707106781186548,1.,0.707106781186548,
1.,0.707106781186548,1.,0.716264233233919,0.982257720483865),(0.982257720483865,
0.990842547952629,1.,0.707106781186548,1.,0.707106781186548,1.,0.707106781186548,
1.,0.716264233233919,0.982257720483865),(0.982257720483865,0.990842547952629,
1.,0.707106781186548,1.,0.707106781186548,1.,0.707106781186548,1.,0.716264233233919,
0.982257720483865),(0.982257720483865,0.990842547952629,1.,0.707106781186548,
1.,0.707106781186548,1.,0.707106781186548,1.,0.716264233233919,0.982257720483865),
(0.982257720483865,0.990842547952629,1.,0.707106781186548,1.,0.707106781186548,
1.,0.707106781186548,1.,0.716264233233919,0.982257720483865),(0.982257720483865,
0.990842547952629,1.,0.707106781186548,1.,0.707106781186548,1.,0.707106781186548,
1.,0.716264233233919,0.982257720483865),(0.982257720483865,0.990842547952629,
1.,0.707106781186548,1.,0.707106781186548,1.,0.707106781186548,1.,0.716264233233919,
0.982257720483865),(0.982257720483865,0.990842547952629,1.,0.707106781186548,
1.,0.707106781186548,1.,0.707106781186548,1.,0.716264233233919,0.982257720483865),
(0.982257720483865,0.990842547952629,1.,0.707106781186548,1.,0.707106781186548,
1.,0.707106781186548,1.,0.716264233233919,0.982257720483865),(0.982257720483865,
0.990842547952629,1.,0.707106781186548,1.,0.707106781186548,1.,0.707106781186548,
1.,0.716264233233919,0.982257720483865),(0.982257720483865,0.990842547952629,
1.,0.707106781186548,1.,0.707106781186548,1.,0.707106781186548,1.,0.716264233233919,
0.982257720483865),(0.982257720483865,0.990842547952629,1.,0.707106781186548,
1.,0.707106781186548,1.,0.707106781186548,1.,0.716264233233919,0.982257720483865)))
REPRESENTATION_ITEM('')
SURFACE()
);
#1076=(
BOUNDED_SURFACE()
B_SPLINE_SURFACE(5,2,((#40619,#40620,#40621,#40622,#40623,#40624,#40625,
#40626,#40627,#40628,#40629),(#40630,#40631,#40632,#40633,#40634,#40635,
#40636,#40637,#40638,#40639,#40640),(#40641,#40642,#40643,#40644,#40645,
#40646,#40647,#40648,#40649,#40650,#40651),(#40652,#40653,#40654,#40655,
#40656,#40657,#40658,#40659,#40660,#40661,#40662),(#40663,#40664,#40665,
#40666,#40667,#40668,#40669,#40670,#40671,#40672,#40673),(#40674,#40675,
#40676,#40677,#40678,#40679,#40680,#40681,#40682,#40683,#40684),(#40685,
#40686,#40687,#40688,#40689,#40690,#40691,#40692,#40693,#40694,#40695),
(#40696,#40697,#40698,#40699,#40700,#40701,#40702,#40703,#40704,#40705,
#40706),(#40707,#40708,#40709,#40710,#40711,#40712,#40713,#40714,#40715,
#40716,#40717),(#40718,#40719,#40720,#40721,#40722,#40723,#40724,#40725,
#40726,#40727,#40728),(#40729,#40730,#40731,#40732,#40733,#40734,#40735,
#40736,#40737,#40738,#40739),(#40740,#40741,#40742,#40743,#40744,#40745,
#40746,#40747,#40748,#40749,#40750),(#40751,#40752,#40753,#40754,#40755,
#40756,#40757,#40758,#40759,#40760,#40761),(#40762,#40763,#40764,#40765,
#40766,#40767,#40768,#40769,#40770,#40771,#40772),(#40773,#40774,#40775,
#40776,#40777,#40778,#40779,#40780,#40781,#40782,#40783),(#40784,#40785,
#40786,#40787,#40788,#40789,#40790,#40791,#40792,#40793,#40794),(#40795,
#40796,#40797,#40798,#40799,#40800,#40801,#40802,#40803,#40804,#40805),
(#40806,#40807,#40808,#40809,#40810,#40811,#40812,#40813,#40814,#40815,
#40816),(#40817,#40818,#40819,#40820,#40821,#40822,#40823,#40824,#40825,
#40826,#40827),(#40828,#40829,#40830,#40831,#40832,#40833,#40834,#40835,
#40836,#40837,#40838),(#40839,#40840,#40841,#40842,#40843,#40844,#40845,
#40846,#40847,#40848,#40849),(#40850,#40851,#40852,#40853,#40854,#40855,
#40856,#40857,#40858,#40859,#40860),(#40861,#40862,#40863,#40864,#40865,
#40866,#40867,#40868,#40869,#40870,#40871),(#40872,#40873,#40874,#40875,
#40876,#40877,#40878,#40879,#40880,#40881,#40882),(#40883,#40884,#40885,
#40886,#40887,#40888,#40889,#40890,#40891,#40892,#40893)),.UNSPECIFIED.,
 .F.,.T.,.F.)
B_SPLINE_SURFACE_WITH_KNOTS((6,1,1,1,1,1,1,1,1,1,1,1,1,1,1,1,1,1,1,1,6),
(3,2,2,2,2,3),(-1.,-0.95,-0.9,-0.85,-0.8,-0.75,-0.7,-0.65,-0.6,-0.55,-0.5,
-0.45,-0.4,-0.35,-0.3,-0.25,-0.2,-0.15,-0.1,-0.05,0.),(-0.0491117278067552,
0.,1.5707963267949,3.14159265358979,4.71238898038469,6.23407357937283),
 .UNSPECIFIED.)
GEOMETRIC_REPRESENTATION_ITEM()
RATIONAL_B_SPLINE_SURFACE(((0.982257720483865,0.990842547952629,1.,0.707106781186548,
1.,0.707106781186548,1.,0.707106781186548,1.,0.716264233233919,0.982257720483865),
(0.982257720483865,0.990842547952629,1.,0.707106781186548,1.,0.707106781186548,
1.,0.707106781186548,1.,0.716264233233919,0.982257720483865),(0.982257720483865,
0.990842547952629,1.,0.707106781186548,1.,0.707106781186548,1.,0.707106781186548,
1.,0.716264233233919,0.982257720483865),(0.982257720483865,0.990842547952629,
1.,0.707106781186548,1.,0.707106781186548,1.,0.707106781186548,1.,0.716264233233919,
0.982257720483865),(0.982257720483865,0.990842547952629,1.,0.707106781186548,
1.,0.707106781186548,1.,0.707106781186548,1.,0.716264233233919,0.982257720483865),
(0.982257720483865,0.990842547952629,1.,0.707106781186548,1.,0.707106781186548,
1.,0.707106781186548,1.,0.716264233233919,0.982257720483865),(0.982257720483865,
0.990842547952629,1.,0.707106781186548,1.,0.707106781186548,1.,0.707106781186548,
1.,0.716264233233919,0.982257720483865),(0.982257720483865,0.990842547952629,
1.,0.707106781186548,1.,0.707106781186548,1.,0.707106781186548,1.,0.716264233233919,
0.982257720483865),(0.982257720483865,0.990842547952629,1.,0.707106781186548,
1.,0.707106781186548,1.,0.707106781186548,1.,0.716264233233919,0.982257720483865),
(0.982257720483865,0.990842547952629,1.,0.707106781186548,1.,0.707106781186548,
1.,0.707106781186548,1.,0.716264233233919,0.982257720483865),(0.982257720483865,
0.990842547952629,1.,0.707106781186548,1.,0.707106781186548,1.,0.707106781186548,
1.,0.716264233233919,0.982257720483865),(0.982257720483865,0.990842547952629,
1.,0.707106781186548,1.,0.707106781186548,1.,0.707106781186548,1.,0.716264233233919,
0.982257720483865),(0.982257720483865,0.990842547952629,1.,0.707106781186548,
1.,0.707106781186548,1.,0.707106781186548,1.,0.716264233233919,0.982257720483865),
(0.982257720483865,0.990842547952629,1.,0.707106781186548,1.,0.707106781186548,
1.,0.707106781186548,1.,0.716264233233919,0.982257720483865),(0.982257720483865,
0.990842547952629,1.,0.707106781186548,1.,0.707106781186548,1.,0.707106781186548,
1.,0.716264233233919,0.982257720483865),(0.982257720483865,0.990842547952629,
1.,0.707106781186548,1.,0.707106781186548,1.,0.707106781186548,1.,0.716264233233919,
0.982257720483865),(0.982257720483865,0.990842547952629,1.,0.707106781186548,
1.,0.707106781186548,1.,0.707106781186548,1.,0.716264233233919,0.982257720483865),
(0.982257720483865,0.990842547952629,1.,0.707106781186548,1.,0.707106781186548,
1.,0.707106781186548,1.,0.716264233233919,0.982257720483865),(0.982257720483865,
0.990842547952629,1.,0.707106781186548,1.,0.707106781186548,1.,0.707106781186548,
1.,0.716264233233919,0.982257720483865),(0.982257720483865,0.990842547952629,
1.,0.707106781186548,1.,0.707106781186548,1.,0.707106781186548,1.,0.716264233233919,
0.982257720483865),(0.982257720483865,0.990842547952629,1.,0.707106781186548,
1.,0.707106781186548,1.,0.707106781186548,1.,0.716264233233919,0.982257720483865),
(0.982257720483865,0.990842547952629,1.,0.707106781186548,1.,0.707106781186548,
1.,0.707106781186548,1.,0.716264233233919,0.982257720483865),(0.982257720483865,
0.990842547952629,1.,0.707106781186548,1.,0.707106781186548,1.,0.707106781186548,
1.,0.716264233233919,0.982257720483865),(0.982257720483865,0.990842547952629,
1.,0.707106781186548,1.,0.707106781186548,1.,0.707106781186548,1.,0.716264233233919,
0.982257720483865),(0.982257720483865,0.990842547952629,1.,0.707106781186548,
1.,0.707106781186548,1.,0.707106781186548,1.,0.716264233233919,0.982257720483865)))
REPRESENTATION_ITEM('')
SURFACE()
);
#1077=(
BOUNDED_SURFACE()
B_SPLINE_SURFACE(5,2,((#41138,#41139,#41140,#41141,#41142,#41143,#41144,
#41145,#41146,#41147,#41148),(#41149,#41150,#41151,#41152,#41153,#41154,
#41155,#41156,#41157,#41158,#41159),(#41160,#41161,#41162,#41163,#41164,
#41165,#41166,#41167,#41168,#41169,#41170),(#41171,#41172,#41173,#41174,
#41175,#41176,#41177,#41178,#41179,#41180,#41181),(#41182,#41183,#41184,
#41185,#41186,#41187,#41188,#41189,#41190,#41191,#41192),(#41193,#41194,
#41195,#41196,#41197,#41198,#41199,#41200,#41201,#41202,#41203),(#41204,
#41205,#41206,#41207,#41208,#41209,#41210,#41211,#41212,#41213,#41214),
(#41215,#41216,#41217,#41218,#41219,#41220,#41221,#41222,#41223,#41224,
#41225),(#41226,#41227,#41228,#41229,#41230,#41231,#41232,#41233,#41234,
#41235,#41236),(#41237,#41238,#41239,#41240,#41241,#41242,#41243,#41244,
#41245,#41246,#41247),(#41248,#41249,#41250,#41251,#41252,#41253,#41254,
#41255,#41256,#41257,#41258),(#41259,#41260,#41261,#41262,#41263,#41264,
#41265,#41266,#41267,#41268,#41269),(#41270,#41271,#41272,#41273,#41274,
#41275,#41276,#41277,#41278,#41279,#41280),(#41281,#41282,#41283,#41284,
#41285,#41286,#41287,#41288,#41289,#41290,#41291),(#41292,#41293,#41294,
#41295,#41296,#41297,#41298,#41299,#41300,#41301,#41302),(#41303,#41304,
#41305,#41306,#41307,#41308,#41309,#41310,#41311,#41312,#41313),(#41314,
#41315,#41316,#41317,#41318,#41319,#41320,#41321,#41322,#41323,#41324),
(#41325,#41326,#41327,#41328,#41329,#41330,#41331,#41332,#41333,#41334,
#41335),(#41336,#41337,#41338,#41339,#41340,#41341,#41342,#41343,#41344,
#41345,#41346),(#41347,#41348,#41349,#41350,#41351,#41352,#41353,#41354,
#41355,#41356,#41357),(#41358,#41359,#41360,#41361,#41362,#41363,#41364,
#41365,#41366,#41367,#41368),(#41369,#41370,#41371,#41372,#41373,#41374,
#41375,#41376,#41377,#41378,#41379),(#41380,#41381,#41382,#41383,#41384,
#41385,#41386,#41387,#41388,#41389,#41390),(#41391,#41392,#41393,#41394,
#41395,#41396,#41397,#41398,#41399,#41400,#41401),(#41402,#41403,#41404,
#41405,#41406,#41407,#41408,#41409,#41410,#41411,#41412)),.UNSPECIFIED.,
 .F.,.T.,.F.)
B_SPLINE_SURFACE_WITH_KNOTS((6,1,1,1,1,1,1,1,1,1,1,1,1,1,1,1,1,1,1,1,6),
(3,2,2,2,2,3),(-1.,-0.95,-0.9,-0.85,-0.8,-0.75,-0.7,-0.65,-0.6,-0.55,-0.5,
-0.45,-0.4,-0.35,-0.3,-0.25,-0.2,-0.15,-0.1,-0.05,0.),(-0.0491117278067552,
0.,1.5707963267949,3.14159265358979,4.71238898038469,6.23407357937283),
 .UNSPECIFIED.)
GEOMETRIC_REPRESENTATION_ITEM()
RATIONAL_B_SPLINE_SURFACE(((0.982257720483865,0.990842547952629,1.,0.707106781186548,
1.,0.707106781186548,1.,0.707106781186548,1.,0.716264233233919,0.982257720483865),
(0.982257720483865,0.990842547952629,1.,0.707106781186548,1.,0.707106781186548,
1.,0.707106781186548,1.,0.716264233233919,0.982257720483865),(0.982257720483865,
0.990842547952629,1.,0.707106781186548,1.,0.707106781186548,1.,0.707106781186548,
1.,0.716264233233919,0.982257720483865),(0.982257720483865,0.990842547952629,
1.,0.707106781186548,1.,0.707106781186548,1.,0.707106781186548,1.,0.716264233233919,
0.982257720483865),(0.982257720483865,0.990842547952629,1.,0.707106781186548,
1.,0.707106781186548,1.,0.707106781186548,1.,0.716264233233919,0.982257720483865),
(0.982257720483865,0.990842547952629,1.,0.707106781186548,1.,0.707106781186548,
1.,0.707106781186548,1.,0.716264233233919,0.982257720483865),(0.982257720483865,
0.990842547952629,1.,0.707106781186548,1.,0.707106781186548,1.,0.707106781186548,
1.,0.716264233233919,0.982257720483865),(0.982257720483865,0.990842547952629,
1.,0.707106781186548,1.,0.707106781186548,1.,0.707106781186548,1.,0.716264233233919,
0.982257720483865),(0.982257720483865,0.990842547952629,1.,0.707106781186548,
1.,0.707106781186548,1.,0.707106781186548,1.,0.716264233233919,0.982257720483865),
(0.982257720483865,0.990842547952629,1.,0.707106781186548,1.,0.707106781186548,
1.,0.707106781186548,1.,0.716264233233919,0.982257720483865),(0.982257720483865,
0.990842547952629,1.,0.707106781186548,1.,0.707106781186548,1.,0.707106781186548,
1.,0.716264233233919,0.982257720483865),(0.982257720483865,0.990842547952629,
1.,0.707106781186548,1.,0.707106781186548,1.,0.707106781186548,1.,0.716264233233919,
0.982257720483865),(0.982257720483865,0.990842547952629,1.,0.707106781186548,
1.,0.707106781186548,1.,0.707106781186548,1.,0.716264233233919,0.982257720483865),
(0.982257720483865,0.990842547952629,1.,0.707106781186548,1.,0.707106781186548,
1.,0.707106781186548,1.,0.716264233233919,0.982257720483865),(0.982257720483865,
0.990842547952629,1.,0.707106781186548,1.,0.707106781186548,1.,0.707106781186548,
1.,0.716264233233919,0.982257720483865),(0.982257720483865,0.990842547952629,
1.,0.707106781186548,1.,0.707106781186548,1.,0.707106781186548,1.,0.716264233233919,
0.982257720483865),(0.982257720483865,0.990842547952629,1.,0.707106781186548,
1.,0.707106781186548,1.,0.707106781186548,1.,0.716264233233919,0.982257720483865),
(0.982257720483865,0.990842547952629,1.,0.707106781186548,1.,0.707106781186548,
1.,0.707106781186548,1.,0.716264233233919,0.982257720483865),(0.982257720483865,
0.990842547952629,1.,0.707106781186548,1.,0.707106781186548,1.,0.707106781186548,
1.,0.716264233233919,0.982257720483865),(0.982257720483865,0.990842547952629,
1.,0.707106781186548,1.,0.707106781186548,1.,0.707106781186548,1.,0.716264233233919,
0.982257720483865),(0.982257720483865,0.990842547952629,1.,0.707106781186548,
1.,0.707106781186548,1.,0.707106781186548,1.,0.716264233233919,0.982257720483865),
(0.982257720483865,0.990842547952629,1.,0.707106781186548,1.,0.707106781186548,
1.,0.707106781186548,1.,0.716264233233919,0.982257720483865),(0.982257720483865,
0.990842547952629,1.,0.707106781186548,1.,0.707106781186548,1.,0.707106781186548,
1.,0.716264233233919,0.982257720483865),(0.982257720483865,0.990842547952629,
1.,0.707106781186548,1.,0.707106781186548,1.,0.707106781186548,1.,0.716264233233919,
0.982257720483865),(0.982257720483865,0.990842547952629,1.,0.707106781186548,
1.,0.707106781186548,1.,0.707106781186548,1.,0.716264233233919,0.982257720483865)))
REPRESENTATION_ITEM('')
SURFACE()
);
#1078=(
BOUNDED_SURFACE()
B_SPLINE_SURFACE(5,1,((#41857,#41858),(#41859,#41860),(#41861,#41862),(#41863,
#41864),(#41865,#41866),(#41867,#41868),(#41869,#41870),(#41871,#41872),
(#41873,#41874),(#41875,#41876),(#41877,#41878),(#41879,#41880),(#41881,
#41882),(#41883,#41884),(#41885,#41886),(#41887,#41888),(#41889,#41890),
(#41891,#41892),(#41893,#41894),(#41895,#41896),(#41897,#41898),(#41899,
#41900),(#41901,#41902),(#41903,#41904),(#41905,#41906),(#41907,#41908),
(#41909,#41910),(#41911,#41912),(#41913,#41914),(#41915,#41916),(#41917,
#41918),(#41919,#41920),(#41921,#41922),(#41923,#41924),(#41925,#41926),
(#41927,#41928),(#41929,#41930),(#41931,#41932),(#41933,#41934),(#41935,
#41936),(#41937,#41938),(#41939,#41940),(#41941,#41942),(#41943,#41944),
(#41945,#41946),(#41947,#41948),(#41949,#41950),(#41951,#41952),(#41953,
#41954),(#41955,#41956),(#41957,#41958),(#41959,#41960),(#41961,#41962),
(#41963,#41964),(#41965,#41966),(#41967,#41968),(#41969,#41970),(#41971,
#41972),(#41973,#41974),(#41975,#41976),(#41977,#41978),(#41979,#41980),
(#41981,#41982),(#41983,#41984),(#41985,#41986),(#41987,#41988),(#41989,
#41990),(#41991,#41992),(#41993,#41994),(#41995,#41996),(#41997,#41998),
(#41999,#42000),(#42001,#42002),(#42003,#42004),(#42005,#42006),(#42007,
#42008),(#42009,#42010),(#42011,#42012),(#42013,#42014),(#42015,#42016),
(#42017,#42018),(#42019,#42020),(#42021,#42022),(#42023,#42024),(#42025,
#42026),(#42027,#42028),(#42029,#42030),(#42031,#42032),(#42033,#42034),
(#42035,#42036),(#42037,#42038),(#42039,#42040),(#42041,#42042),(#42043,
#42044),(#42045,#42046),(#42047,#42048),(#42049,#42050),(#42051,#42052),
(#42053,#42054),(#42055,#42056),(#42057,#42058),(#42059,#42060),(#42061,
#42062),(#42063,#42064),(#42065,#42066),(#42067,#42068),(#42069,#42070),
(#42071,#42072),(#42073,#42074),(#42075,#42076),(#42077,#42078),(#42079,
#42080),(#42081,#42082),(#42083,#42084),(#42085,#42086),(#42087,#42088),
(#42089,#42090),(#42091,#42092),(#42093,#42094),(#42095,#42096),(#42097,
#42098),(#42099,#42100),(#42101,#42102),(#42103,#42104),(#42105,#42106),
(#42107,#42108),(#42109,#42110),(#42111,#42112),(#42113,#42114),(#42115,
#42116),(#42117,#42118),(#42119,#42120),(#42121,#42122),(#42123,#42124),
(#42125,#42126),(#42127,#42128),(#42129,#42130),(#42131,#42132),(#42133,
#42134),(#42135,#42136),(#42137,#42138),(#42139,#42140),(#42141,#42142),
(#42143,#42144),(#42145,#42146),(#42147,#42148),(#42149,#42150),(#42151,
#42152),(#42153,#42154),(#42155,#42156),(#42157,#42158),(#42159,#42160),
(#42161,#42162),(#42163,#42164),(#42165,#42166),(#42167,#42168),(#42169,
#42170),(#42171,#42172),(#42173,#42174),(#42175,#42176),(#42177,#42178),
(#42179,#42180),(#42181,#42182),(#42183,#42184),(#42185,#42186),(#42187,
#42188),(#42189,#42190),(#42191,#42192),(#42193,#42194),(#42195,#42196),
(#42197,#42198),(#42199,#42200),(#42201,#42202),(#42203,#42204),(#42205,
#42206),(#42207,#42208),(#42209,#42210),(#42211,#42212),(#42213,#42214),
(#42215,#42216),(#42217,#42218),(#42219,#42220),(#42221,#42222),(#42223,
#42224),(#42225,#42226),(#42227,#42228),(#42229,#42230),(#42231,#42232),
(#42233,#42234),(#42235,#42236),(#42237,#42238),(#42239,#42240),(#42241,
#42242),(#42243,#42244),(#42245,#42246),(#42247,#42248),(#42249,#42250),
(#42251,#42252),(#42253,#42254),(#42255,#42256),(#42257,#42258),(#42259,
#42260),(#42261,#42262),(#42263,#42264),(#42265,#42266),(#42267,#42268),
(#42269,#42270),(#42271,#42272),(#42273,#42274),(#42275,#42276),(#42277,
#42278),(#42279,#42280),(#42281,#42282),(#42283,#42284),(#42285,#42286),
(#42287,#42288),(#42289,#42290),(#42291,#42292),(#42293,#42294),(#42295,
#42296),(#42297,#42298),(#42299,#42300),(#42301,#42302),(#42303,#42304),
(#42305,#42306),(#42307,#42308),(#42309,#42310),(#42311,#42312),(#42313,
#42314),(#42315,#42316),(#42317,#42318),(#42319,#42320),(#42321,#42322),
(#42323,#42324),(#42325,#42326),(#42327,#42328),(#42329,#42330),(#42331,
#42332),(#42333,#42334),(#42335,#42336),(#42337,#42338),(#42339,#42340),
(#42341,#42342),(#42343,#42344),(#42345,#42346),(#42347,#42348),(#42349,
#42350),(#42351,#42352),(#42353,#42354),(#42355,#42356),(#42357,#42358),
(#42359,#42360),(#42361,#42362),(#42363,#42364),(#42365,#42366),(#42367,
#42368),(#42369,#42370),(#42371,#42372),(#42373,#42374),(#42375,#42376),
(#42377,#42378),(#42379,#42380),(#42381,#42382),(#42383,#42384),(#42385,
#42386),(#42387,#42388),(#42389,#42390),(#42391,#42392),(#42393,#42394),
(#42395,#42396),(#42397,#42398),(#42399,#42400),(#42401,#42402),(#42403,
#42404),(#42405,#42406),(#42407,#42408),(#42409,#42410),(#42411,#42412),
(#42413,#42414),(#42415,#42416),(#42417,#42418),(#42419,#42420),(#42421,
#42422),(#42423,#42424),(#42425,#42426),(#42427,#42428),(#42429,#42430),
(#42431,#42432),(#42433,#42434),(#42435,#42436),(#42437,#42438),(#42439,
#42440),(#42441,#42442),(#42443,#42444),(#42445,#42446),(#42447,#42448),
(#42449,#42450),(#42451,#42452),(#42453,#42454),(#42455,#42456),(#42457,
#42458),(#42459,#42460),(#42461,#42462),(#42463,#42464),(#42465,#42466),
(#42467,#42468),(#42469,#42470),(#42471,#42472),(#42473,#42474),(#42475,
#42476),(#42477,#42478),(#42479,#42480),(#42481,#42482),(#42483,#42484),
(#42485,#42486),(#42487,#42488),(#42489,#42490),(#42491,#42492),(#42493,
#42494),(#42495,#42496),(#42497,#42498),(#42499,#42500),(#42501,#42502),
(#42503,#42504),(#42505,#42506),(#42507,#42508),(#42509,#42510),(#42511,
#42512),(#42513,#42514),(#42515,#42516),(#42517,#42518),(#42519,#42520),
(#42521,#42522),(#42523,#42524),(#42525,#42526),(#42527,#42528),(#42529,
#42530),(#42531,#42532),(#42533,#42534),(#42535,#42536),(#42537,#42538),
(#42539,#42540),(#42541,#42542),(#42543,#42544),(#42545,#42546),(#42547,
#42548),(#42549,#42550),(#42551,#42552),(#42553,#42554),(#42555,#42556),
(#42557,#42558),(#42559,#42560),(#42561,#42562),(#42563,#42564),(#42565,
#42566),(#42567,#42568),(#42569,#42570),(#42571,#42572),(#42573,#42574),
(#42575,#42576),(#42577,#42578),(#42579,#42580),(#42581,#42582),(#42583,
#42584),(#42585,#42586)),.UNSPECIFIED.,.F.,.F.,.F.)
B_SPLINE_SURFACE_WITH_KNOTS((6,1,1,1,1,1,1,1,1,1,1,1,1,1,1,1,1,1,1,1,1,
1,1,1,1,1,1,1,1,1,1,1,1,1,1,1,1,1,1,1,1,1,1,1,1,1,1,1,1,1,1,1,1,1,1,1,1,
1,1,1,1,1,1,1,1,1,1,1,1,1,1,1,1,1,1,1,1,1,1,1,1,1,1,1,1,1,1,1,1,1,1,1,1,
1,1,1,1,1,1,1,1,1,1,1,1,1,1,1,1,1,1,1,1,1,1,1,1,1,1,1,1,1,1,1,1,1,1,1,1,
1,1,1,1,1,1,1,1,1,1,1,1,1,1,1,1,1,1,1,1,1,1,1,1,1,1,1,1,1,1,1,1,1,1,1,1,
1,1,1,1,1,1,1,1,1,1,1,1,1,1,1,1,1,1,1,1,1,1,1,1,1,1,1,1,1,1,1,1,1,1,1,1,
1,1,1,1,1,1,1,1,1,1,1,1,1,1,1,1,1,1,1,1,1,1,1,1,1,1,1,1,1,1,1,1,1,1,1,1,
1,1,1,1,1,1,1,1,1,1,1,1,1,1,1,1,1,1,1,1,1,1,1,1,1,1,1,1,1,1,1,1,1,1,1,1,
1,1,1,1,1,1,1,1,1,1,1,1,1,1,1,1,1,1,1,1,1,1,1,1,1,1,1,1,1,1,1,1,1,1,1,1,
1,1,1,1,1,1,1,1,1,1,1,1,1,1,1,1,1,1,1,1,1,1,1,1,1,1,1,1,1,1,1,1,1,1,1,1,
1,1,1,1,1,1,1,1,1,1,1,1,1,1,1,6),(2,2),(0.,0.00277777777777778,0.00555555555555556,
0.00833333333333333,0.0111111111111111,0.0138888888888889,0.0166666666666667,
0.0194444444444444,0.0222222222222222,0.025,0.0277777777777778,0.0305555555555556,
0.0333333333333333,0.0361111111111111,0.0388888888888889,0.0416666666666667,
0.0444444444444444,0.0472222222222222,0.05,0.0527777777777778,0.0555555555555555,
0.0583333333333333,0.0611111111111111,0.0638888888888889,0.0666666666666666,
0.0694444444444444,0.0722222222222222,0.075,0.0777777777777778,0.0805555555555555,
0.0833333333333333,0.0861111111111111,0.0888888888888889,0.0916666666666667,
0.0944444444444445,0.0972222222222222,0.1,0.102777777777778,0.105555555555556,
0.108333333333333,0.111111111111111,0.113888888888889,0.116666666666667,
0.119444444444444,0.122222222222222,0.125,0.127777777777778,0.130555555555556,
0.133333333333333,0.136111111111111,0.138888888888889,0.141666666666667,
0.144444444444444,0.147222222222222,0.15,0.152777777777778,0.155555555555556,
0.158333333333333,0.161111111111111,0.163888888888889,0.166666666666667,
0.169444444444444,0.172222222222222,0.175,0.177777777777778,0.180555555555555,
0.183333333333333,0.186111111111111,0.188888888888889,0.191666666666666,
0.194444444444444,0.197222222222222,0.2,0.202777777777778,0.205555555555555,
0.208333333333333,0.211111111111111,0.213888888888889,0.216666666666666,
0.219444444444444,0.222222222222222,0.225,0.227777777777777,0.230555555555555,
0.233333333333333,0.236111111111111,0.238888888888889,0.241666666666666,
0.244444444444444,0.247222222222222,0.25,0.252777777777777,0.255555555555555,
0.258333333333333,0.261111111111111,0.263888888888888,0.266666666666666,
0.269444444444444,0.272222222222222,0.275,0.277777777777777,0.280555555555555,
0.283333333333333,0.286111111111111,0.288888888888888,0.291666666666666,
0.294444444444444,0.297222222222222,0.299999999999999,0.302777777777777,
0.305555555555555,0.308333333333333,0.311111111111111,0.313888888888888,
0.316666666666666,0.319444444444444,0.322222222222222,0.324999999999999,
0.327777777777777,0.330555555555555,0.333333333333333,0.33611111111111,
0.338888888888888,0.341666666666666,0.344444444444444,0.347222222222221,
0.349999999999999,0.352777777777777,0.355555555555555,0.358333333333333,
0.36111111111111,0.363888888888888,0.366666666666666,0.369444444444444,
0.372222222222221,0.374999999999999,0.377777777777777,0.380555555555555,
0.383333333333332,0.38611111111111,0.388888888888888,0.391666666666666,
0.394444444444444,0.397222222222221,0.399999999999999,0.402777777777777,
0.405555555555555,0.408333333333332,0.41111111111111,0.413888888888888,
0.416666666666666,0.419444444444443,0.422222222222221,0.424999999999999,
0.427777777777777,0.430555555555555,0.433333333333332,0.43611111111111,
0.438888888888888,0.441666666666666,0.444444444444443,0.447222222222221,
0.449999999999999,0.452777777777777,0.455555555555554,0.458333333333332,
0.46111111111111,0.463888888888888,0.466666666666666,0.469444444444443,
0.472222222222221,0.474999999999999,0.477777777777777,0.480555555555554,
0.483333333333332,0.48611111111111,0.488888888888888,0.491666666666665,
0.494444444444443,0.497222222222221,0.499999999999999,0.502777777777777,
0.505555555555554,0.508333333333332,0.51111111111111,0.513888888888888,
0.516666666666665,0.519444444444443,0.522222222222221,0.524999999999999,
0.527777777777776,0.530555555555554,0.533333333333332,0.53611111111111,
0.538888888888888,0.541666666666665,0.544444444444443,0.547222222222221,
0.549999999999999,0.552777777777776,0.555555555555554,0.558333333333332,
0.56111111111111,0.563888888888887,0.566666666666665,0.569444444444443,
0.572222222222221,0.574999999999999,0.577777777777776,0.580555555555554,
0.583333333333332,0.58611111111111,0.588888888888887,0.591666666666665,
0.594444444444443,0.597222222222221,0.599999999999998,0.602777777777776,
0.605555555555554,0.608333333333332,0.611111111111109,0.613888888888887,
0.616666666666665,0.619444444444443,0.622222222222221,0.624999999999998,
0.627777777777776,0.630555555555554,0.633333333333332,0.636111111111109,
0.638888888888887,0.641666666666665,0.644444444444443,0.64722222222222,
0.649999999999998,0.652777777777776,0.655555555555554,0.658333333333332,
0.661111111111109,0.663888888888887,0.666666666666665,0.669444444444443,
0.67222222222222,0.674999999999998,0.677777777777776,0.680555555555554,
0.683333333333331,0.686111111111109,0.688888888888887,0.691666666666665,
0.694444444444443,0.69722222222222,0.699999999999998,0.702777777777776,
0.705555555555554,0.708333333333331,0.711111111111109,0.713888888888887,
0.716666666666665,0.719444444444442,0.72222222222222,0.724999999999998,
0.727777777777776,0.730555555555554,0.733333333333331,0.736111111111109,
0.738888888888887,0.741666666666665,0.744444444444442,0.74722222222222,
0.749999999999998,0.752777777777776,0.755555555555553,0.758333333333331,
0.761111111111109,0.763888888888887,0.766666666666664,0.769444444444442,
0.77222222222222,0.774999999999998,0.777777777777776,0.780555555555553,
0.783333333333331,0.786111111111109,0.788888888888887,0.791666666666664,
0.794444444444442,0.79722222222222,0.799999999999998,0.802777777777775,
0.805555555555553,0.808333333333331,0.811111111111109,0.813888888888887,
0.816666666666664,0.819444444444442,0.82222222222222,0.824999999999998,
0.827777777777775,0.830555555555553,0.833333333333331,0.836111111111109,
0.838888888888886,0.841666666666664,0.844444444444442,0.84722222222222,
0.849999999999998,0.852777777777775,0.855555555555553,0.858333333333331,
0.861111111111109,0.863888888888886,0.866666666666664,0.869444444444442,
0.87222222222222,0.874999999999997,0.877777777777775,0.880555555555553,
0.883333333333331,0.886111111111109,0.888888888888886,0.891666666666664,
0.894444444444442,0.89722222222222,0.899999999999997,0.902777777777775,
0.905555555555553,0.908333333333331,0.911111111111108,0.913888888888886,
0.916666666666664,0.919444444444442,0.92222222222222,0.924999999999997,
0.927777777777775,0.930555555555553,0.933333333333331,0.936111111111108,
0.938888888888886,0.941666666666664,0.944444444444442,0.947222222222219,
0.949999999999997,0.952777777777775,0.955555555555553,0.95833333333333,
0.961111111111108,0.963888888888886,0.966666666666664,0.969444444444442,
0.972222222222219,0.974999999999997,0.977777777777775,0.980555555555553,
0.98333333333333,0.986111111111108,0.988888888888886,0.991666666666664,
0.994444444444441,0.997222222222219,1.),(0.,0.15),.UNSPECIFIED.)
GEOMETRIC_REPRESENTATION_ITEM()
RATIONAL_B_SPLINE_SURFACE(((1.,1.),(1.,1.),(1.,1.),(1.,1.),(1.,1.),(1.,
1.),(1.,1.),(1.,1.),(1.,1.),(1.,1.),(1.,1.),(1.,1.),(1.,1.),(1.,1.),(1.,
1.),(1.,1.),(1.,1.),(1.,1.),(1.,1.),(1.,1.),(1.,1.),(1.,1.),(1.,1.),(1.,
1.),(1.,1.),(1.,1.),(1.,1.),(1.,1.),(1.,1.),(1.,1.),(1.,1.),(1.,1.),(1.,
1.),(1.,1.),(1.,1.),(1.,1.),(1.,1.),(1.,1.),(1.,1.),(1.,1.),(1.,1.),(1.,
1.),(1.,1.),(1.,1.),(1.,1.),(1.,1.),(1.,1.),(1.,1.),(1.,1.),(1.,1.),(1.,
1.),(1.,1.),(1.,1.),(1.,1.),(1.,1.),(1.,1.),(1.,1.),(1.,1.),(1.,1.),(1.,
1.),(1.,1.),(1.,1.),(1.,1.),(1.,1.),(1.,1.),(1.,1.),(1.,1.),(1.,1.),(1.,
1.),(1.,1.),(1.,1.),(1.,1.),(1.,1.),(1.,1.),(1.,1.),(1.,1.),(1.,1.),(1.,
1.),(1.,1.),(1.,1.),(1.,1.),(1.,1.),(1.,1.),(1.,1.),(1.,1.),(1.,1.),(1.,
1.),(1.,1.),(1.,1.),(1.,1.),(1.,1.),(1.,1.),(1.,1.),(1.,1.),(1.,1.),(1.,
1.),(1.,1.),(1.,1.),(1.,1.),(1.,1.),(1.,1.),(1.,1.),(1.,1.),(1.,1.),(1.,
1.),(1.,1.),(1.,1.),(1.,1.),(1.,1.),(1.,1.),(1.,1.),(1.,1.),(1.,1.),(1.,
1.),(1.,1.),(1.,1.),(1.,1.),(1.,1.),(1.,1.),(1.,1.),(1.,1.),(1.,1.),(1.,
1.),(1.,1.),(1.,1.),(1.,1.),(1.,1.),(1.,1.),(1.,1.),(1.,1.),(1.,1.),(1.,
1.),(1.,1.),(1.,1.),(1.,1.),(1.,1.),(1.,1.),(1.,1.),(1.,1.),(1.,1.),(1.,
1.),(1.,1.),(1.,1.),(1.,1.),(1.,1.),(1.,1.),(1.,1.),(1.,1.),(1.,1.),(1.,
1.),(1.,1.),(1.,1.),(1.,1.),(1.,1.),(1.,1.),(1.,1.),(1.,1.),(1.,1.),(1.,
1.),(1.,1.),(1.,1.),(1.,1.),(1.,1.),(1.,1.),(1.,1.),(1.,1.),(1.,1.),(1.,
1.),(1.,1.),(1.,1.),(1.,1.),(1.,1.),(1.,1.),(1.,1.),(1.,1.),(1.,1.),(1.,
1.),(1.,1.),(1.,1.),(1.,1.),(1.,1.),(1.,1.),(1.,1.),(1.,1.),(1.,1.),(1.,
1.),(1.,1.),(1.,1.),(1.,1.),(1.,1.),(1.,1.),(1.,1.),(1.,1.),(1.,1.),(1.,
1.),(1.,1.),(1.,1.),(1.,1.),(1.,1.),(1.,1.),(1.,1.),(1.,1.),(1.,1.),(1.,
1.),(1.,1.),(1.,1.),(1.,1.),(1.,1.),(1.,1.),(1.,1.),(1.,1.),(1.,1.),(1.,
1.),(1.,1.),(1.,1.),(1.,1.),(1.,1.),(1.,1.),(1.,1.),(1.,1.),(1.,1.),(1.,
1.),(1.,1.),(1.,1.),(1.,1.),(1.,1.),(1.,1.),(1.,1.),(1.,1.),(1.,1.),(1.,
1.),(1.,1.),(1.,1.),(1.,1.),(1.,1.),(1.,1.),(1.,1.),(1.,1.),(1.,1.),(1.,
1.),(1.,1.),(1.,1.),(1.,1.),(1.,1.),(1.,1.),(1.,1.),(1.,1.),(1.,1.),(1.,
1.),(1.,1.),(1.,1.),(1.,1.),(1.,1.),(1.,1.),(1.,1.),(1.,1.),(1.,1.),(1.,
1.),(1.,1.),(1.,1.),(1.,1.),(1.,1.),(1.,1.),(1.,1.),(1.,1.),(1.,1.),(1.,
1.),(1.,1.),(1.,1.),(1.,1.),(1.,1.),(1.,1.),(1.,1.),(1.,1.),(1.,1.),(1.,
1.),(1.,1.),(1.,1.),(1.,1.),(1.,1.),(1.,1.),(1.,1.),(1.,1.),(1.,1.),(1.,
1.),(1.,1.),(1.,1.),(1.,1.),(1.,1.),(1.,1.),(1.,1.),(1.,1.),(1.,1.),(1.,
1.),(1.,1.),(1.,1.),(1.,1.),(1.,1.),(1.,1.),(1.,1.),(1.,1.),(1.,1.),(1.,
1.),(1.,1.),(1.,1.),(1.,1.),(1.,1.),(1.,1.),(1.,1.),(1.,1.),(1.,1.),(1.,
1.),(1.,1.),(1.,1.),(1.,1.),(1.,1.),(1.,1.),(1.,1.),(1.,1.),(1.,1.),(1.,
1.),(1.,1.),(1.,1.),(1.,1.),(1.,1.),(1.,1.),(1.,1.),(1.,1.),(1.,1.),(1.,
1.),(1.,1.),(1.,1.),(1.,1.),(1.,1.),(1.,1.),(1.,1.),(1.,1.),(1.,1.),(1.,
1.),(1.,1.),(1.,1.),(1.,1.),(1.,1.),(1.,1.),(1.,1.),(1.,1.),(1.,1.),(1.,
1.),(1.,1.),(1.,1.),(1.,1.),(1.,1.),(1.,1.),(1.,1.),(1.,1.),(1.,1.),(1.,
1.),(1.,1.),(1.,1.),(1.,1.),(1.,1.),(1.,1.),(1.,1.),(1.,1.),(1.,1.)))
REPRESENTATION_ITEM('')
SURFACE()
);
#1079=(
BOUNDED_SURFACE()
B_SPLINE_SURFACE(5,1,((#42883,#42884),(#42885,#42886),(#42887,#42888),(#42889,
#42890),(#42891,#42892),(#42893,#42894),(#42895,#42896),(#42897,#42898),
(#42899,#42900),(#42901,#42902),(#42903,#42904),(#42905,#42906),(#42907,
#42908),(#42909,#42910),(#42911,#42912),(#42913,#42914),(#42915,#42916),
(#42917,#42918),(#42919,#42920),(#42921,#42922),(#42923,#42924),(#42925,
#42926),(#42927,#42928),(#42929,#42930),(#42931,#42932),(#42933,#42934),
(#42935,#42936),(#42937,#42938),(#42939,#42940),(#42941,#42942),(#42943,
#42944),(#42945,#42946),(#42947,#42948),(#42949,#42950),(#42951,#42952),
(#42953,#42954),(#42955,#42956),(#42957,#42958),(#42959,#42960),(#42961,
#42962),(#42963,#42964),(#42965,#42966),(#42967,#42968),(#42969,#42970),
(#42971,#42972),(#42973,#42974),(#42975,#42976),(#42977,#42978),(#42979,
#42980),(#42981,#42982),(#42983,#42984),(#42985,#42986),(#42987,#42988),
(#42989,#42990),(#42991,#42992),(#42993,#42994),(#42995,#42996),(#42997,
#42998),(#42999,#43000),(#43001,#43002),(#43003,#43004),(#43005,#43006),
(#43007,#43008),(#43009,#43010),(#43011,#43012),(#43013,#43014),(#43015,
#43016),(#43017,#43018),(#43019,#43020),(#43021,#43022),(#43023,#43024),
(#43025,#43026),(#43027,#43028),(#43029,#43030),(#43031,#43032),(#43033,
#43034),(#43035,#43036),(#43037,#43038),(#43039,#43040),(#43041,#43042),
(#43043,#43044),(#43045,#43046),(#43047,#43048),(#43049,#43050),(#43051,
#43052),(#43053,#43054),(#43055,#43056),(#43057,#43058),(#43059,#43060),
(#43061,#43062),(#43063,#43064),(#43065,#43066),(#43067,#43068),(#43069,
#43070),(#43071,#43072),(#43073,#43074),(#43075,#43076),(#43077,#43078),
(#43079,#43080),(#43081,#43082),(#43083,#43084),(#43085,#43086),(#43087,
#43088),(#43089,#43090),(#43091,#43092),(#43093,#43094),(#43095,#43096),
(#43097,#43098),(#43099,#43100),(#43101,#43102),(#43103,#43104),(#43105,
#43106),(#43107,#43108),(#43109,#43110),(#43111,#43112),(#43113,#43114),
(#43115,#43116),(#43117,#43118),(#43119,#43120),(#43121,#43122),(#43123,
#43124),(#43125,#43126),(#43127,#43128),(#43129,#43130),(#43131,#43132),
(#43133,#43134),(#43135,#43136),(#43137,#43138),(#43139,#43140),(#43141,
#43142),(#43143,#43144),(#43145,#43146),(#43147,#43148),(#43149,#43150),
(#43151,#43152),(#43153,#43154),(#43155,#43156),(#43157,#43158),(#43159,
#43160),(#43161,#43162),(#43163,#43164),(#43165,#43166),(#43167,#43168),
(#43169,#43170),(#43171,#43172),(#43173,#43174),(#43175,#43176),(#43177,
#43178),(#43179,#43180),(#43181,#43182),(#43183,#43184),(#43185,#43186),
(#43187,#43188),(#43189,#43190),(#43191,#43192),(#43193,#43194),(#43195,
#43196),(#43197,#43198),(#43199,#43200),(#43201,#43202),(#43203,#43204),
(#43205,#43206),(#43207,#43208),(#43209,#43210),(#43211,#43212),(#43213,
#43214),(#43215,#43216),(#43217,#43218),(#43219,#43220),(#43221,#43222),
(#43223,#43224),(#43225,#43226),(#43227,#43228),(#43229,#43230),(#43231,
#43232),(#43233,#43234),(#43235,#43236),(#43237,#43238),(#43239,#43240),
(#43241,#43242),(#43243,#43244),(#43245,#43246),(#43247,#43248),(#43249,
#43250),(#43251,#43252),(#43253,#43254),(#43255,#43256),(#43257,#43258),
(#43259,#43260),(#43261,#43262),(#43263,#43264),(#43265,#43266),(#43267,
#43268),(#43269,#43270),(#43271,#43272),(#43273,#43274),(#43275,#43276),
(#43277,#43278),(#43279,#43280),(#43281,#43282),(#43283,#43284),(#43285,
#43286),(#43287,#43288),(#43289,#43290),(#43291,#43292),(#43293,#43294),
(#43295,#43296),(#43297,#43298),(#43299,#43300),(#43301,#43302),(#43303,
#43304),(#43305,#43306),(#43307,#43308),(#43309,#43310),(#43311,#43312),
(#43313,#43314),(#43315,#43316),(#43317,#43318),(#43319,#43320),(#43321,
#43322),(#43323,#43324),(#43325,#43326),(#43327,#43328),(#43329,#43330),
(#43331,#43332),(#43333,#43334),(#43335,#43336),(#43337,#43338),(#43339,
#43340),(#43341,#43342),(#43343,#43344),(#43345,#43346),(#43347,#43348),
(#43349,#43350),(#43351,#43352),(#43353,#43354),(#43355,#43356),(#43357,
#43358),(#43359,#43360),(#43361,#43362),(#43363,#43364),(#43365,#43366),
(#43367,#43368),(#43369,#43370),(#43371,#43372),(#43373,#43374),(#43375,
#43376),(#43377,#43378),(#43379,#43380),(#43381,#43382),(#43383,#43384),
(#43385,#43386),(#43387,#43388),(#43389,#43390),(#43391,#43392),(#43393,
#43394),(#43395,#43396),(#43397,#43398),(#43399,#43400),(#43401,#43402),
(#43403,#43404),(#43405,#43406),(#43407,#43408),(#43409,#43410),(#43411,
#43412),(#43413,#43414),(#43415,#43416),(#43417,#43418),(#43419,#43420),
(#43421,#43422),(#43423,#43424),(#43425,#43426),(#43427,#43428),(#43429,
#43430),(#43431,#43432),(#43433,#43434),(#43435,#43436),(#43437,#43438),
(#43439,#43440),(#43441,#43442),(#43443,#43444),(#43445,#43446),(#43447,
#43448),(#43449,#43450),(#43451,#43452),(#43453,#43454),(#43455,#43456),
(#43457,#43458),(#43459,#43460),(#43461,#43462),(#43463,#43464),(#43465,
#43466),(#43467,#43468),(#43469,#43470),(#43471,#43472),(#43473,#43474),
(#43475,#43476),(#43477,#43478),(#43479,#43480),(#43481,#43482),(#43483,
#43484),(#43485,#43486),(#43487,#43488),(#43489,#43490),(#43491,#43492),
(#43493,#43494),(#43495,#43496),(#43497,#43498),(#43499,#43500),(#43501,
#43502),(#43503,#43504),(#43505,#43506),(#43507,#43508),(#43509,#43510),
(#43511,#43512),(#43513,#43514),(#43515,#43516),(#43517,#43518),(#43519,
#43520),(#43521,#43522),(#43523,#43524),(#43525,#43526),(#43527,#43528),
(#43529,#43530),(#43531,#43532),(#43533,#43534),(#43535,#43536),(#43537,
#43538),(#43539,#43540),(#43541,#43542),(#43543,#43544),(#43545,#43546),
(#43547,#43548),(#43549,#43550),(#43551,#43552),(#43553,#43554),(#43555,
#43556),(#43557,#43558),(#43559,#43560),(#43561,#43562),(#43563,#43564),
(#43565,#43566),(#43567,#43568),(#43569,#43570),(#43571,#43572),(#43573,
#43574),(#43575,#43576),(#43577,#43578),(#43579,#43580),(#43581,#43582),
(#43583,#43584),(#43585,#43586),(#43587,#43588),(#43589,#43590),(#43591,
#43592),(#43593,#43594),(#43595,#43596),(#43597,#43598),(#43599,#43600),
(#43601,#43602),(#43603,#43604),(#43605,#43606),(#43607,#43608),(#43609,
#43610),(#43611,#43612)),.UNSPECIFIED.,.F.,.F.,.F.)
B_SPLINE_SURFACE_WITH_KNOTS((6,1,1,1,1,1,1,1,1,1,1,1,1,1,1,1,1,1,1,1,1,
1,1,1,1,1,1,1,1,1,1,1,1,1,1,1,1,1,1,1,1,1,1,1,1,1,1,1,1,1,1,1,1,1,1,1,1,
1,1,1,1,1,1,1,1,1,1,1,1,1,1,1,1,1,1,1,1,1,1,1,1,1,1,1,1,1,1,1,1,1,1,1,1,
1,1,1,1,1,1,1,1,1,1,1,1,1,1,1,1,1,1,1,1,1,1,1,1,1,1,1,1,1,1,1,1,1,1,1,1,
1,1,1,1,1,1,1,1,1,1,1,1,1,1,1,1,1,1,1,1,1,1,1,1,1,1,1,1,1,1,1,1,1,1,1,1,
1,1,1,1,1,1,1,1,1,1,1,1,1,1,1,1,1,1,1,1,1,1,1,1,1,1,1,1,1,1,1,1,1,1,1,1,
1,1,1,1,1,1,1,1,1,1,1,1,1,1,1,1,1,1,1,1,1,1,1,1,1,1,1,1,1,1,1,1,1,1,1,1,
1,1,1,1,1,1,1,1,1,1,1,1,1,1,1,1,1,1,1,1,1,1,1,1,1,1,1,1,1,1,1,1,1,1,1,1,
1,1,1,1,1,1,1,1,1,1,1,1,1,1,1,1,1,1,1,1,1,1,1,1,1,1,1,1,1,1,1,1,1,1,1,1,
1,1,1,1,1,1,1,1,1,1,1,1,1,1,1,1,1,1,1,1,1,1,1,1,1,1,1,1,1,1,1,1,1,1,1,1,
1,1,1,1,1,1,1,1,1,1,1,1,1,1,1,6),(2,2),(0.,0.00277777777777778,0.00555555555555556,
0.00833333333333333,0.0111111111111111,0.0138888888888889,0.0166666666666667,
0.0194444444444444,0.0222222222222222,0.025,0.0277777777777778,0.0305555555555556,
0.0333333333333333,0.0361111111111111,0.0388888888888889,0.0416666666666667,
0.0444444444444444,0.0472222222222222,0.05,0.0527777777777778,0.0555555555555555,
0.0583333333333333,0.0611111111111111,0.0638888888888889,0.0666666666666666,
0.0694444444444444,0.0722222222222222,0.075,0.0777777777777778,0.0805555555555555,
0.0833333333333333,0.0861111111111111,0.0888888888888889,0.0916666666666667,
0.0944444444444445,0.0972222222222222,0.1,0.102777777777778,0.105555555555556,
0.108333333333333,0.111111111111111,0.113888888888889,0.116666666666667,
0.119444444444444,0.122222222222222,0.125,0.127777777777778,0.130555555555556,
0.133333333333333,0.136111111111111,0.138888888888889,0.141666666666667,
0.144444444444444,0.147222222222222,0.15,0.152777777777778,0.155555555555556,
0.158333333333333,0.161111111111111,0.163888888888889,0.166666666666667,
0.169444444444444,0.172222222222222,0.175,0.177777777777778,0.180555555555555,
0.183333333333333,0.186111111111111,0.188888888888889,0.191666666666666,
0.194444444444444,0.197222222222222,0.2,0.202777777777778,0.205555555555555,
0.208333333333333,0.211111111111111,0.213888888888889,0.216666666666666,
0.219444444444444,0.222222222222222,0.225,0.227777777777777,0.230555555555555,
0.233333333333333,0.236111111111111,0.238888888888889,0.241666666666666,
0.244444444444444,0.247222222222222,0.25,0.252777777777777,0.255555555555555,
0.258333333333333,0.261111111111111,0.263888888888888,0.266666666666666,
0.269444444444444,0.272222222222222,0.275,0.277777777777777,0.280555555555555,
0.283333333333333,0.286111111111111,0.288888888888888,0.291666666666666,
0.294444444444444,0.297222222222222,0.299999999999999,0.302777777777777,
0.305555555555555,0.308333333333333,0.311111111111111,0.313888888888888,
0.316666666666666,0.319444444444444,0.322222222222222,0.324999999999999,
0.327777777777777,0.330555555555555,0.333333333333333,0.33611111111111,
0.338888888888888,0.341666666666666,0.344444444444444,0.347222222222221,
0.349999999999999,0.352777777777777,0.355555555555555,0.358333333333333,
0.36111111111111,0.363888888888888,0.366666666666666,0.369444444444444,
0.372222222222221,0.374999999999999,0.377777777777777,0.380555555555555,
0.383333333333332,0.38611111111111,0.388888888888888,0.391666666666666,
0.394444444444444,0.397222222222221,0.399999999999999,0.402777777777777,
0.405555555555555,0.408333333333332,0.41111111111111,0.413888888888888,
0.416666666666666,0.419444444444443,0.422222222222221,0.424999999999999,
0.427777777777777,0.430555555555555,0.433333333333332,0.43611111111111,
0.438888888888888,0.441666666666666,0.444444444444443,0.447222222222221,
0.449999999999999,0.452777777777777,0.455555555555554,0.458333333333332,
0.46111111111111,0.463888888888888,0.466666666666666,0.469444444444443,
0.472222222222221,0.474999999999999,0.477777777777777,0.480555555555554,
0.483333333333332,0.48611111111111,0.488888888888888,0.491666666666665,
0.494444444444443,0.497222222222221,0.499999999999999,0.502777777777777,
0.505555555555554,0.508333333333332,0.51111111111111,0.513888888888888,
0.516666666666665,0.519444444444443,0.522222222222221,0.524999999999999,
0.527777777777776,0.530555555555554,0.533333333333332,0.53611111111111,
0.538888888888888,0.541666666666665,0.544444444444443,0.547222222222221,
0.549999999999999,0.552777777777776,0.555555555555554,0.558333333333332,
0.56111111111111,0.563888888888887,0.566666666666665,0.569444444444443,
0.572222222222221,0.574999999999999,0.577777777777776,0.580555555555554,
0.583333333333332,0.58611111111111,0.588888888888887,0.591666666666665,
0.594444444444443,0.597222222222221,0.599999999999998,0.602777777777776,
0.605555555555554,0.608333333333332,0.611111111111109,0.613888888888887,
0.616666666666665,0.619444444444443,0.622222222222221,0.624999999999998,
0.627777777777776,0.630555555555554,0.633333333333332,0.636111111111109,
0.638888888888887,0.641666666666665,0.644444444444443,0.64722222222222,
0.649999999999998,0.652777777777776,0.655555555555554,0.658333333333332,
0.661111111111109,0.663888888888887,0.666666666666665,0.669444444444443,
0.67222222222222,0.674999999999998,0.677777777777776,0.680555555555554,
0.683333333333331,0.686111111111109,0.688888888888887,0.691666666666665,
0.694444444444443,0.69722222222222,0.699999999999998,0.702777777777776,
0.705555555555554,0.708333333333331,0.711111111111109,0.713888888888887,
0.716666666666665,0.719444444444442,0.72222222222222,0.724999999999998,
0.727777777777776,0.730555555555554,0.733333333333331,0.736111111111109,
0.738888888888887,0.741666666666665,0.744444444444442,0.74722222222222,
0.749999999999998,0.752777777777776,0.755555555555553,0.758333333333331,
0.761111111111109,0.763888888888887,0.766666666666664,0.769444444444442,
0.77222222222222,0.774999999999998,0.777777777777776,0.780555555555553,
0.783333333333331,0.786111111111109,0.788888888888887,0.791666666666664,
0.794444444444442,0.79722222222222,0.799999999999998,0.802777777777775,
0.805555555555553,0.808333333333331,0.811111111111109,0.813888888888887,
0.816666666666664,0.819444444444442,0.82222222222222,0.824999999999998,
0.827777777777775,0.830555555555553,0.833333333333331,0.836111111111109,
0.838888888888886,0.841666666666664,0.844444444444442,0.84722222222222,
0.849999999999998,0.852777777777775,0.855555555555553,0.858333333333331,
0.861111111111109,0.863888888888886,0.866666666666664,0.869444444444442,
0.87222222222222,0.874999999999997,0.877777777777775,0.880555555555553,
0.883333333333331,0.886111111111109,0.888888888888886,0.891666666666664,
0.894444444444442,0.89722222222222,0.899999999999997,0.902777777777775,
0.905555555555553,0.908333333333331,0.911111111111108,0.913888888888886,
0.916666666666664,0.919444444444442,0.92222222222222,0.924999999999997,
0.927777777777775,0.930555555555553,0.933333333333331,0.936111111111108,
0.938888888888886,0.941666666666664,0.944444444444442,0.947222222222219,
0.949999999999997,0.952777777777775,0.955555555555553,0.95833333333333,
0.961111111111108,0.963888888888886,0.966666666666664,0.969444444444442,
0.972222222222219,0.974999999999997,0.977777777777775,0.980555555555553,
0.98333333333333,0.986111111111108,0.988888888888886,0.991666666666664,
0.994444444444441,0.997222222222219,1.),(0.,0.15),.UNSPECIFIED.)
GEOMETRIC_REPRESENTATION_ITEM()
RATIONAL_B_SPLINE_SURFACE(((1.,1.),(1.,1.),(1.,1.),(1.,1.),(1.,1.),(1.,
1.),(1.,1.),(1.,1.),(1.,1.),(1.,1.),(1.,1.),(1.,1.),(1.,1.),(1.,1.),(1.,
1.),(1.,1.),(1.,1.),(1.,1.),(1.,1.),(1.,1.),(1.,1.),(1.,1.),(1.,1.),(1.,
1.),(1.,1.),(1.,1.),(1.,1.),(1.,1.),(1.,1.),(1.,1.),(1.,1.),(1.,1.),(1.,
1.),(1.,1.),(1.,1.),(1.,1.),(1.,1.),(1.,1.),(1.,1.),(1.,1.),(1.,1.),(1.,
1.),(1.,1.),(1.,1.),(1.,1.),(1.,1.),(1.,1.),(1.,1.),(1.,1.),(1.,1.),(1.,
1.),(1.,1.),(1.,1.),(1.,1.),(1.,1.),(1.,1.),(1.,1.),(1.,1.),(1.,1.),(1.,
1.),(1.,1.),(1.,1.),(1.,1.),(1.,1.),(1.,1.),(1.,1.),(1.,1.),(1.,1.),(1.,
1.),(1.,1.),(1.,1.),(1.,1.),(1.,1.),(1.,1.),(1.,1.),(1.,1.),(1.,1.),(1.,
1.),(1.,1.),(1.,1.),(1.,1.),(1.,1.),(1.,1.),(1.,1.),(1.,1.),(1.,1.),(1.,
1.),(1.,1.),(1.,1.),(1.,1.),(1.,1.),(1.,1.),(1.,1.),(1.,1.),(1.,1.),(1.,
1.),(1.,1.),(1.,1.),(1.,1.),(1.,1.),(1.,1.),(1.,1.),(1.,1.),(1.,1.),(1.,
1.),(1.,1.),(1.,1.),(1.,1.),(1.,1.),(1.,1.),(1.,1.),(1.,1.),(1.,1.),(1.,
1.),(1.,1.),(1.,1.),(1.,1.),(1.,1.),(1.,1.),(1.,1.),(1.,1.),(1.,1.),(1.,
1.),(1.,1.),(1.,1.),(1.,1.),(1.,1.),(1.,1.),(1.,1.),(1.,1.),(1.,1.),(1.,
1.),(1.,1.),(1.,1.),(1.,1.),(1.,1.),(1.,1.),(1.,1.),(1.,1.),(1.,1.),(1.,
1.),(1.,1.),(1.,1.),(1.,1.),(1.,1.),(1.,1.),(1.,1.),(1.,1.),(1.,1.),(1.,
1.),(1.,1.),(1.,1.),(1.,1.),(1.,1.),(1.,1.),(1.,1.),(1.,1.),(1.,1.),(1.,
1.),(1.,1.),(1.,1.),(1.,1.),(1.,1.),(1.,1.),(1.,1.),(1.,1.),(1.,1.),(1.,
1.),(1.,1.),(1.,1.),(1.,1.),(1.,1.),(1.,1.),(1.,1.),(1.,1.),(1.,1.),(1.,
1.),(1.,1.),(1.,1.),(1.,1.),(1.,1.),(1.,1.),(1.,1.),(1.,1.),(1.,1.),(1.,
1.),(1.,1.),(1.,1.),(1.,1.),(1.,1.),(1.,1.),(1.,1.),(1.,1.),(1.,1.),(1.,
1.),(1.,1.),(1.,1.),(1.,1.),(1.,1.),(1.,1.),(1.,1.),(1.,1.),(1.,1.),(1.,
1.),(1.,1.),(1.,1.),(1.,1.),(1.,1.),(1.,1.),(1.,1.),(1.,1.),(1.,1.),(1.,
1.),(1.,1.),(1.,1.),(1.,1.),(1.,1.),(1.,1.),(1.,1.),(1.,1.),(1.,1.),(1.,
1.),(1.,1.),(1.,1.),(1.,1.),(1.,1.),(1.,1.),(1.,1.),(1.,1.),(1.,1.),(1.,
1.),(1.,1.),(1.,1.),(1.,1.),(1.,1.),(1.,1.),(1.,1.),(1.,1.),(1.,1.),(1.,
1.),(1.,1.),(1.,1.),(1.,1.),(1.,1.),(1.,1.),(1.,1.),(1.,1.),(1.,1.),(1.,
1.),(1.,1.),(1.,1.),(1.,1.),(1.,1.),(1.,1.),(1.,1.),(1.,1.),(1.,1.),(1.,
1.),(1.,1.),(1.,1.),(1.,1.),(1.,1.),(1.,1.),(1.,1.),(1.,1.),(1.,1.),(1.,
1.),(1.,1.),(1.,1.),(1.,1.),(1.,1.),(1.,1.),(1.,1.),(1.,1.),(1.,1.),(1.,
1.),(1.,1.),(1.,1.),(1.,1.),(1.,1.),(1.,1.),(1.,1.),(1.,1.),(1.,1.),(1.,
1.),(1.,1.),(1.,1.),(1.,1.),(1.,1.),(1.,1.),(1.,1.),(1.,1.),(1.,1.),(1.,
1.),(1.,1.),(1.,1.),(1.,1.),(1.,1.),(1.,1.),(1.,1.),(1.,1.),(1.,1.),(1.,
1.),(1.,1.),(1.,1.),(1.,1.),(1.,1.),(1.,1.),(1.,1.),(1.,1.),(1.,1.),(1.,
1.),(1.,1.),(1.,1.),(1.,1.),(1.,1.),(1.,1.),(1.,1.),(1.,1.),(1.,1.),(1.,
1.),(1.,1.),(1.,1.),(1.,1.),(1.,1.),(1.,1.),(1.,1.),(1.,1.),(1.,1.),(1.,
1.),(1.,1.),(1.,1.),(1.,1.),(1.,1.),(1.,1.),(1.,1.),(1.,1.),(1.,1.),(1.,
1.),(1.,1.),(1.,1.),(1.,1.),(1.,1.),(1.,1.),(1.,1.),(1.,1.),(1.,1.),(1.,
1.),(1.,1.),(1.,1.),(1.,1.),(1.,1.),(1.,1.),(1.,1.),(1.,1.),(1.,1.),(1.,
1.),(1.,1.),(1.,1.),(1.,1.),(1.,1.),(1.,1.),(1.,1.),(1.,1.),(1.,1.)))
REPRESENTATION_ITEM('')
SURFACE()
);
#1080=(
BOUNDED_SURFACE()
B_SPLINE_SURFACE(5,1,((#45196,#45197),(#45198,#45199),(#45200,#45201),(#45202,
#45203),(#45204,#45205),(#45206,#45207),(#45208,#45209),(#45210,#45211),
(#45212,#45213),(#45214,#45215),(#45216,#45217),(#45218,#45219),(#45220,
#45221),(#45222,#45223),(#45224,#45225),(#45226,#45227),(#45228,#45229),
(#45230,#45231),(#45232,#45233),(#45234,#45235),(#45236,#45237),(#45238,
#45239),(#45240,#45241),(#45242,#45243),(#45244,#45245),(#45246,#45247),
(#45248,#45249),(#45250,#45251),(#45252,#45253),(#45254,#45255),(#45256,
#45257),(#45258,#45259),(#45260,#45261),(#45262,#45263),(#45264,#45265),
(#45266,#45267),(#45268,#45269),(#45270,#45271),(#45272,#45273),(#45274,
#45275),(#45276,#45277),(#45278,#45279),(#45280,#45281),(#45282,#45283),
(#45284,#45285),(#45286,#45287),(#45288,#45289),(#45290,#45291),(#45292,
#45293),(#45294,#45295),(#45296,#45297),(#45298,#45299),(#45300,#45301),
(#45302,#45303),(#45304,#45305),(#45306,#45307),(#45308,#45309),(#45310,
#45311),(#45312,#45313),(#45314,#45315),(#45316,#45317),(#45318,#45319),
(#45320,#45321),(#45322,#45323),(#45324,#45325),(#45326,#45327),(#45328,
#45329),(#45330,#45331),(#45332,#45333),(#45334,#45335),(#45336,#45337),
(#45338,#45339),(#45340,#45341),(#45342,#45343),(#45344,#45345),(#45346,
#45347),(#45348,#45349),(#45350,#45351),(#45352,#45353),(#45354,#45355),
(#45356,#45357),(#45358,#45359),(#45360,#45361),(#45362,#45363),(#45364,
#45365),(#45366,#45367),(#45368,#45369),(#45370,#45371),(#45372,#45373),
(#45374,#45375),(#45376,#45377),(#45378,#45379),(#45380,#45381),(#45382,
#45383),(#45384,#45385),(#45386,#45387),(#45388,#45389),(#45390,#45391),
(#45392,#45393),(#45394,#45395),(#45396,#45397),(#45398,#45399),(#45400,
#45401),(#45402,#45403),(#45404,#45405),(#45406,#45407),(#45408,#45409),
(#45410,#45411),(#45412,#45413),(#45414,#45415),(#45416,#45417),(#45418,
#45419),(#45420,#45421),(#45422,#45423),(#45424,#45425),(#45426,#45427),
(#45428,#45429),(#45430,#45431),(#45432,#45433),(#45434,#45435),(#45436,
#45437),(#45438,#45439),(#45440,#45441),(#45442,#45443),(#45444,#45445),
(#45446,#45447),(#45448,#45449),(#45450,#45451),(#45452,#45453),(#45454,
#45455),(#45456,#45457),(#45458,#45459),(#45460,#45461),(#45462,#45463),
(#45464,#45465),(#45466,#45467),(#45468,#45469),(#45470,#45471),(#45472,
#45473),(#45474,#45475),(#45476,#45477),(#45478,#45479),(#45480,#45481),
(#45482,#45483),(#45484,#45485),(#45486,#45487),(#45488,#45489),(#45490,
#45491),(#45492,#45493),(#45494,#45495),(#45496,#45497),(#45498,#45499),
(#45500,#45501),(#45502,#45503),(#45504,#45505),(#45506,#45507),(#45508,
#45509),(#45510,#45511),(#45512,#45513),(#45514,#45515),(#45516,#45517),
(#45518,#45519),(#45520,#45521),(#45522,#45523),(#45524,#45525),(#45526,
#45527),(#45528,#45529),(#45530,#45531),(#45532,#45533),(#45534,#45535),
(#45536,#45537),(#45538,#45539),(#45540,#45541),(#45542,#45543),(#45544,
#45545),(#45546,#45547),(#45548,#45549),(#45550,#45551),(#45552,#45553),
(#45554,#45555),(#45556,#45557),(#45558,#45559),(#45560,#45561),(#45562,
#45563),(#45564,#45565),(#45566,#45567),(#45568,#45569),(#45570,#45571),
(#45572,#45573),(#45574,#45575),(#45576,#45577),(#45578,#45579),(#45580,
#45581),(#45582,#45583),(#45584,#45585),(#45586,#45587),(#45588,#45589),
(#45590,#45591),(#45592,#45593),(#45594,#45595),(#45596,#45597),(#45598,
#45599),(#45600,#45601),(#45602,#45603),(#45604,#45605),(#45606,#45607),
(#45608,#45609),(#45610,#45611),(#45612,#45613),(#45614,#45615),(#45616,
#45617),(#45618,#45619),(#45620,#45621),(#45622,#45623),(#45624,#45625),
(#45626,#45627),(#45628,#45629),(#45630,#45631),(#45632,#45633),(#45634,
#45635),(#45636,#45637),(#45638,#45639),(#45640,#45641),(#45642,#45643),
(#45644,#45645),(#45646,#45647),(#45648,#45649),(#45650,#45651),(#45652,
#45653),(#45654,#45655),(#45656,#45657),(#45658,#45659),(#45660,#45661),
(#45662,#45663),(#45664,#45665),(#45666,#45667),(#45668,#45669),(#45670,
#45671),(#45672,#45673),(#45674,#45675),(#45676,#45677),(#45678,#45679),
(#45680,#45681),(#45682,#45683),(#45684,#45685),(#45686,#45687),(#45688,
#45689),(#45690,#45691),(#45692,#45693),(#45694,#45695),(#45696,#45697),
(#45698,#45699),(#45700,#45701),(#45702,#45703),(#45704,#45705),(#45706,
#45707),(#45708,#45709),(#45710,#45711),(#45712,#45713),(#45714,#45715),
(#45716,#45717),(#45718,#45719),(#45720,#45721),(#45722,#45723),(#45724,
#45725),(#45726,#45727),(#45728,#45729),(#45730,#45731),(#45732,#45733),
(#45734,#45735),(#45736,#45737),(#45738,#45739),(#45740,#45741),(#45742,
#45743),(#45744,#45745),(#45746,#45747),(#45748,#45749),(#45750,#45751),
(#45752,#45753),(#45754,#45755),(#45756,#45757),(#45758,#45759),(#45760,
#45761),(#45762,#45763),(#45764,#45765),(#45766,#45767),(#45768,#45769),
(#45770,#45771),(#45772,#45773),(#45774,#45775),(#45776,#45777),(#45778,
#45779),(#45780,#45781),(#45782,#45783),(#45784,#45785),(#45786,#45787),
(#45788,#45789),(#45790,#45791),(#45792,#45793),(#45794,#45795),(#45796,
#45797),(#45798,#45799),(#45800,#45801),(#45802,#45803),(#45804,#45805),
(#45806,#45807),(#45808,#45809),(#45810,#45811),(#45812,#45813),(#45814,
#45815),(#45816,#45817),(#45818,#45819),(#45820,#45821),(#45822,#45823),
(#45824,#45825),(#45826,#45827),(#45828,#45829),(#45830,#45831),(#45832,
#45833),(#45834,#45835),(#45836,#45837),(#45838,#45839),(#45840,#45841),
(#45842,#45843),(#45844,#45845),(#45846,#45847),(#45848,#45849),(#45850,
#45851),(#45852,#45853),(#45854,#45855),(#45856,#45857),(#45858,#45859),
(#45860,#45861),(#45862,#45863),(#45864,#45865),(#45866,#45867),(#45868,
#45869),(#45870,#45871),(#45872,#45873),(#45874,#45875),(#45876,#45877),
(#45878,#45879),(#45880,#45881),(#45882,#45883),(#45884,#45885),(#45886,
#45887),(#45888,#45889),(#45890,#45891),(#45892,#45893),(#45894,#45895),
(#45896,#45897),(#45898,#45899),(#45900,#45901),(#45902,#45903),(#45904,
#45905),(#45906,#45907),(#45908,#45909),(#45910,#45911),(#45912,#45913),
(#45914,#45915),(#45916,#45917),(#45918,#45919),(#45920,#45921),(#45922,
#45923),(#45924,#45925)),.UNSPECIFIED.,.F.,.F.,.F.)
B_SPLINE_SURFACE_WITH_KNOTS((6,1,1,1,1,1,1,1,1,1,1,1,1,1,1,1,1,1,1,1,1,
1,1,1,1,1,1,1,1,1,1,1,1,1,1,1,1,1,1,1,1,1,1,1,1,1,1,1,1,1,1,1,1,1,1,1,1,
1,1,1,1,1,1,1,1,1,1,1,1,1,1,1,1,1,1,1,1,1,1,1,1,1,1,1,1,1,1,1,1,1,1,1,1,
1,1,1,1,1,1,1,1,1,1,1,1,1,1,1,1,1,1,1,1,1,1,1,1,1,1,1,1,1,1,1,1,1,1,1,1,
1,1,1,1,1,1,1,1,1,1,1,1,1,1,1,1,1,1,1,1,1,1,1,1,1,1,1,1,1,1,1,1,1,1,1,1,
1,1,1,1,1,1,1,1,1,1,1,1,1,1,1,1,1,1,1,1,1,1,1,1,1,1,1,1,1,1,1,1,1,1,1,1,
1,1,1,1,1,1,1,1,1,1,1,1,1,1,1,1,1,1,1,1,1,1,1,1,1,1,1,1,1,1,1,1,1,1,1,1,
1,1,1,1,1,1,1,1,1,1,1,1,1,1,1,1,1,1,1,1,1,1,1,1,1,1,1,1,1,1,1,1,1,1,1,1,
1,1,1,1,1,1,1,1,1,1,1,1,1,1,1,1,1,1,1,1,1,1,1,1,1,1,1,1,1,1,1,1,1,1,1,1,
1,1,1,1,1,1,1,1,1,1,1,1,1,1,1,1,1,1,1,1,1,1,1,1,1,1,1,1,1,1,1,1,1,1,1,1,
1,1,1,1,1,1,1,1,1,1,1,1,1,1,1,6),(2,2),(0.,0.00277777777777778,0.00555555555555556,
0.00833333333333333,0.0111111111111111,0.0138888888888889,0.0166666666666667,
0.0194444444444444,0.0222222222222222,0.025,0.0277777777777778,0.0305555555555556,
0.0333333333333333,0.0361111111111111,0.0388888888888889,0.0416666666666667,
0.0444444444444444,0.0472222222222222,0.05,0.0527777777777778,0.0555555555555555,
0.0583333333333333,0.0611111111111111,0.0638888888888889,0.0666666666666666,
0.0694444444444444,0.0722222222222222,0.075,0.0777777777777778,0.0805555555555555,
0.0833333333333333,0.0861111111111111,0.0888888888888889,0.0916666666666667,
0.0944444444444445,0.0972222222222222,0.1,0.102777777777778,0.105555555555556,
0.108333333333333,0.111111111111111,0.113888888888889,0.116666666666667,
0.119444444444444,0.122222222222222,0.125,0.127777777777778,0.130555555555556,
0.133333333333333,0.136111111111111,0.138888888888889,0.141666666666667,
0.144444444444444,0.147222222222222,0.15,0.152777777777778,0.155555555555556,
0.158333333333333,0.161111111111111,0.163888888888889,0.166666666666667,
0.169444444444444,0.172222222222222,0.175,0.177777777777778,0.180555555555555,
0.183333333333333,0.186111111111111,0.188888888888889,0.191666666666666,
0.194444444444444,0.197222222222222,0.2,0.202777777777778,0.205555555555555,
0.208333333333333,0.211111111111111,0.213888888888889,0.216666666666666,
0.219444444444444,0.222222222222222,0.225,0.227777777777777,0.230555555555555,
0.233333333333333,0.236111111111111,0.238888888888889,0.241666666666666,
0.244444444444444,0.247222222222222,0.25,0.252777777777777,0.255555555555555,
0.258333333333333,0.261111111111111,0.263888888888888,0.266666666666666,
0.269444444444444,0.272222222222222,0.275,0.277777777777777,0.280555555555555,
0.283333333333333,0.286111111111111,0.288888888888888,0.291666666666666,
0.294444444444444,0.297222222222222,0.299999999999999,0.302777777777777,
0.305555555555555,0.308333333333333,0.311111111111111,0.313888888888888,
0.316666666666666,0.319444444444444,0.322222222222222,0.324999999999999,
0.327777777777777,0.330555555555555,0.333333333333333,0.33611111111111,
0.338888888888888,0.341666666666666,0.344444444444444,0.347222222222221,
0.349999999999999,0.352777777777777,0.355555555555555,0.358333333333333,
0.36111111111111,0.363888888888888,0.366666666666666,0.369444444444444,
0.372222222222221,0.374999999999999,0.377777777777777,0.380555555555555,
0.383333333333332,0.38611111111111,0.388888888888888,0.391666666666666,
0.394444444444444,0.397222222222221,0.399999999999999,0.402777777777777,
0.405555555555555,0.408333333333332,0.41111111111111,0.413888888888888,
0.416666666666666,0.419444444444443,0.422222222222221,0.424999999999999,
0.427777777777777,0.430555555555555,0.433333333333332,0.43611111111111,
0.438888888888888,0.441666666666666,0.444444444444443,0.447222222222221,
0.449999999999999,0.452777777777777,0.455555555555554,0.458333333333332,
0.46111111111111,0.463888888888888,0.466666666666666,0.469444444444443,
0.472222222222221,0.474999999999999,0.477777777777777,0.480555555555554,
0.483333333333332,0.48611111111111,0.488888888888888,0.491666666666665,
0.494444444444443,0.497222222222221,0.499999999999999,0.502777777777777,
0.505555555555554,0.508333333333332,0.51111111111111,0.513888888888888,
0.516666666666665,0.519444444444443,0.522222222222221,0.524999999999999,
0.527777777777776,0.530555555555554,0.533333333333332,0.53611111111111,
0.538888888888888,0.541666666666665,0.544444444444443,0.547222222222221,
0.549999999999999,0.552777777777776,0.555555555555554,0.558333333333332,
0.56111111111111,0.563888888888887,0.566666666666665,0.569444444444443,
0.572222222222221,0.574999999999999,0.577777777777776,0.580555555555554,
0.583333333333332,0.58611111111111,0.588888888888887,0.591666666666665,
0.594444444444443,0.597222222222221,0.599999999999998,0.602777777777776,
0.605555555555554,0.608333333333332,0.611111111111109,0.613888888888887,
0.616666666666665,0.619444444444443,0.622222222222221,0.624999999999998,
0.627777777777776,0.630555555555554,0.633333333333332,0.636111111111109,
0.638888888888887,0.641666666666665,0.644444444444443,0.64722222222222,
0.649999999999998,0.652777777777776,0.655555555555554,0.658333333333332,
0.661111111111109,0.663888888888887,0.666666666666665,0.669444444444443,
0.67222222222222,0.674999999999998,0.677777777777776,0.680555555555554,
0.683333333333331,0.686111111111109,0.688888888888887,0.691666666666665,
0.694444444444443,0.69722222222222,0.699999999999998,0.702777777777776,
0.705555555555554,0.708333333333331,0.711111111111109,0.713888888888887,
0.716666666666665,0.719444444444442,0.72222222222222,0.724999999999998,
0.727777777777776,0.730555555555554,0.733333333333331,0.736111111111109,
0.738888888888887,0.741666666666665,0.744444444444442,0.74722222222222,
0.749999999999998,0.752777777777776,0.755555555555553,0.758333333333331,
0.761111111111109,0.763888888888887,0.766666666666664,0.769444444444442,
0.77222222222222,0.774999999999998,0.777777777777776,0.780555555555553,
0.783333333333331,0.786111111111109,0.788888888888887,0.791666666666664,
0.794444444444442,0.79722222222222,0.799999999999998,0.802777777777775,
0.805555555555553,0.808333333333331,0.811111111111109,0.813888888888887,
0.816666666666664,0.819444444444442,0.82222222222222,0.824999999999998,
0.827777777777775,0.830555555555553,0.833333333333331,0.836111111111109,
0.838888888888886,0.841666666666664,0.844444444444442,0.84722222222222,
0.849999999999998,0.852777777777775,0.855555555555553,0.858333333333331,
0.861111111111109,0.863888888888886,0.866666666666664,0.869444444444442,
0.87222222222222,0.874999999999997,0.877777777777775,0.880555555555553,
0.883333333333331,0.886111111111109,0.888888888888886,0.891666666666664,
0.894444444444442,0.89722222222222,0.899999999999997,0.902777777777775,
0.905555555555553,0.908333333333331,0.911111111111108,0.913888888888886,
0.916666666666664,0.919444444444442,0.92222222222222,0.924999999999997,
0.927777777777775,0.930555555555553,0.933333333333331,0.936111111111108,
0.938888888888886,0.941666666666664,0.944444444444442,0.947222222222219,
0.949999999999997,0.952777777777775,0.955555555555553,0.95833333333333,
0.961111111111108,0.963888888888886,0.966666666666664,0.969444444444442,
0.972222222222219,0.974999999999997,0.977777777777775,0.980555555555553,
0.98333333333333,0.986111111111108,0.988888888888886,0.991666666666664,
0.994444444444441,0.997222222222219,1.),(0.,0.15),.UNSPECIFIED.)
GEOMETRIC_REPRESENTATION_ITEM()
RATIONAL_B_SPLINE_SURFACE(((1.,1.),(1.,1.),(1.,1.),(1.,1.),(1.,1.),(1.,
1.),(1.,1.),(1.,1.),(1.,1.),(1.,1.),(1.,1.),(1.,1.),(1.,1.),(1.,1.),(1.,
1.),(1.,1.),(1.,1.),(1.,1.),(1.,1.),(1.,1.),(1.,1.),(1.,1.),(1.,1.),(1.,
1.),(1.,1.),(1.,1.),(1.,1.),(1.,1.),(1.,1.),(1.,1.),(1.,1.),(1.,1.),(1.,
1.),(1.,1.),(1.,1.),(1.,1.),(1.,1.),(1.,1.),(1.,1.),(1.,1.),(1.,1.),(1.,
1.),(1.,1.),(1.,1.),(1.,1.),(1.,1.),(1.,1.),(1.,1.),(1.,1.),(1.,1.),(1.,
1.),(1.,1.),(1.,1.),(1.,1.),(1.,1.),(1.,1.),(1.,1.),(1.,1.),(1.,1.),(1.,
1.),(1.,1.),(1.,1.),(1.,1.),(1.,1.),(1.,1.),(1.,1.),(1.,1.),(1.,1.),(1.,
1.),(1.,1.),(1.,1.),(1.,1.),(1.,1.),(1.,1.),(1.,1.),(1.,1.),(1.,1.),(1.,
1.),(1.,1.),(1.,1.),(1.,1.),(1.,1.),(1.,1.),(1.,1.),(1.,1.),(1.,1.),(1.,
1.),(1.,1.),(1.,1.),(1.,1.),(1.,1.),(1.,1.),(1.,1.),(1.,1.),(1.,1.),(1.,
1.),(1.,1.),(1.,1.),(1.,1.),(1.,1.),(1.,1.),(1.,1.),(1.,1.),(1.,1.),(1.,
1.),(1.,1.),(1.,1.),(1.,1.),(1.,1.),(1.,1.),(1.,1.),(1.,1.),(1.,1.),(1.,
1.),(1.,1.),(1.,1.),(1.,1.),(1.,1.),(1.,1.),(1.,1.),(1.,1.),(1.,1.),(1.,
1.),(1.,1.),(1.,1.),(1.,1.),(1.,1.),(1.,1.),(1.,1.),(1.,1.),(1.,1.),(1.,
1.),(1.,1.),(1.,1.),(1.,1.),(1.,1.),(1.,1.),(1.,1.),(1.,1.),(1.,1.),(1.,
1.),(1.,1.),(1.,1.),(1.,1.),(1.,1.),(1.,1.),(1.,1.),(1.,1.),(1.,1.),(1.,
1.),(1.,1.),(1.,1.),(1.,1.),(1.,1.),(1.,1.),(1.,1.),(1.,1.),(1.,1.),(1.,
1.),(1.,1.),(1.,1.),(1.,1.),(1.,1.),(1.,1.),(1.,1.),(1.,1.),(1.,1.),(1.,
1.),(1.,1.),(1.,1.),(1.,1.),(1.,1.),(1.,1.),(1.,1.),(1.,1.),(1.,1.),(1.,
1.),(1.,1.),(1.,1.),(1.,1.),(1.,1.),(1.,1.),(1.,1.),(1.,1.),(1.,1.),(1.,
1.),(1.,1.),(1.,1.),(1.,1.),(1.,1.),(1.,1.),(1.,1.),(1.,1.),(1.,1.),(1.,
1.),(1.,1.),(1.,1.),(1.,1.),(1.,1.),(1.,1.),(1.,1.),(1.,1.),(1.,1.),(1.,
1.),(1.,1.),(1.,1.),(1.,1.),(1.,1.),(1.,1.),(1.,1.),(1.,1.),(1.,1.),(1.,
1.),(1.,1.),(1.,1.),(1.,1.),(1.,1.),(1.,1.),(1.,1.),(1.,1.),(1.,1.),(1.,
1.),(1.,1.),(1.,1.),(1.,1.),(1.,1.),(1.,1.),(1.,1.),(1.,1.),(1.,1.),(1.,
1.),(1.,1.),(1.,1.),(1.,1.),(1.,1.),(1.,1.),(1.,1.),(1.,1.),(1.,1.),(1.,
1.),(1.,1.),(1.,1.),(1.,1.),(1.,1.),(1.,1.),(1.,1.),(1.,1.),(1.,1.),(1.,
1.),(1.,1.),(1.,1.),(1.,1.),(1.,1.),(1.,1.),(1.,1.),(1.,1.),(1.,1.),(1.,
1.),(1.,1.),(1.,1.),(1.,1.),(1.,1.),(1.,1.),(1.,1.),(1.,1.),(1.,1.),(1.,
1.),(1.,1.),(1.,1.),(1.,1.),(1.,1.),(1.,1.),(1.,1.),(1.,1.),(1.,1.),(1.,
1.),(1.,1.),(1.,1.),(1.,1.),(1.,1.),(1.,1.),(1.,1.),(1.,1.),(1.,1.),(1.,
1.),(1.,1.),(1.,1.),(1.,1.),(1.,1.),(1.,1.),(1.,1.),(1.,1.),(1.,1.),(1.,
1.),(1.,1.),(1.,1.),(1.,1.),(1.,1.),(1.,1.),(1.,1.),(1.,1.),(1.,1.),(1.,
1.),(1.,1.),(1.,1.),(1.,1.),(1.,1.),(1.,1.),(1.,1.),(1.,1.),(1.,1.),(1.,
1.),(1.,1.),(1.,1.),(1.,1.),(1.,1.),(1.,1.),(1.,1.),(1.,1.),(1.,1.),(1.,
1.),(1.,1.),(1.,1.),(1.,1.),(1.,1.),(1.,1.),(1.,1.),(1.,1.),(1.,1.),(1.,
1.),(1.,1.),(1.,1.),(1.,1.),(1.,1.),(1.,1.),(1.,1.),(1.,1.),(1.,1.),(1.,
1.),(1.,1.),(1.,1.),(1.,1.),(1.,1.),(1.,1.),(1.,1.),(1.,1.),(1.,1.),(1.,
1.),(1.,1.),(1.,1.),(1.,1.),(1.,1.),(1.,1.),(1.,1.),(1.,1.),(1.,1.),(1.,
1.),(1.,1.),(1.,1.),(1.,1.),(1.,1.),(1.,1.),(1.,1.),(1.,1.),(1.,1.)))
REPRESENTATION_ITEM('')
SURFACE()
);
#1081=(
BOUNDED_SURFACE()
B_SPLINE_SURFACE(5,1,((#46179,#46180),(#46181,#46182),(#46183,#46184),(#46185,
#46186),(#46187,#46188),(#46189,#46190),(#46191,#46192),(#46193,#46194),
(#46195,#46196),(#46197,#46198),(#46199,#46200),(#46201,#46202),(#46203,
#46204),(#46205,#46206),(#46207,#46208),(#46209,#46210),(#46211,#46212),
(#46213,#46214),(#46215,#46216),(#46217,#46218),(#46219,#46220),(#46221,
#46222),(#46223,#46224),(#46225,#46226),(#46227,#46228),(#46229,#46230),
(#46231,#46232),(#46233,#46234),(#46235,#46236),(#46237,#46238),(#46239,
#46240),(#46241,#46242),(#46243,#46244),(#46245,#46246),(#46247,#46248),
(#46249,#46250),(#46251,#46252),(#46253,#46254),(#46255,#46256),(#46257,
#46258),(#46259,#46260),(#46261,#46262),(#46263,#46264),(#46265,#46266),
(#46267,#46268),(#46269,#46270),(#46271,#46272),(#46273,#46274),(#46275,
#46276),(#46277,#46278),(#46279,#46280),(#46281,#46282),(#46283,#46284),
(#46285,#46286),(#46287,#46288),(#46289,#46290),(#46291,#46292),(#46293,
#46294),(#46295,#46296),(#46297,#46298),(#46299,#46300),(#46301,#46302),
(#46303,#46304),(#46305,#46306),(#46307,#46308),(#46309,#46310),(#46311,
#46312),(#46313,#46314),(#46315,#46316),(#46317,#46318),(#46319,#46320),
(#46321,#46322),(#46323,#46324),(#46325,#46326),(#46327,#46328),(#46329,
#46330),(#46331,#46332),(#46333,#46334),(#46335,#46336),(#46337,#46338),
(#46339,#46340),(#46341,#46342),(#46343,#46344),(#46345,#46346),(#46347,
#46348),(#46349,#46350),(#46351,#46352),(#46353,#46354),(#46355,#46356),
(#46357,#46358),(#46359,#46360),(#46361,#46362),(#46363,#46364),(#46365,
#46366),(#46367,#46368),(#46369,#46370),(#46371,#46372),(#46373,#46374),
(#46375,#46376),(#46377,#46378),(#46379,#46380),(#46381,#46382),(#46383,
#46384),(#46385,#46386),(#46387,#46388),(#46389,#46390),(#46391,#46392),
(#46393,#46394),(#46395,#46396),(#46397,#46398),(#46399,#46400),(#46401,
#46402),(#46403,#46404),(#46405,#46406),(#46407,#46408),(#46409,#46410),
(#46411,#46412),(#46413,#46414),(#46415,#46416),(#46417,#46418),(#46419,
#46420),(#46421,#46422),(#46423,#46424),(#46425,#46426),(#46427,#46428),
(#46429,#46430),(#46431,#46432),(#46433,#46434),(#46435,#46436),(#46437,
#46438),(#46439,#46440),(#46441,#46442),(#46443,#46444),(#46445,#46446),
(#46447,#46448),(#46449,#46450),(#46451,#46452),(#46453,#46454),(#46455,
#46456),(#46457,#46458),(#46459,#46460),(#46461,#46462),(#46463,#46464),
(#46465,#46466),(#46467,#46468),(#46469,#46470),(#46471,#46472),(#46473,
#46474),(#46475,#46476),(#46477,#46478),(#46479,#46480),(#46481,#46482),
(#46483,#46484),(#46485,#46486),(#46487,#46488),(#46489,#46490),(#46491,
#46492),(#46493,#46494),(#46495,#46496),(#46497,#46498),(#46499,#46500),
(#46501,#46502),(#46503,#46504),(#46505,#46506),(#46507,#46508),(#46509,
#46510),(#46511,#46512),(#46513,#46514),(#46515,#46516),(#46517,#46518),
(#46519,#46520),(#46521,#46522),(#46523,#46524),(#46525,#46526),(#46527,
#46528),(#46529,#46530),(#46531,#46532),(#46533,#46534),(#46535,#46536),
(#46537,#46538),(#46539,#46540),(#46541,#46542),(#46543,#46544),(#46545,
#46546),(#46547,#46548),(#46549,#46550),(#46551,#46552),(#46553,#46554),
(#46555,#46556),(#46557,#46558),(#46559,#46560),(#46561,#46562),(#46563,
#46564),(#46565,#46566),(#46567,#46568),(#46569,#46570),(#46571,#46572),
(#46573,#46574),(#46575,#46576),(#46577,#46578),(#46579,#46580),(#46581,
#46582),(#46583,#46584),(#46585,#46586),(#46587,#46588),(#46589,#46590),
(#46591,#46592),(#46593,#46594),(#46595,#46596),(#46597,#46598),(#46599,
#46600),(#46601,#46602),(#46603,#46604),(#46605,#46606),(#46607,#46608),
(#46609,#46610),(#46611,#46612),(#46613,#46614),(#46615,#46616),(#46617,
#46618),(#46619,#46620),(#46621,#46622),(#46623,#46624),(#46625,#46626),
(#46627,#46628),(#46629,#46630),(#46631,#46632),(#46633,#46634),(#46635,
#46636),(#46637,#46638),(#46639,#46640),(#46641,#46642),(#46643,#46644),
(#46645,#46646),(#46647,#46648),(#46649,#46650),(#46651,#46652),(#46653,
#46654),(#46655,#46656),(#46657,#46658),(#46659,#46660),(#46661,#46662),
(#46663,#46664),(#46665,#46666),(#46667,#46668),(#46669,#46670),(#46671,
#46672),(#46673,#46674),(#46675,#46676),(#46677,#46678),(#46679,#46680),
(#46681,#46682),(#46683,#46684),(#46685,#46686),(#46687,#46688),(#46689,
#46690),(#46691,#46692),(#46693,#46694),(#46695,#46696),(#46697,#46698),
(#46699,#46700),(#46701,#46702),(#46703,#46704),(#46705,#46706),(#46707,
#46708),(#46709,#46710),(#46711,#46712),(#46713,#46714),(#46715,#46716),
(#46717,#46718),(#46719,#46720),(#46721,#46722),(#46723,#46724),(#46725,
#46726),(#46727,#46728),(#46729,#46730),(#46731,#46732),(#46733,#46734),
(#46735,#46736),(#46737,#46738),(#46739,#46740),(#46741,#46742),(#46743,
#46744),(#46745,#46746),(#46747,#46748),(#46749,#46750),(#46751,#46752),
(#46753,#46754),(#46755,#46756),(#46757,#46758),(#46759,#46760),(#46761,
#46762),(#46763,#46764),(#46765,#46766),(#46767,#46768),(#46769,#46770),
(#46771,#46772),(#46773,#46774),(#46775,#46776),(#46777,#46778),(#46779,
#46780),(#46781,#46782),(#46783,#46784),(#46785,#46786),(#46787,#46788),
(#46789,#46790),(#46791,#46792),(#46793,#46794),(#46795,#46796),(#46797,
#46798),(#46799,#46800),(#46801,#46802),(#46803,#46804),(#46805,#46806),
(#46807,#46808),(#46809,#46810),(#46811,#46812),(#46813,#46814),(#46815,
#46816),(#46817,#46818),(#46819,#46820),(#46821,#46822),(#46823,#46824),
(#46825,#46826),(#46827,#46828),(#46829,#46830),(#46831,#46832),(#46833,
#46834),(#46835,#46836),(#46837,#46838),(#46839,#46840),(#46841,#46842),
(#46843,#46844),(#46845,#46846),(#46847,#46848),(#46849,#46850),(#46851,
#46852),(#46853,#46854),(#46855,#46856),(#46857,#46858),(#46859,#46860),
(#46861,#46862),(#46863,#46864),(#46865,#46866),(#46867,#46868),(#46869,
#46870),(#46871,#46872),(#46873,#46874),(#46875,#46876),(#46877,#46878),
(#46879,#46880),(#46881,#46882),(#46883,#46884),(#46885,#46886),(#46887,
#46888),(#46889,#46890),(#46891,#46892),(#46893,#46894),(#46895,#46896),
(#46897,#46898),(#46899,#46900),(#46901,#46902),(#46903,#46904),(#46905,
#46906),(#46907,#46908)),.UNSPECIFIED.,.F.,.F.,.F.)
B_SPLINE_SURFACE_WITH_KNOTS((6,1,1,1,1,1,1,1,1,1,1,1,1,1,1,1,1,1,1,1,1,
1,1,1,1,1,1,1,1,1,1,1,1,1,1,1,1,1,1,1,1,1,1,1,1,1,1,1,1,1,1,1,1,1,1,1,1,
1,1,1,1,1,1,1,1,1,1,1,1,1,1,1,1,1,1,1,1,1,1,1,1,1,1,1,1,1,1,1,1,1,1,1,1,
1,1,1,1,1,1,1,1,1,1,1,1,1,1,1,1,1,1,1,1,1,1,1,1,1,1,1,1,1,1,1,1,1,1,1,1,
1,1,1,1,1,1,1,1,1,1,1,1,1,1,1,1,1,1,1,1,1,1,1,1,1,1,1,1,1,1,1,1,1,1,1,1,
1,1,1,1,1,1,1,1,1,1,1,1,1,1,1,1,1,1,1,1,1,1,1,1,1,1,1,1,1,1,1,1,1,1,1,1,
1,1,1,1,1,1,1,1,1,1,1,1,1,1,1,1,1,1,1,1,1,1,1,1,1,1,1,1,1,1,1,1,1,1,1,1,
1,1,1,1,1,1,1,1,1,1,1,1,1,1,1,1,1,1,1,1,1,1,1,1,1,1,1,1,1,1,1,1,1,1,1,1,
1,1,1,1,1,1,1,1,1,1,1,1,1,1,1,1,1,1,1,1,1,1,1,1,1,1,1,1,1,1,1,1,1,1,1,1,
1,1,1,1,1,1,1,1,1,1,1,1,1,1,1,1,1,1,1,1,1,1,1,1,1,1,1,1,1,1,1,1,1,1,1,1,
1,1,1,1,1,1,1,1,1,1,1,1,1,1,1,6),(2,2),(0.,0.00277777777777778,0.00555555555555556,
0.00833333333333333,0.0111111111111111,0.0138888888888889,0.0166666666666667,
0.0194444444444444,0.0222222222222222,0.025,0.0277777777777778,0.0305555555555556,
0.0333333333333333,0.0361111111111111,0.0388888888888889,0.0416666666666667,
0.0444444444444444,0.0472222222222222,0.05,0.0527777777777778,0.0555555555555555,
0.0583333333333333,0.0611111111111111,0.0638888888888889,0.0666666666666666,
0.0694444444444444,0.0722222222222222,0.075,0.0777777777777778,0.0805555555555555,
0.0833333333333333,0.0861111111111111,0.0888888888888889,0.0916666666666667,
0.0944444444444445,0.0972222222222222,0.1,0.102777777777778,0.105555555555556,
0.108333333333333,0.111111111111111,0.113888888888889,0.116666666666667,
0.119444444444444,0.122222222222222,0.125,0.127777777777778,0.130555555555556,
0.133333333333333,0.136111111111111,0.138888888888889,0.141666666666667,
0.144444444444444,0.147222222222222,0.15,0.152777777777778,0.155555555555556,
0.158333333333333,0.161111111111111,0.163888888888889,0.166666666666667,
0.169444444444444,0.172222222222222,0.175,0.177777777777778,0.180555555555555,
0.183333333333333,0.186111111111111,0.188888888888889,0.191666666666666,
0.194444444444444,0.197222222222222,0.2,0.202777777777778,0.205555555555555,
0.208333333333333,0.211111111111111,0.213888888888889,0.216666666666666,
0.219444444444444,0.222222222222222,0.225,0.227777777777777,0.230555555555555,
0.233333333333333,0.236111111111111,0.238888888888889,0.241666666666666,
0.244444444444444,0.247222222222222,0.25,0.252777777777777,0.255555555555555,
0.258333333333333,0.261111111111111,0.263888888888888,0.266666666666666,
0.269444444444444,0.272222222222222,0.275,0.277777777777777,0.280555555555555,
0.283333333333333,0.286111111111111,0.288888888888888,0.291666666666666,
0.294444444444444,0.297222222222222,0.299999999999999,0.302777777777777,
0.305555555555555,0.308333333333333,0.311111111111111,0.313888888888888,
0.316666666666666,0.319444444444444,0.322222222222222,0.324999999999999,
0.327777777777777,0.330555555555555,0.333333333333333,0.33611111111111,
0.338888888888888,0.341666666666666,0.344444444444444,0.347222222222221,
0.349999999999999,0.352777777777777,0.355555555555555,0.358333333333333,
0.36111111111111,0.363888888888888,0.366666666666666,0.369444444444444,
0.372222222222221,0.374999999999999,0.377777777777777,0.380555555555555,
0.383333333333332,0.38611111111111,0.388888888888888,0.391666666666666,
0.394444444444444,0.397222222222221,0.399999999999999,0.402777777777777,
0.405555555555555,0.408333333333332,0.41111111111111,0.413888888888888,
0.416666666666666,0.419444444444443,0.422222222222221,0.424999999999999,
0.427777777777777,0.430555555555555,0.433333333333332,0.43611111111111,
0.438888888888888,0.441666666666666,0.444444444444443,0.447222222222221,
0.449999999999999,0.452777777777777,0.455555555555554,0.458333333333332,
0.46111111111111,0.463888888888888,0.466666666666666,0.469444444444443,
0.472222222222221,0.474999999999999,0.477777777777777,0.480555555555554,
0.483333333333332,0.48611111111111,0.488888888888888,0.491666666666665,
0.494444444444443,0.497222222222221,0.499999999999999,0.502777777777777,
0.505555555555554,0.508333333333332,0.51111111111111,0.513888888888888,
0.516666666666665,0.519444444444443,0.522222222222221,0.524999999999999,
0.527777777777776,0.530555555555554,0.533333333333332,0.53611111111111,
0.538888888888888,0.541666666666665,0.544444444444443,0.547222222222221,
0.549999999999999,0.552777777777776,0.555555555555554,0.558333333333332,
0.56111111111111,0.563888888888887,0.566666666666665,0.569444444444443,
0.572222222222221,0.574999999999999,0.577777777777776,0.580555555555554,
0.583333333333332,0.58611111111111,0.588888888888887,0.591666666666665,
0.594444444444443,0.597222222222221,0.599999999999998,0.602777777777776,
0.605555555555554,0.608333333333332,0.611111111111109,0.613888888888887,
0.616666666666665,0.619444444444443,0.622222222222221,0.624999999999998,
0.627777777777776,0.630555555555554,0.633333333333332,0.636111111111109,
0.638888888888887,0.641666666666665,0.644444444444443,0.64722222222222,
0.649999999999998,0.652777777777776,0.655555555555554,0.658333333333332,
0.661111111111109,0.663888888888887,0.666666666666665,0.669444444444443,
0.67222222222222,0.674999999999998,0.677777777777776,0.680555555555554,
0.683333333333331,0.686111111111109,0.688888888888887,0.691666666666665,
0.694444444444443,0.69722222222222,0.699999999999998,0.702777777777776,
0.705555555555554,0.708333333333331,0.711111111111109,0.713888888888887,
0.716666666666665,0.719444444444442,0.72222222222222,0.724999999999998,
0.727777777777776,0.730555555555554,0.733333333333331,0.736111111111109,
0.738888888888887,0.741666666666665,0.744444444444442,0.74722222222222,
0.749999999999998,0.752777777777776,0.755555555555553,0.758333333333331,
0.761111111111109,0.763888888888887,0.766666666666664,0.769444444444442,
0.77222222222222,0.774999999999998,0.777777777777776,0.780555555555553,
0.783333333333331,0.786111111111109,0.788888888888887,0.791666666666664,
0.794444444444442,0.79722222222222,0.799999999999998,0.802777777777775,
0.805555555555553,0.808333333333331,0.811111111111109,0.813888888888887,
0.816666666666664,0.819444444444442,0.82222222222222,0.824999999999998,
0.827777777777775,0.830555555555553,0.833333333333331,0.836111111111109,
0.838888888888886,0.841666666666664,0.844444444444442,0.84722222222222,
0.849999999999998,0.852777777777775,0.855555555555553,0.858333333333331,
0.861111111111109,0.863888888888886,0.866666666666664,0.869444444444442,
0.87222222222222,0.874999999999997,0.877777777777775,0.880555555555553,
0.883333333333331,0.886111111111109,0.888888888888886,0.891666666666664,
0.894444444444442,0.89722222222222,0.899999999999997,0.902777777777775,
0.905555555555553,0.908333333333331,0.911111111111108,0.913888888888886,
0.916666666666664,0.919444444444442,0.92222222222222,0.924999999999997,
0.927777777777775,0.930555555555553,0.933333333333331,0.936111111111108,
0.938888888888886,0.941666666666664,0.944444444444442,0.947222222222219,
0.949999999999997,0.952777777777775,0.955555555555553,0.95833333333333,
0.961111111111108,0.963888888888886,0.966666666666664,0.969444444444442,
0.972222222222219,0.974999999999997,0.977777777777775,0.980555555555553,
0.98333333333333,0.986111111111108,0.988888888888886,0.991666666666664,
0.994444444444441,0.997222222222219,1.),(0.,0.15),.UNSPECIFIED.)
GEOMETRIC_REPRESENTATION_ITEM()
RATIONAL_B_SPLINE_SURFACE(((1.,1.),(1.,1.),(1.,1.),(1.,1.),(1.,1.),(1.,
1.),(1.,1.),(1.,1.),(1.,1.),(1.,1.),(1.,1.),(1.,1.),(1.,1.),(1.,1.),(1.,
1.),(1.,1.),(1.,1.),(1.,1.),(1.,1.),(1.,1.),(1.,1.),(1.,1.),(1.,1.),(1.,
1.),(1.,1.),(1.,1.),(1.,1.),(1.,1.),(1.,1.),(1.,1.),(1.,1.),(1.,1.),(1.,
1.),(1.,1.),(1.,1.),(1.,1.),(1.,1.),(1.,1.),(1.,1.),(1.,1.),(1.,1.),(1.,
1.),(1.,1.),(1.,1.),(1.,1.),(1.,1.),(1.,1.),(1.,1.),(1.,1.),(1.,1.),(1.,
1.),(1.,1.),(1.,1.),(1.,1.),(1.,1.),(1.,1.),(1.,1.),(1.,1.),(1.,1.),(1.,
1.),(1.,1.),(1.,1.),(1.,1.),(1.,1.),(1.,1.),(1.,1.),(1.,1.),(1.,1.),(1.,
1.),(1.,1.),(1.,1.),(1.,1.),(1.,1.),(1.,1.),(1.,1.),(1.,1.),(1.,1.),(1.,
1.),(1.,1.),(1.,1.),(1.,1.),(1.,1.),(1.,1.),(1.,1.),(1.,1.),(1.,1.),(1.,
1.),(1.,1.),(1.,1.),(1.,1.),(1.,1.),(1.,1.),(1.,1.),(1.,1.),(1.,1.),(1.,
1.),(1.,1.),(1.,1.),(1.,1.),(1.,1.),(1.,1.),(1.,1.),(1.,1.),(1.,1.),(1.,
1.),(1.,1.),(1.,1.),(1.,1.),(1.,1.),(1.,1.),(1.,1.),(1.,1.),(1.,1.),(1.,
1.),(1.,1.),(1.,1.),(1.,1.),(1.,1.),(1.,1.),(1.,1.),(1.,1.),(1.,1.),(1.,
1.),(1.,1.),(1.,1.),(1.,1.),(1.,1.),(1.,1.),(1.,1.),(1.,1.),(1.,1.),(1.,
1.),(1.,1.),(1.,1.),(1.,1.),(1.,1.),(1.,1.),(1.,1.),(1.,1.),(1.,1.),(1.,
1.),(1.,1.),(1.,1.),(1.,1.),(1.,1.),(1.,1.),(1.,1.),(1.,1.),(1.,1.),(1.,
1.),(1.,1.),(1.,1.),(1.,1.),(1.,1.),(1.,1.),(1.,1.),(1.,1.),(1.,1.),(1.,
1.),(1.,1.),(1.,1.),(1.,1.),(1.,1.),(1.,1.),(1.,1.),(1.,1.),(1.,1.),(1.,
1.),(1.,1.),(1.,1.),(1.,1.),(1.,1.),(1.,1.),(1.,1.),(1.,1.),(1.,1.),(1.,
1.),(1.,1.),(1.,1.),(1.,1.),(1.,1.),(1.,1.),(1.,1.),(1.,1.),(1.,1.),(1.,
1.),(1.,1.),(1.,1.),(1.,1.),(1.,1.),(1.,1.),(1.,1.),(1.,1.),(1.,1.),(1.,
1.),(1.,1.),(1.,1.),(1.,1.),(1.,1.),(1.,1.),(1.,1.),(1.,1.),(1.,1.),(1.,
1.),(1.,1.),(1.,1.),(1.,1.),(1.,1.),(1.,1.),(1.,1.),(1.,1.),(1.,1.),(1.,
1.),(1.,1.),(1.,1.),(1.,1.),(1.,1.),(1.,1.),(1.,1.),(1.,1.),(1.,1.),(1.,
1.),(1.,1.),(1.,1.),(1.,1.),(1.,1.),(1.,1.),(1.,1.),(1.,1.),(1.,1.),(1.,
1.),(1.,1.),(1.,1.),(1.,1.),(1.,1.),(1.,1.),(1.,1.),(1.,1.),(1.,1.),(1.,
1.),(1.,1.),(1.,1.),(1.,1.),(1.,1.),(1.,1.),(1.,1.),(1.,1.),(1.,1.),(1.,
1.),(1.,1.),(1.,1.),(1.,1.),(1.,1.),(1.,1.),(1.,1.),(1.,1.),(1.,1.),(1.,
1.),(1.,1.),(1.,1.),(1.,1.),(1.,1.),(1.,1.),(1.,1.),(1.,1.),(1.,1.),(1.,
1.),(1.,1.),(1.,1.),(1.,1.),(1.,1.),(1.,1.),(1.,1.),(1.,1.),(1.,1.),(1.,
1.),(1.,1.),(1.,1.),(1.,1.),(1.,1.),(1.,1.),(1.,1.),(1.,1.),(1.,1.),(1.,
1.),(1.,1.),(1.,1.),(1.,1.),(1.,1.),(1.,1.),(1.,1.),(1.,1.),(1.,1.),(1.,
1.),(1.,1.),(1.,1.),(1.,1.),(1.,1.),(1.,1.),(1.,1.),(1.,1.),(1.,1.),(1.,
1.),(1.,1.),(1.,1.),(1.,1.),(1.,1.),(1.,1.),(1.,1.),(1.,1.),(1.,1.),(1.,
1.),(1.,1.),(1.,1.),(1.,1.),(1.,1.),(1.,1.),(1.,1.),(1.,1.),(1.,1.),(1.,
1.),(1.,1.),(1.,1.),(1.,1.),(1.,1.),(1.,1.),(1.,1.),(1.,1.),(1.,1.),(1.,
1.),(1.,1.),(1.,1.),(1.,1.),(1.,1.),(1.,1.),(1.,1.),(1.,1.),(1.,1.),(1.,
1.),(1.,1.),(1.,1.),(1.,1.),(1.,1.),(1.,1.),(1.,1.),(1.,1.),(1.,1.),(1.,
1.),(1.,1.),(1.,1.),(1.,1.),(1.,1.),(1.,1.),(1.,1.),(1.,1.),(1.,1.),(1.,
1.),(1.,1.),(1.,1.),(1.,1.),(1.,1.),(1.,1.),(1.,1.),(1.,1.),(1.,1.)))
REPRESENTATION_ITEM('')
SURFACE()
);
#1082=(
BOUNDED_SURFACE()
B_SPLINE_SURFACE(5,2,((#47066,#47067,#47068,#47069,#47070,#47071,#47072,
#47073,#47074),(#47075,#47076,#47077,#47078,#47079,#47080,#47081,#47082,
#47083),(#47084,#47085,#47086,#47087,#47088,#47089,#47090,#47091,#47092),
(#47093,#47094,#47095,#47096,#47097,#47098,#47099,#47100,#47101),(#47102,
#47103,#47104,#47105,#47106,#47107,#47108,#47109,#47110),(#47111,#47112,
#47113,#47114,#47115,#47116,#47117,#47118,#47119),(#47120,#47121,#47122,
#47123,#47124,#47125,#47126,#47127,#47128),(#47129,#47130,#47131,#47132,
#47133,#47134,#47135,#47136,#47137),(#47138,#47139,#47140,#47141,#47142,
#47143,#47144,#47145,#47146),(#47147,#47148,#47149,#47150,#47151,#47152,
#47153,#47154,#47155),(#47156,#47157,#47158,#47159,#47160,#47161,#47162,
#47163,#47164),(#47165,#47166,#47167,#47168,#47169,#47170,#47171,#47172,
#47173),(#47174,#47175,#47176,#47177,#47178,#47179,#47180,#47181,#47182),
(#47183,#47184,#47185,#47186,#47187,#47188,#47189,#47190,#47191),(#47192,
#47193,#47194,#47195,#47196,#47197,#47198,#47199,#47200),(#47201,#47202,
#47203,#47204,#47205,#47206,#47207,#47208,#47209),(#47210,#47211,#47212,
#47213,#47214,#47215,#47216,#47217,#47218),(#47219,#47220,#47221,#47222,
#47223,#47224,#47225,#47226,#47227),(#47228,#47229,#47230,#47231,#47232,
#47233,#47234,#47235,#47236),(#47237,#47238,#47239,#47240,#47241,#47242,
#47243,#47244,#47245),(#47246,#47247,#47248,#47249,#47250,#47251,#47252,
#47253,#47254),(#47255,#47256,#47257,#47258,#47259,#47260,#47261,#47262,
#47263),(#47264,#47265,#47266,#47267,#47268,#47269,#47270,#47271,#47272),
(#47273,#47274,#47275,#47276,#47277,#47278,#47279,#47280,#47281),(#47282,
#47283,#47284,#47285,#47286,#47287,#47288,#47289,#47290),(#47291,#47292,
#47293,#47294,#47295,#47296,#47297,#47298,#47299),(#47300,#47301,#47302,
#47303,#47304,#47305,#47306,#47307,#47308),(#47309,#47310,#47311,#47312,
#47313,#47314,#47315,#47316,#47317),(#47318,#47319,#47320,#47321,#47322,
#47323,#47324,#47325,#47326),(#47327,#47328,#47329,#47330,#47331,#47332,
#47333,#47334,#47335)),.UNSPECIFIED.,.F.,.T.,.F.)
B_SPLINE_SURFACE_WITH_KNOTS((6,1,1,1,1,1,1,1,1,1,1,1,1,1,1,1,1,1,1,1,1,
1,1,1,1,6),(3,2,2,2,3),(-1.,-0.96,-0.92,-0.88,-0.84,-0.8,-0.76,-0.72,-0.68,
-0.64,-0.6,-0.56,-0.52,-0.48,-0.44,-0.4,-0.36,-0.32,-0.28,-0.24,-0.2,-0.16,
-0.12,-0.08,-0.04,0.),(0.,1.5707963267949,3.14159265358979,4.71238898038469,
6.28318530717959),.UNSPECIFIED.)
GEOMETRIC_REPRESENTATION_ITEM()
RATIONAL_B_SPLINE_SURFACE(((1.,0.707106781186548,1.,0.707106781186548,1.,
0.707106781186548,1.,0.707106781186548,1.),(1.,0.707106781186548,1.,0.707106781186548,
1.,0.707106781186548,1.,0.707106781186548,1.),(1.,0.707106781186548,1.,
0.707106781186548,1.,0.707106781186548,1.,0.707106781186548,1.),(1.,0.707106781186548,
1.,0.707106781186548,1.,0.707106781186548,1.,0.707106781186548,1.),(1.,
0.707106781186548,1.,0.707106781186548,1.,0.707106781186548,1.,0.707106781186548,
1.),(1.,0.707106781186548,1.,0.707106781186548,1.,0.707106781186548,1.,
0.707106781186548,1.),(1.,0.707106781186548,1.,0.707106781186548,1.,0.707106781186548,
1.,0.707106781186548,1.),(1.,0.707106781186548,1.,0.707106781186548,1.,
0.707106781186548,1.,0.707106781186548,1.),(1.,0.707106781186548,1.,0.707106781186548,
1.,0.707106781186548,1.,0.707106781186548,1.),(1.,0.707106781186548,1.,
0.707106781186548,1.,0.707106781186548,1.,0.707106781186548,1.),(1.,0.707106781186548,
1.,0.707106781186548,1.,0.707106781186548,1.,0.707106781186548,1.),(1.,
0.707106781186548,1.,0.707106781186548,1.,0.707106781186548,1.,0.707106781186548,
1.),(1.,0.707106781186548,1.,0.707106781186548,1.,0.707106781186548,1.,
0.707106781186548,1.),(1.,0.707106781186548,1.,0.707106781186548,1.,0.707106781186548,
1.,0.707106781186548,1.),(1.,0.707106781186548,1.,0.707106781186548,1.,
0.707106781186548,1.,0.707106781186548,1.),(1.,0.707106781186548,1.,0.707106781186548,
1.,0.707106781186548,1.,0.707106781186548,1.),(1.,0.707106781186548,1.,
0.707106781186548,1.,0.707106781186548,1.,0.707106781186548,1.),(1.,0.707106781186548,
1.,0.707106781186548,1.,0.707106781186548,1.,0.707106781186548,1.),(1.,
0.707106781186548,1.,0.707106781186548,1.,0.707106781186548,1.,0.707106781186548,
1.),(1.,0.707106781186548,1.,0.707106781186548,1.,0.707106781186548,1.,
0.707106781186548,1.),(1.,0.707106781186548,1.,0.707106781186548,1.,0.707106781186548,
1.,0.707106781186548,1.),(1.,0.707106781186548,1.,0.707106781186548,1.,
0.707106781186548,1.,0.707106781186548,1.),(1.,0.707106781186548,1.,0.707106781186548,
1.,0.707106781186548,1.,0.707106781186548,1.),(1.,0.707106781186548,1.,
0.707106781186548,1.,0.707106781186548,1.,0.707106781186548,1.),(1.,0.707106781186548,
1.,0.707106781186548,1.,0.707106781186548,1.,0.707106781186548,1.),(1.,
0.707106781186548,1.,0.707106781186548,1.,0.707106781186548,1.,0.707106781186548,
1.),(1.,0.707106781186548,1.,0.707106781186548,1.,0.707106781186548,1.,
0.707106781186548,1.),(1.,0.707106781186548,1.,0.707106781186548,1.,0.707106781186548,
1.,0.707106781186548,1.),(1.,0.707106781186548,1.,0.707106781186548,1.,
0.707106781186548,1.,0.707106781186548,1.),(1.,0.707106781186548,1.,0.707106781186548,
1.,0.707106781186548,1.,0.707106781186548,1.)))
REPRESENTATION_ITEM('')
SURFACE()
);
#1083=(
BOUNDED_SURFACE()
B_SPLINE_SURFACE(5,2,((#48257,#48258,#48259,#48260,#48261,#48262,#48263,
#48264,#48265),(#48266,#48267,#48268,#48269,#48270,#48271,#48272,#48273,
#48274),(#48275,#48276,#48277,#48278,#48279,#48280,#48281,#48282,#48283),
(#48284,#48285,#48286,#48287,#48288,#48289,#48290,#48291,#48292),(#48293,
#48294,#48295,#48296,#48297,#48298,#48299,#48300,#48301),(#48302,#48303,
#48304,#48305,#48306,#48307,#48308,#48309,#48310),(#48311,#48312,#48313,
#48314,#48315,#48316,#48317,#48318,#48319),(#48320,#48321,#48322,#48323,
#48324,#48325,#48326,#48327,#48328),(#48329,#48330,#48331,#48332,#48333,
#48334,#48335,#48336,#48337),(#48338,#48339,#48340,#48341,#48342,#48343,
#48344,#48345,#48346),(#48347,#48348,#48349,#48350,#48351,#48352,#48353,
#48354,#48355),(#48356,#48357,#48358,#48359,#48360,#48361,#48362,#48363,
#48364),(#48365,#48366,#48367,#48368,#48369,#48370,#48371,#48372,#48373),
(#48374,#48375,#48376,#48377,#48378,#48379,#48380,#48381,#48382),(#48383,
#48384,#48385,#48386,#48387,#48388,#48389,#48390,#48391)),.UNSPECIFIED.,
 .F.,.T.,.F.)
B_SPLINE_SURFACE_WITH_KNOTS((6,1,1,1,1,1,1,1,1,1,6),(3,2,2,2,3),(-1.,-0.9,
-0.8,-0.7,-0.6,-0.5,-0.4,-0.3,-0.2,-0.1,0.),(0.,1.5707963267949,3.14159265358979,
4.71238898038469,6.28318530717959),.UNSPECIFIED.)
GEOMETRIC_REPRESENTATION_ITEM()
RATIONAL_B_SPLINE_SURFACE(((1.,0.707106781186548,1.,0.707106781186548,1.,
0.707106781186548,1.,0.707106781186548,1.),(1.,0.707106781186548,1.,0.707106781186548,
1.,0.707106781186548,1.,0.707106781186548,1.),(1.,0.707106781186548,1.,
0.707106781186548,1.,0.707106781186548,1.,0.707106781186548,1.),(1.,0.707106781186548,
1.,0.707106781186548,1.,0.707106781186548,1.,0.707106781186548,1.),(1.,
0.707106781186548,1.,0.707106781186548,1.,0.707106781186548,1.,0.707106781186548,
1.),(1.,0.707106781186548,1.,0.707106781186548,1.,0.707106781186548,1.,
0.707106781186548,1.),(1.,0.707106781186548,1.,0.707106781186548,1.,0.707106781186548,
1.,0.707106781186548,1.),(1.,0.707106781186548,1.,0.707106781186548,1.,
0.707106781186548,1.,0.707106781186548,1.),(1.,0.707106781186548,1.,0.707106781186548,
1.,0.707106781186548,1.,0.707106781186548,1.),(1.,0.707106781186548,1.,
0.707106781186548,1.,0.707106781186548,1.,0.707106781186548,1.),(1.,0.707106781186548,
1.,0.707106781186548,1.,0.707106781186548,1.,0.707106781186548,1.),(1.,
0.707106781186548,1.,0.707106781186548,1.,0.707106781186548,1.,0.707106781186548,
1.),(1.,0.707106781186548,1.,0.707106781186548,1.,0.707106781186548,1.,
0.707106781186548,1.),(1.,0.707106781186548,1.,0.707106781186548,1.,0.707106781186548,
1.,0.707106781186548,1.),(1.,0.707106781186548,1.,0.707106781186548,1.,
0.707106781186548,1.,0.707106781186548,1.)))
REPRESENTATION_ITEM('')
SURFACE()
);
#1084=(
BOUNDED_SURFACE()
B_SPLINE_SURFACE(5,2,((#48727,#48728,#48729,#48730,#48731,#48732,#48733,
#48734,#48735),(#48736,#48737,#48738,#48739,#48740,#48741,#48742,#48743,
#48744),(#48745,#48746,#48747,#48748,#48749,#48750,#48751,#48752,#48753),
(#48754,#48755,#48756,#48757,#48758,#48759,#48760,#48761,#48762),(#48763,
#48764,#48765,#48766,#48767,#48768,#48769,#48770,#48771),(#48772,#48773,
#48774,#48775,#48776,#48777,#48778,#48779,#48780),(#48781,#48782,#48783,
#48784,#48785,#48786,#48787,#48788,#48789),(#48790,#48791,#48792,#48793,
#48794,#48795,#48796,#48797,#48798),(#48799,#48800,#48801,#48802,#48803,
#48804,#48805,#48806,#48807),(#48808,#48809,#48810,#48811,#48812,#48813,
#48814,#48815,#48816),(#48817,#48818,#48819,#48820,#48821,#48822,#48823,
#48824,#48825),(#48826,#48827,#48828,#48829,#48830,#48831,#48832,#48833,
#48834),(#48835,#48836,#48837,#48838,#48839,#48840,#48841,#48842,#48843),
(#48844,#48845,#48846,#48847,#48848,#48849,#48850,#48851,#48852),(#48853,
#48854,#48855,#48856,#48857,#48858,#48859,#48860,#48861)),.UNSPECIFIED.,
 .F.,.T.,.F.)
B_SPLINE_SURFACE_WITH_KNOTS((6,1,1,1,1,1,1,1,1,1,6),(3,2,2,2,3),(-1.,-0.9,
-0.8,-0.7,-0.6,-0.5,-0.4,-0.3,-0.2,-0.1,0.),(0.,1.5707963267949,3.14159265358979,
4.71238898038469,6.28318530717959),.UNSPECIFIED.)
GEOMETRIC_REPRESENTATION_ITEM()
RATIONAL_B_SPLINE_SURFACE(((1.,0.707106781186548,1.,0.707106781186548,1.,
0.707106781186548,1.,0.707106781186548,1.),(1.,0.707106781186548,1.,0.707106781186548,
1.,0.707106781186548,1.,0.707106781186548,1.),(1.,0.707106781186548,1.,
0.707106781186548,1.,0.707106781186548,1.,0.707106781186548,1.),(1.,0.707106781186548,
1.,0.707106781186548,1.,0.707106781186548,1.,0.707106781186548,1.),(1.,
0.707106781186548,1.,0.707106781186548,1.,0.707106781186548,1.,0.707106781186548,
1.),(1.,0.707106781186548,1.,0.707106781186548,1.,0.707106781186548,1.,
0.707106781186548,1.),(1.,0.707106781186548,1.,0.707106781186548,1.,0.707106781186548,
1.,0.707106781186548,1.),(1.,0.707106781186548,1.,0.707106781186548,1.,
0.707106781186548,1.,0.707106781186548,1.),(1.,0.707106781186548,1.,0.707106781186548,
1.,0.707106781186548,1.,0.707106781186548,1.),(1.,0.707106781186548,1.,
0.707106781186548,1.,0.707106781186548,1.,0.707106781186548,1.),(1.,0.707106781186548,
1.,0.707106781186548,1.,0.707106781186548,1.,0.707106781186548,1.),(1.,
0.707106781186548,1.,0.707106781186548,1.,0.707106781186548,1.,0.707106781186548,
1.),(1.,0.707106781186548,1.,0.707106781186548,1.,0.707106781186548,1.,
0.707106781186548,1.),(1.,0.707106781186548,1.,0.707106781186548,1.,0.707106781186548,
1.,0.707106781186548,1.),(1.,0.707106781186548,1.,0.707106781186548,1.,
0.707106781186548,1.,0.707106781186548,1.)))
REPRESENTATION_ITEM('')
SURFACE()
);
#1085=(
BOUNDED_SURFACE()
B_SPLINE_SURFACE(5,2,((#49197,#49198,#49199,#49200,#49201,#49202,#49203,
#49204,#49205),(#49206,#49207,#49208,#49209,#49210,#49211,#49212,#49213,
#49214),(#49215,#49216,#49217,#49218,#49219,#49220,#49221,#49222,#49223),
(#49224,#49225,#49226,#49227,#49228,#49229,#49230,#49231,#49232),(#49233,
#49234,#49235,#49236,#49237,#49238,#49239,#49240,#49241),(#49242,#49243,
#49244,#49245,#49246,#49247,#49248,#49249,#49250),(#49251,#49252,#49253,
#49254,#49255,#49256,#49257,#49258,#49259),(#49260,#49261,#49262,#49263,
#49264,#49265,#49266,#49267,#49268),(#49269,#49270,#49271,#49272,#49273,
#49274,#49275,#49276,#49277),(#49278,#49279,#49280,#49281,#49282,#49283,
#49284,#49285,#49286),(#49287,#49288,#49289,#49290,#49291,#49292,#49293,
#49294,#49295),(#49296,#49297,#49298,#49299,#49300,#49301,#49302,#49303,
#49304),(#49305,#49306,#49307,#49308,#49309,#49310,#49311,#49312,#49313),
(#49314,#49315,#49316,#49317,#49318,#49319,#49320,#49321,#49322),(#49323,
#49324,#49325,#49326,#49327,#49328,#49329,#49330,#49331)),.UNSPECIFIED.,
 .F.,.T.,.F.)
B_SPLINE_SURFACE_WITH_KNOTS((6,1,1,1,1,1,1,1,1,1,6),(3,2,2,2,3),(-1.,-0.9,
-0.8,-0.7,-0.6,-0.5,-0.4,-0.3,-0.2,-0.1,0.),(0.,1.5707963267949,3.14159265358979,
4.71238898038469,6.28318530717959),.UNSPECIFIED.)
GEOMETRIC_REPRESENTATION_ITEM()
RATIONAL_B_SPLINE_SURFACE(((1.,0.707106781186548,1.,0.707106781186548,1.,
0.707106781186548,1.,0.707106781186548,1.),(1.,0.707106781186548,1.,0.707106781186548,
1.,0.707106781186548,1.,0.707106781186548,1.),(1.,0.707106781186548,1.,
0.707106781186548,1.,0.707106781186548,1.,0.707106781186548,1.),(1.,0.707106781186548,
1.,0.707106781186548,1.,0.707106781186548,1.,0.707106781186548,1.),(1.,
0.707106781186548,1.,0.707106781186548,1.,0.707106781186548,1.,0.707106781186548,
1.),(1.,0.707106781186548,1.,0.707106781186548,1.,0.707106781186548,1.,
0.707106781186548,1.),(1.,0.707106781186548,1.,0.707106781186548,1.,0.707106781186548,
1.,0.707106781186548,1.),(1.,0.707106781186548,1.,0.707106781186548,1.,
0.707106781186548,1.,0.707106781186548,1.),(1.,0.707106781186548,1.,0.707106781186548,
1.,0.707106781186548,1.,0.707106781186548,1.),(1.,0.707106781186548,1.,
0.707106781186548,1.,0.707106781186548,1.,0.707106781186548,1.),(1.,0.707106781186548,
1.,0.707106781186548,1.,0.707106781186548,1.,0.707106781186548,1.),(1.,
0.707106781186548,1.,0.707106781186548,1.,0.707106781186548,1.,0.707106781186548,
1.),(1.,0.707106781186548,1.,0.707106781186548,1.,0.707106781186548,1.,
0.707106781186548,1.),(1.,0.707106781186548,1.,0.707106781186548,1.,0.707106781186548,
1.,0.707106781186548,1.),(1.,0.707106781186548,1.,0.707106781186548,1.,
0.707106781186548,1.,0.707106781186548,1.)))
REPRESENTATION_ITEM('')
SURFACE()
);
#1086=(
BOUNDED_SURFACE()
B_SPLINE_SURFACE(5,2,((#49669,#49670,#49671,#49672,#49673,#49674,#49675,
#49676,#49677),(#49678,#49679,#49680,#49681,#49682,#49683,#49684,#49685,
#49686),(#49687,#49688,#49689,#49690,#49691,#49692,#49693,#49694,#49695),
(#49696,#49697,#49698,#49699,#49700,#49701,#49702,#49703,#49704),(#49705,
#49706,#49707,#49708,#49709,#49710,#49711,#49712,#49713),(#49714,#49715,
#49716,#49717,#49718,#49719,#49720,#49721,#49722),(#49723,#49724,#49725,
#49726,#49727,#49728,#49729,#49730,#49731),(#49732,#49733,#49734,#49735,
#49736,#49737,#49738,#49739,#49740),(#49741,#49742,#49743,#49744,#49745,
#49746,#49747,#49748,#49749),(#49750,#49751,#49752,#49753,#49754,#49755,
#49756,#49757,#49758),(#49759,#49760,#49761,#49762,#49763,#49764,#49765,
#49766,#49767),(#49768,#49769,#49770,#49771,#49772,#49773,#49774,#49775,
#49776),(#49777,#49778,#49779,#49780,#49781,#49782,#49783,#49784,#49785),
(#49786,#49787,#49788,#49789,#49790,#49791,#49792,#49793,#49794),(#49795,
#49796,#49797,#49798,#49799,#49800,#49801,#49802,#49803)),.UNSPECIFIED.,
 .F.,.T.,.F.)
B_SPLINE_SURFACE_WITH_KNOTS((6,1,1,1,1,1,1,1,1,1,6),(3,2,2,2,3),(-1.,-0.9,
-0.8,-0.7,-0.6,-0.5,-0.4,-0.3,-0.2,-0.1,0.),(0.,1.5707963267949,3.14159265358979,
4.71238898038469,6.28318530717959),.UNSPECIFIED.)
GEOMETRIC_REPRESENTATION_ITEM()
RATIONAL_B_SPLINE_SURFACE(((1.,0.707106781186548,1.,0.707106781186548,1.,
0.707106781186548,1.,0.707106781186548,1.),(1.,0.707106781186548,1.,0.707106781186548,
1.,0.707106781186548,1.,0.707106781186548,1.),(1.,0.707106781186548,1.,
0.707106781186548,1.,0.707106781186548,1.,0.707106781186548,1.),(1.,0.707106781186548,
1.,0.707106781186548,1.,0.707106781186548,1.,0.707106781186548,1.),(1.,
0.707106781186548,1.,0.707106781186548,1.,0.707106781186548,1.,0.707106781186548,
1.),(1.,0.707106781186548,1.,0.707106781186548,1.,0.707106781186548,1.,
0.707106781186548,1.),(1.,0.707106781186548,1.,0.707106781186548,1.,0.707106781186548,
1.,0.707106781186548,1.),(1.,0.707106781186548,1.,0.707106781186548,1.,
0.707106781186548,1.,0.707106781186548,1.),(1.,0.707106781186548,1.,0.707106781186548,
1.,0.707106781186548,1.,0.707106781186548,1.),(1.,0.707106781186548,1.,
0.707106781186548,1.,0.707106781186548,1.,0.707106781186548,1.),(1.,0.707106781186548,
1.,0.707106781186548,1.,0.707106781186548,1.,0.707106781186548,1.),(1.,
0.707106781186548,1.,0.707106781186548,1.,0.707106781186548,1.,0.707106781186548,
1.),(1.,0.707106781186548,1.,0.707106781186548,1.,0.707106781186548,1.,
0.707106781186548,1.),(1.,0.707106781186548,1.,0.707106781186548,1.,0.707106781186548,
1.,0.707106781186548,1.),(1.,0.707106781186548,1.,0.707106781186548,1.,
0.707106781186548,1.,0.707106781186548,1.)))
REPRESENTATION_ITEM('')
SURFACE()
);
#1087=(
BOUNDED_SURFACE()
B_SPLINE_SURFACE(5,2,((#50141,#50142,#50143,#50144,#50145,#50146,#50147,
#50148,#50149),(#50150,#50151,#50152,#50153,#50154,#50155,#50156,#50157,
#50158),(#50159,#50160,#50161,#50162,#50163,#50164,#50165,#50166,#50167),
(#50168,#50169,#50170,#50171,#50172,#50173,#50174,#50175,#50176),(#50177,
#50178,#50179,#50180,#50181,#50182,#50183,#50184,#50185),(#50186,#50187,
#50188,#50189,#50190,#50191,#50192,#50193,#50194),(#50195,#50196,#50197,
#50198,#50199,#50200,#50201,#50202,#50203),(#50204,#50205,#50206,#50207,
#50208,#50209,#50210,#50211,#50212),(#50213,#50214,#50215,#50216,#50217,
#50218,#50219,#50220,#50221),(#50222,#50223,#50224,#50225,#50226,#50227,
#50228,#50229,#50230),(#50231,#50232,#50233,#50234,#50235,#50236,#50237,
#50238,#50239),(#50240,#50241,#50242,#50243,#50244,#50245,#50246,#50247,
#50248),(#50249,#50250,#50251,#50252,#50253,#50254,#50255,#50256,#50257),
(#50258,#50259,#50260,#50261,#50262,#50263,#50264,#50265,#50266),(#50267,
#50268,#50269,#50270,#50271,#50272,#50273,#50274,#50275)),.UNSPECIFIED.,
 .F.,.T.,.F.)
B_SPLINE_SURFACE_WITH_KNOTS((6,1,1,1,1,1,1,1,1,1,6),(3,2,2,2,3),(-1.,-0.9,
-0.8,-0.7,-0.6,-0.5,-0.4,-0.3,-0.2,-0.1,0.),(0.,1.5707963267949,3.14159265358979,
4.71238898038469,6.28318530717959),.UNSPECIFIED.)
GEOMETRIC_REPRESENTATION_ITEM()
RATIONAL_B_SPLINE_SURFACE(((1.,0.707106781186548,1.,0.707106781186548,1.,
0.707106781186548,1.,0.707106781186548,1.),(1.,0.707106781186548,1.,0.707106781186548,
1.,0.707106781186548,1.,0.707106781186548,1.),(1.,0.707106781186548,1.,
0.707106781186548,1.,0.707106781186548,1.,0.707106781186548,1.),(1.,0.707106781186548,
1.,0.707106781186548,1.,0.707106781186548,1.,0.707106781186548,1.),(1.,
0.707106781186548,1.,0.707106781186548,1.,0.707106781186548,1.,0.707106781186548,
1.),(1.,0.707106781186548,1.,0.707106781186548,1.,0.707106781186548,1.,
0.707106781186548,1.),(1.,0.707106781186548,1.,0.707106781186548,1.,0.707106781186548,
1.,0.707106781186548,1.),(1.,0.707106781186548,1.,0.707106781186548,1.,
0.707106781186548,1.,0.707106781186548,1.),(1.,0.707106781186548,1.,0.707106781186548,
1.,0.707106781186548,1.,0.707106781186548,1.),(1.,0.707106781186548,1.,
0.707106781186548,1.,0.707106781186548,1.,0.707106781186548,1.),(1.,0.707106781186548,
1.,0.707106781186548,1.,0.707106781186548,1.,0.707106781186548,1.),(1.,
0.707106781186548,1.,0.707106781186548,1.,0.707106781186548,1.,0.707106781186548,
1.),(1.,0.707106781186548,1.,0.707106781186548,1.,0.707106781186548,1.,
0.707106781186548,1.),(1.,0.707106781186548,1.,0.707106781186548,1.,0.707106781186548,
1.,0.707106781186548,1.),(1.,0.707106781186548,1.,0.707106781186548,1.,
0.707106781186548,1.,0.707106781186548,1.)))
REPRESENTATION_ITEM('')
SURFACE()
);
#1088=(
BOUNDED_SURFACE()
B_SPLINE_SURFACE(5,2,((#50611,#50612,#50613,#50614,#50615,#50616,#50617,
#50618,#50619),(#50620,#50621,#50622,#50623,#50624,#50625,#50626,#50627,
#50628),(#50629,#50630,#50631,#50632,#50633,#50634,#50635,#50636,#50637),
(#50638,#50639,#50640,#50641,#50642,#50643,#50644,#50645,#50646),(#50647,
#50648,#50649,#50650,#50651,#50652,#50653,#50654,#50655),(#50656,#50657,
#50658,#50659,#50660,#50661,#50662,#50663,#50664),(#50665,#50666,#50667,
#50668,#50669,#50670,#50671,#50672,#50673),(#50674,#50675,#50676,#50677,
#50678,#50679,#50680,#50681,#50682),(#50683,#50684,#50685,#50686,#50687,
#50688,#50689,#50690,#50691),(#50692,#50693,#50694,#50695,#50696,#50697,
#50698,#50699,#50700),(#50701,#50702,#50703,#50704,#50705,#50706,#50707,
#50708,#50709),(#50710,#50711,#50712,#50713,#50714,#50715,#50716,#50717,
#50718),(#50719,#50720,#50721,#50722,#50723,#50724,#50725,#50726,#50727),
(#50728,#50729,#50730,#50731,#50732,#50733,#50734,#50735,#50736),(#50737,
#50738,#50739,#50740,#50741,#50742,#50743,#50744,#50745)),.UNSPECIFIED.,
 .F.,.T.,.F.)
B_SPLINE_SURFACE_WITH_KNOTS((6,1,1,1,1,1,1,1,1,1,6),(3,2,2,2,3),(-1.,-0.9,
-0.8,-0.7,-0.6,-0.5,-0.4,-0.3,-0.2,-0.1,0.),(0.,1.5707963267949,3.14159265358979,
4.71238898038469,6.28318530717959),.UNSPECIFIED.)
GEOMETRIC_REPRESENTATION_ITEM()
RATIONAL_B_SPLINE_SURFACE(((1.,0.707106781186548,1.,0.707106781186548,1.,
0.707106781186548,1.,0.707106781186548,1.),(1.,0.707106781186548,1.,0.707106781186548,
1.,0.707106781186548,1.,0.707106781186548,1.),(1.,0.707106781186548,1.,
0.707106781186548,1.,0.707106781186548,1.,0.707106781186548,1.),(1.,0.707106781186548,
1.,0.707106781186548,1.,0.707106781186548,1.,0.707106781186548,1.),(1.,
0.707106781186548,1.,0.707106781186548,1.,0.707106781186548,1.,0.707106781186548,
1.),(1.,0.707106781186548,1.,0.707106781186548,1.,0.707106781186548,1.,
0.707106781186548,1.),(1.,0.707106781186548,1.,0.707106781186548,1.,0.707106781186548,
1.,0.707106781186548,1.),(1.,0.707106781186548,1.,0.707106781186548,1.,
0.707106781186548,1.,0.707106781186548,1.),(1.,0.707106781186548,1.,0.707106781186548,
1.,0.707106781186548,1.,0.707106781186548,1.),(1.,0.707106781186548,1.,
0.707106781186548,1.,0.707106781186548,1.,0.707106781186548,1.),(1.,0.707106781186548,
1.,0.707106781186548,1.,0.707106781186548,1.,0.707106781186548,1.),(1.,
0.707106781186548,1.,0.707106781186548,1.,0.707106781186548,1.,0.707106781186548,
1.),(1.,0.707106781186548,1.,0.707106781186548,1.,0.707106781186548,1.,
0.707106781186548,1.),(1.,0.707106781186548,1.,0.707106781186548,1.,0.707106781186548,
1.,0.707106781186548,1.),(1.,0.707106781186548,1.,0.707106781186548,1.,
0.707106781186548,1.,0.707106781186548,1.)))
REPRESENTATION_ITEM('')
SURFACE()
);
#1089=(
BOUNDED_SURFACE()
B_SPLINE_SURFACE(5,2,((#51046,#51047,#51048,#51049,#51050,#51051,#51052,
#51053,#51054),(#51055,#51056,#51057,#51058,#51059,#51060,#51061,#51062,
#51063),(#51064,#51065,#51066,#51067,#51068,#51069,#51070,#51071,#51072),
(#51073,#51074,#51075,#51076,#51077,#51078,#51079,#51080,#51081),(#51082,
#51083,#51084,#51085,#51086,#51087,#51088,#51089,#51090),(#51091,#51092,
#51093,#51094,#51095,#51096,#51097,#51098,#51099),(#51100,#51101,#51102,
#51103,#51104,#51105,#51106,#51107,#51108),(#51109,#51110,#51111,#51112,
#51113,#51114,#51115,#51116,#51117),(#51118,#51119,#51120,#51121,#51122,
#51123,#51124,#51125,#51126),(#51127,#51128,#51129,#51130,#51131,#51132,
#51133,#51134,#51135),(#51136,#51137,#51138,#51139,#51140,#51141,#51142,
#51143,#51144),(#51145,#51146,#51147,#51148,#51149,#51150,#51151,#51152,
#51153),(#51154,#51155,#51156,#51157,#51158,#51159,#51160,#51161,#51162),
(#51163,#51164,#51165,#51166,#51167,#51168,#51169,#51170,#51171),(#51172,
#51173,#51174,#51175,#51176,#51177,#51178,#51179,#51180)),.UNSPECIFIED.,
 .F.,.T.,.F.)
B_SPLINE_SURFACE_WITH_KNOTS((6,1,1,1,1,1,1,1,1,1,6),(3,2,2,2,3),(-1.,-0.9,
-0.8,-0.7,-0.6,-0.5,-0.4,-0.3,-0.2,-0.1,0.),(0.,1.5707963267949,3.14159265358979,
4.71238898038469,6.28318530717959),.UNSPECIFIED.)
GEOMETRIC_REPRESENTATION_ITEM()
RATIONAL_B_SPLINE_SURFACE(((1.,0.707106781186548,1.,0.707106781186548,1.,
0.707106781186548,1.,0.707106781186548,1.),(1.,0.707106781186548,1.,0.707106781186548,
1.,0.707106781186548,1.,0.707106781186548,1.),(1.,0.707106781186548,1.,
0.707106781186548,1.,0.707106781186548,1.,0.707106781186548,1.),(1.,0.707106781186548,
1.,0.707106781186548,1.,0.707106781186548,1.,0.707106781186548,1.),(1.,
0.707106781186548,1.,0.707106781186548,1.,0.707106781186548,1.,0.707106781186548,
1.),(1.,0.707106781186548,1.,0.707106781186548,1.,0.707106781186548,1.,
0.707106781186548,1.),(1.,0.707106781186548,1.,0.707106781186548,1.,0.707106781186548,
1.,0.707106781186548,1.),(1.,0.707106781186548,1.,0.707106781186548,1.,
0.707106781186548,1.,0.707106781186548,1.),(1.,0.707106781186548,1.,0.707106781186548,
1.,0.707106781186548,1.,0.707106781186548,1.),(1.,0.707106781186548,1.,
0.707106781186548,1.,0.707106781186548,1.,0.707106781186548,1.),(1.,0.707106781186548,
1.,0.707106781186548,1.,0.707106781186548,1.,0.707106781186548,1.),(1.,
0.707106781186548,1.,0.707106781186548,1.,0.707106781186548,1.,0.707106781186548,
1.),(1.,0.707106781186548,1.,0.707106781186548,1.,0.707106781186548,1.,
0.707106781186548,1.),(1.,0.707106781186548,1.,0.707106781186548,1.,0.707106781186548,
1.,0.707106781186548,1.),(1.,0.707106781186548,1.,0.707106781186548,1.,
0.707106781186548,1.,0.707106781186548,1.)))
REPRESENTATION_ITEM('')
SURFACE()
);
#1090=(
BOUNDED_SURFACE()
B_SPLINE_SURFACE(5,2,((#51574,#51575,#51576,#51577,#51578,#51579,#51580,
#51581,#51582,#51583,#51584),(#51585,#51586,#51587,#51588,#51589,#51590,
#51591,#51592,#51593,#51594,#51595),(#51596,#51597,#51598,#51599,#51600,
#51601,#51602,#51603,#51604,#51605,#51606),(#51607,#51608,#51609,#51610,
#51611,#51612,#51613,#51614,#51615,#51616,#51617),(#51618,#51619,#51620,
#51621,#51622,#51623,#51624,#51625,#51626,#51627,#51628),(#51629,#51630,
#51631,#51632,#51633,#51634,#51635,#51636,#51637,#51638,#51639),(#51640,
#51641,#51642,#51643,#51644,#51645,#51646,#51647,#51648,#51649,#51650),
(#51651,#51652,#51653,#51654,#51655,#51656,#51657,#51658,#51659,#51660,
#51661),(#51662,#51663,#51664,#51665,#51666,#51667,#51668,#51669,#51670,
#51671,#51672),(#51673,#51674,#51675,#51676,#51677,#51678,#51679,#51680,
#51681,#51682,#51683),(#51684,#51685,#51686,#51687,#51688,#51689,#51690,
#51691,#51692,#51693,#51694),(#51695,#51696,#51697,#51698,#51699,#51700,
#51701,#51702,#51703,#51704,#51705),(#51706,#51707,#51708,#51709,#51710,
#51711,#51712,#51713,#51714,#51715,#51716),(#51717,#51718,#51719,#51720,
#51721,#51722,#51723,#51724,#51725,#51726,#51727),(#51728,#51729,#51730,
#51731,#51732,#51733,#51734,#51735,#51736,#51737,#51738),(#51739,#51740,
#51741,#51742,#51743,#51744,#51745,#51746,#51747,#51748,#51749),(#51750,
#51751,#51752,#51753,#51754,#51755,#51756,#51757,#51758,#51759,#51760),
(#51761,#51762,#51763,#51764,#51765,#51766,#51767,#51768,#51769,#51770,
#51771),(#51772,#51773,#51774,#51775,#51776,#51777,#51778,#51779,#51780,
#51781,#51782),(#51783,#51784,#51785,#51786,#51787,#51788,#51789,#51790,
#51791,#51792,#51793),(#51794,#51795,#51796,#51797,#51798,#51799,#51800,
#51801,#51802,#51803,#51804),(#51805,#51806,#51807,#51808,#51809,#51810,
#51811,#51812,#51813,#51814,#51815),(#51816,#51817,#51818,#51819,#51820,
#51821,#51822,#51823,#51824,#51825,#51826),(#51827,#51828,#51829,#51830,
#51831,#51832,#51833,#51834,#51835,#51836,#51837),(#51838,#51839,#51840,
#51841,#51842,#51843,#51844,#51845,#51846,#51847,#51848)),.UNSPECIFIED.,
 .F.,.T.,.F.)
B_SPLINE_SURFACE_WITH_KNOTS((6,1,1,1,1,1,1,1,1,1,1,1,1,1,1,1,1,1,1,1,6),
(3,2,2,2,2,3),(-1.,-0.95,-0.9,-0.85,-0.8,-0.75,-0.7,-0.65,-0.6,-0.55,-0.5,
-0.45,-0.4,-0.35,-0.3,-0.25,-0.2,-0.15,-0.1,-0.05,0.),(-0.960413254722853,
0.,1.5707963267949,3.14159265358979,4.71238898038469,5.32277205245673),
 .UNSPECIFIED.)
GEOMETRIC_REPRESENTATION_ITEM()
RATIONAL_B_SPLINE_SURFACE(((0.860825335104674,0.820919794139797,1.,0.707106781186548,
1.,0.707106781186548,1.,0.707106781186548,1.,0.88618698704675,0.860825335104674),
(0.860825335104674,0.820919794139797,1.,0.707106781186548,1.,0.707106781186548,
1.,0.707106781186548,1.,0.88618698704675,0.860825335104674),(0.860825335104674,
0.820919794139797,1.,0.707106781186548,1.,0.707106781186548,1.,0.707106781186548,
1.,0.88618698704675,0.860825335104674),(0.860825335104674,0.820919794139797,
1.,0.707106781186548,1.,0.707106781186548,1.,0.707106781186548,1.,0.88618698704675,
0.860825335104674),(0.860825335104674,0.820919794139797,1.,0.707106781186548,
1.,0.707106781186548,1.,0.707106781186548,1.,0.88618698704675,0.860825335104674),
(0.860825335104674,0.820919794139797,1.,0.707106781186548,1.,0.707106781186548,
1.,0.707106781186548,1.,0.88618698704675,0.860825335104674),(0.860825335104674,
0.820919794139797,1.,0.707106781186548,1.,0.707106781186548,1.,0.707106781186548,
1.,0.88618698704675,0.860825335104674),(0.860825335104674,0.820919794139797,
1.,0.707106781186548,1.,0.707106781186548,1.,0.707106781186548,1.,0.88618698704675,
0.860825335104674),(0.860825335104674,0.820919794139797,1.,0.707106781186548,
1.,0.707106781186548,1.,0.707106781186548,1.,0.88618698704675,0.860825335104674),
(0.860825335104674,0.820919794139797,1.,0.707106781186548,1.,0.707106781186548,
1.,0.707106781186548,1.,0.88618698704675,0.860825335104674),(0.860825335104674,
0.820919794139797,1.,0.707106781186548,1.,0.707106781186548,1.,0.707106781186548,
1.,0.88618698704675,0.860825335104674),(0.860825335104674,0.820919794139797,
1.,0.707106781186548,1.,0.707106781186548,1.,0.707106781186548,1.,0.88618698704675,
0.860825335104674),(0.860825335104674,0.820919794139797,1.,0.707106781186548,
1.,0.707106781186548,1.,0.707106781186548,1.,0.88618698704675,0.860825335104674),
(0.860825335104674,0.820919794139797,1.,0.707106781186548,1.,0.707106781186548,
1.,0.707106781186548,1.,0.88618698704675,0.860825335104674),(0.860825335104674,
0.820919794139797,1.,0.707106781186548,1.,0.707106781186548,1.,0.707106781186548,
1.,0.88618698704675,0.860825335104674),(0.860825335104674,0.820919794139797,
1.,0.707106781186548,1.,0.707106781186548,1.,0.707106781186548,1.,0.88618698704675,
0.860825335104674),(0.860825335104674,0.820919794139797,1.,0.707106781186548,
1.,0.707106781186548,1.,0.707106781186548,1.,0.88618698704675,0.860825335104674),
(0.860825335104674,0.820919794139797,1.,0.707106781186548,1.,0.707106781186548,
1.,0.707106781186548,1.,0.88618698704675,0.860825335104674),(0.860825335104674,
0.820919794139797,1.,0.707106781186548,1.,0.707106781186548,1.,0.707106781186548,
1.,0.88618698704675,0.860825335104674),(0.860825335104674,0.820919794139797,
1.,0.707106781186548,1.,0.707106781186548,1.,0.707106781186548,1.,0.88618698704675,
0.860825335104674),(0.860825335104674,0.820919794139797,1.,0.707106781186548,
1.,0.707106781186548,1.,0.707106781186548,1.,0.88618698704675,0.860825335104674),
(0.860825335104674,0.820919794139797,1.,0.707106781186548,1.,0.707106781186548,
1.,0.707106781186548,1.,0.88618698704675,0.860825335104674),(0.860825335104674,
0.820919794139797,1.,0.707106781186548,1.,0.707106781186548,1.,0.707106781186548,
1.,0.88618698704675,0.860825335104674),(0.860825335104674,0.820919794139797,
1.,0.707106781186548,1.,0.707106781186548,1.,0.707106781186548,1.,0.88618698704675,
0.860825335104674),(0.860825335104674,0.820919794139797,1.,0.707106781186548,
1.,0.707106781186548,1.,0.707106781186548,1.,0.88618698704675,0.860825335104674)))
REPRESENTATION_ITEM('')
SURFACE()
);
#1091=(
BOUNDED_SURFACE()
B_SPLINE_SURFACE(5,2,((#52396,#52397,#52398,#52399,#52400,#52401,#52402,
#52403,#52404,#52405,#52406),(#52407,#52408,#52409,#52410,#52411,#52412,
#52413,#52414,#52415,#52416,#52417),(#52418,#52419,#52420,#52421,#52422,
#52423,#52424,#52425,#52426,#52427,#52428),(#52429,#52430,#52431,#52432,
#52433,#52434,#52435,#52436,#52437,#52438,#52439),(#52440,#52441,#52442,
#52443,#52444,#52445,#52446,#52447,#52448,#52449,#52450),(#52451,#52452,
#52453,#52454,#52455,#52456,#52457,#52458,#52459,#52460,#52461),(#52462,
#52463,#52464,#52465,#52466,#52467,#52468,#52469,#52470,#52471,#52472),
(#52473,#52474,#52475,#52476,#52477,#52478,#52479,#52480,#52481,#52482,
#52483),(#52484,#52485,#52486,#52487,#52488,#52489,#52490,#52491,#52492,
#52493,#52494),(#52495,#52496,#52497,#52498,#52499,#52500,#52501,#52502,
#52503,#52504,#52505),(#52506,#52507,#52508,#52509,#52510,#52511,#52512,
#52513,#52514,#52515,#52516),(#52517,#52518,#52519,#52520,#52521,#52522,
#52523,#52524,#52525,#52526,#52527),(#52528,#52529,#52530,#52531,#52532,
#52533,#52534,#52535,#52536,#52537,#52538),(#52539,#52540,#52541,#52542,
#52543,#52544,#52545,#52546,#52547,#52548,#52549),(#52550,#52551,#52552,
#52553,#52554,#52555,#52556,#52557,#52558,#52559,#52560),(#52561,#52562,
#52563,#52564,#52565,#52566,#52567,#52568,#52569,#52570,#52571),(#52572,
#52573,#52574,#52575,#52576,#52577,#52578,#52579,#52580,#52581,#52582),
(#52583,#52584,#52585,#52586,#52587,#52588,#52589,#52590,#52591,#52592,
#52593),(#52594,#52595,#52596,#52597,#52598,#52599,#52600,#52601,#52602,
#52603,#52604),(#52605,#52606,#52607,#52608,#52609,#52610,#52611,#52612,
#52613,#52614,#52615),(#52616,#52617,#52618,#52619,#52620,#52621,#52622,
#52623,#52624,#52625,#52626),(#52627,#52628,#52629,#52630,#52631,#52632,
#52633,#52634,#52635,#52636,#52637),(#52638,#52639,#52640,#52641,#52642,
#52643,#52644,#52645,#52646,#52647,#52648),(#52649,#52650,#52651,#52652,
#52653,#52654,#52655,#52656,#52657,#52658,#52659),(#52660,#52661,#52662,
#52663,#52664,#52665,#52666,#52667,#52668,#52669,#52670)),.UNSPECIFIED.,
 .F.,.T.,.F.)
B_SPLINE_SURFACE_WITH_KNOTS((6,1,1,1,1,1,1,1,1,1,1,1,1,1,1,1,1,1,1,1,6),
(3,2,2,2,2,3),(-1.,-0.95,-0.9,-0.85,-0.8,-0.75,-0.7,-0.65,-0.6,-0.55,-0.5,
-0.45,-0.4,-0.35,-0.3,-0.25,-0.2,-0.15,-0.1,-0.05,0.),(-0.960413254722853,
0.,1.5707963267949,3.14159265358979,4.71238898038469,5.32277205245673),
 .UNSPECIFIED.)
GEOMETRIC_REPRESENTATION_ITEM()
RATIONAL_B_SPLINE_SURFACE(((0.860825335104674,0.820919794139797,1.,0.707106781186548,
1.,0.707106781186548,1.,0.707106781186548,1.,0.88618698704675,0.860825335104674),
(0.860825335104674,0.820919794139797,1.,0.707106781186548,1.,0.707106781186548,
1.,0.707106781186548,1.,0.88618698704675,0.860825335104674),(0.860825335104674,
0.820919794139797,1.,0.707106781186548,1.,0.707106781186548,1.,0.707106781186548,
1.,0.88618698704675,0.860825335104674),(0.860825335104674,0.820919794139797,
1.,0.707106781186548,1.,0.707106781186548,1.,0.707106781186548,1.,0.88618698704675,
0.860825335104674),(0.860825335104674,0.820919794139797,1.,0.707106781186548,
1.,0.707106781186548,1.,0.707106781186548,1.,0.88618698704675,0.860825335104674),
(0.860825335104674,0.820919794139797,1.,0.707106781186548,1.,0.707106781186548,
1.,0.707106781186548,1.,0.88618698704675,0.860825335104674),(0.860825335104674,
0.820919794139797,1.,0.707106781186548,1.,0.707106781186548,1.,0.707106781186548,
1.,0.88618698704675,0.860825335104674),(0.860825335104674,0.820919794139797,
1.,0.707106781186548,1.,0.707106781186548,1.,0.707106781186548,1.,0.88618698704675,
0.860825335104674),(0.860825335104674,0.820919794139797,1.,0.707106781186548,
1.,0.707106781186548,1.,0.707106781186548,1.,0.88618698704675,0.860825335104674),
(0.860825335104674,0.820919794139797,1.,0.707106781186548,1.,0.707106781186548,
1.,0.707106781186548,1.,0.88618698704675,0.860825335104674),(0.860825335104674,
0.820919794139797,1.,0.707106781186548,1.,0.707106781186548,1.,0.707106781186548,
1.,0.88618698704675,0.860825335104674),(0.860825335104674,0.820919794139797,
1.,0.707106781186548,1.,0.707106781186548,1.,0.707106781186548,1.,0.88618698704675,
0.860825335104674),(0.860825335104674,0.820919794139797,1.,0.707106781186548,
1.,0.707106781186548,1.,0.707106781186548,1.,0.88618698704675,0.860825335104674),
(0.860825335104674,0.820919794139797,1.,0.707106781186548,1.,0.707106781186548,
1.,0.707106781186548,1.,0.88618698704675,0.860825335104674),(0.860825335104674,
0.820919794139797,1.,0.707106781186548,1.,0.707106781186548,1.,0.707106781186548,
1.,0.88618698704675,0.860825335104674),(0.860825335104674,0.820919794139797,
1.,0.707106781186548,1.,0.707106781186548,1.,0.707106781186548,1.,0.88618698704675,
0.860825335104674),(0.860825335104674,0.820919794139797,1.,0.707106781186548,
1.,0.707106781186548,1.,0.707106781186548,1.,0.88618698704675,0.860825335104674),
(0.860825335104674,0.820919794139797,1.,0.707106781186548,1.,0.707106781186548,
1.,0.707106781186548,1.,0.88618698704675,0.860825335104674),(0.860825335104674,
0.820919794139797,1.,0.707106781186548,1.,0.707106781186548,1.,0.707106781186548,
1.,0.88618698704675,0.860825335104674),(0.860825335104674,0.820919794139797,
1.,0.707106781186548,1.,0.707106781186548,1.,0.707106781186548,1.,0.88618698704675,
0.860825335104674),(0.860825335104674,0.820919794139797,1.,0.707106781186548,
1.,0.707106781186548,1.,0.707106781186548,1.,0.88618698704675,0.860825335104674),
(0.860825335104674,0.820919794139797,1.,0.707106781186548,1.,0.707106781186548,
1.,0.707106781186548,1.,0.88618698704675,0.860825335104674),(0.860825335104674,
0.820919794139797,1.,0.707106781186548,1.,0.707106781186548,1.,0.707106781186548,
1.,0.88618698704675,0.860825335104674),(0.860825335104674,0.820919794139797,
1.,0.707106781186548,1.,0.707106781186548,1.,0.707106781186548,1.,0.88618698704675,
0.860825335104674),(0.860825335104674,0.820919794139797,1.,0.707106781186548,
1.,0.707106781186548,1.,0.707106781186548,1.,0.88618698704675,0.860825335104674)))
REPRESENTATION_ITEM('')
SURFACE()
);
#1092=(
BOUNDED_SURFACE()
B_SPLINE_SURFACE(5,2,((#53253,#53254,#53255,#53256,#53257,#53258,#53259,
#53260,#53261,#53262,#53263),(#53264,#53265,#53266,#53267,#53268,#53269,
#53270,#53271,#53272,#53273,#53274),(#53275,#53276,#53277,#53278,#53279,
#53280,#53281,#53282,#53283,#53284,#53285),(#53286,#53287,#53288,#53289,
#53290,#53291,#53292,#53293,#53294,#53295,#53296),(#53297,#53298,#53299,
#53300,#53301,#53302,#53303,#53304,#53305,#53306,#53307),(#53308,#53309,
#53310,#53311,#53312,#53313,#53314,#53315,#53316,#53317,#53318),(#53319,
#53320,#53321,#53322,#53323,#53324,#53325,#53326,#53327,#53328,#53329),
(#53330,#53331,#53332,#53333,#53334,#53335,#53336,#53337,#53338,#53339,
#53340),(#53341,#53342,#53343,#53344,#53345,#53346,#53347,#53348,#53349,
#53350,#53351),(#53352,#53353,#53354,#53355,#53356,#53357,#53358,#53359,
#53360,#53361,#53362),(#53363,#53364,#53365,#53366,#53367,#53368,#53369,
#53370,#53371,#53372,#53373),(#53374,#53375,#53376,#53377,#53378,#53379,
#53380,#53381,#53382,#53383,#53384),(#53385,#53386,#53387,#53388,#53389,
#53390,#53391,#53392,#53393,#53394,#53395),(#53396,#53397,#53398,#53399,
#53400,#53401,#53402,#53403,#53404,#53405,#53406),(#53407,#53408,#53409,
#53410,#53411,#53412,#53413,#53414,#53415,#53416,#53417),(#53418,#53419,
#53420,#53421,#53422,#53423,#53424,#53425,#53426,#53427,#53428),(#53429,
#53430,#53431,#53432,#53433,#53434,#53435,#53436,#53437,#53438,#53439),
(#53440,#53441,#53442,#53443,#53444,#53445,#53446,#53447,#53448,#53449,
#53450),(#53451,#53452,#53453,#53454,#53455,#53456,#53457,#53458,#53459,
#53460,#53461),(#53462,#53463,#53464,#53465,#53466,#53467,#53468,#53469,
#53470,#53471,#53472),(#53473,#53474,#53475,#53476,#53477,#53478,#53479,
#53480,#53481,#53482,#53483),(#53484,#53485,#53486,#53487,#53488,#53489,
#53490,#53491,#53492,#53493,#53494),(#53495,#53496,#53497,#53498,#53499,
#53500,#53501,#53502,#53503,#53504,#53505),(#53506,#53507,#53508,#53509,
#53510,#53511,#53512,#53513,#53514,#53515,#53516),(#53517,#53518,#53519,
#53520,#53521,#53522,#53523,#53524,#53525,#53526,#53527)),.UNSPECIFIED.,
 .F.,.T.,.F.)
B_SPLINE_SURFACE_WITH_KNOTS((6,1,1,1,1,1,1,1,1,1,1,1,1,1,1,1,1,1,1,1,6),
(3,2,2,2,2,3),(-1.,-0.95,-0.9,-0.85,-0.8,-0.75,-0.7,-0.65,-0.6,-0.55,-0.5,
-0.45,-0.4,-0.35,-0.3,-0.25,-0.2,-0.15,-0.1,-0.05,0.),(-0.960413254722853,
0.,1.5707963267949,3.14159265358979,4.71238898038469,5.32277205245673),
 .UNSPECIFIED.)
GEOMETRIC_REPRESENTATION_ITEM()
RATIONAL_B_SPLINE_SURFACE(((0.860825335104674,0.820919794139797,1.,0.707106781186548,
1.,0.707106781186548,1.,0.707106781186548,1.,0.88618698704675,0.860825335104674),
(0.860825335104674,0.820919794139797,1.,0.707106781186548,1.,0.707106781186548,
1.,0.707106781186548,1.,0.88618698704675,0.860825335104674),(0.860825335104674,
0.820919794139797,1.,0.707106781186548,1.,0.707106781186548,1.,0.707106781186548,
1.,0.88618698704675,0.860825335104674),(0.860825335104674,0.820919794139797,
1.,0.707106781186548,1.,0.707106781186548,1.,0.707106781186548,1.,0.88618698704675,
0.860825335104674),(0.860825335104674,0.820919794139797,1.,0.707106781186548,
1.,0.707106781186548,1.,0.707106781186548,1.,0.88618698704675,0.860825335104674),
(0.860825335104674,0.820919794139797,1.,0.707106781186548,1.,0.707106781186548,
1.,0.707106781186548,1.,0.88618698704675,0.860825335104674),(0.860825335104674,
0.820919794139797,1.,0.707106781186548,1.,0.707106781186548,1.,0.707106781186548,
1.,0.88618698704675,0.860825335104674),(0.860825335104674,0.820919794139797,
1.,0.707106781186548,1.,0.707106781186548,1.,0.707106781186548,1.,0.88618698704675,
0.860825335104674),(0.860825335104674,0.820919794139797,1.,0.707106781186548,
1.,0.707106781186548,1.,0.707106781186548,1.,0.88618698704675,0.860825335104674),
(0.860825335104674,0.820919794139797,1.,0.707106781186548,1.,0.707106781186548,
1.,0.707106781186548,1.,0.88618698704675,0.860825335104674),(0.860825335104674,
0.820919794139797,1.,0.707106781186548,1.,0.707106781186548,1.,0.707106781186548,
1.,0.88618698704675,0.860825335104674),(0.860825335104674,0.820919794139797,
1.,0.707106781186548,1.,0.707106781186548,1.,0.707106781186548,1.,0.88618698704675,
0.860825335104674),(0.860825335104674,0.820919794139797,1.,0.707106781186548,
1.,0.707106781186548,1.,0.707106781186548,1.,0.88618698704675,0.860825335104674),
(0.860825335104674,0.820919794139797,1.,0.707106781186548,1.,0.707106781186548,
1.,0.707106781186548,1.,0.88618698704675,0.860825335104674),(0.860825335104674,
0.820919794139797,1.,0.707106781186548,1.,0.707106781186548,1.,0.707106781186548,
1.,0.88618698704675,0.860825335104674),(0.860825335104674,0.820919794139797,
1.,0.707106781186548,1.,0.707106781186548,1.,0.707106781186548,1.,0.88618698704675,
0.860825335104674),(0.860825335104674,0.820919794139797,1.,0.707106781186548,
1.,0.707106781186548,1.,0.707106781186548,1.,0.88618698704675,0.860825335104674),
(0.860825335104674,0.820919794139797,1.,0.707106781186548,1.,0.707106781186548,
1.,0.707106781186548,1.,0.88618698704675,0.860825335104674),(0.860825335104674,
0.820919794139797,1.,0.707106781186548,1.,0.707106781186548,1.,0.707106781186548,
1.,0.88618698704675,0.860825335104674),(0.860825335104674,0.820919794139797,
1.,0.707106781186548,1.,0.707106781186548,1.,0.707106781186548,1.,0.88618698704675,
0.860825335104674),(0.860825335104674,0.820919794139797,1.,0.707106781186548,
1.,0.707106781186548,1.,0.707106781186548,1.,0.88618698704675,0.860825335104674),
(0.860825335104674,0.820919794139797,1.,0.707106781186548,1.,0.707106781186548,
1.,0.707106781186548,1.,0.88618698704675,0.860825335104674),(0.860825335104674,
0.820919794139797,1.,0.707106781186548,1.,0.707106781186548,1.,0.707106781186548,
1.,0.88618698704675,0.860825335104674),(0.860825335104674,0.820919794139797,
1.,0.707106781186548,1.,0.707106781186548,1.,0.707106781186548,1.,0.88618698704675,
0.860825335104674),(0.860825335104674,0.820919794139797,1.,0.707106781186548,
1.,0.707106781186548,1.,0.707106781186548,1.,0.88618698704675,0.860825335104674)))
REPRESENTATION_ITEM('')
SURFACE()
);
#1093=(
BOUNDED_SURFACE()
B_SPLINE_SURFACE(5,2,((#54070,#54071,#54072,#54073,#54074,#54075,#54076,
#54077,#54078,#54079,#54080),(#54081,#54082,#54083,#54084,#54085,#54086,
#54087,#54088,#54089,#54090,#54091),(#54092,#54093,#54094,#54095,#54096,
#54097,#54098,#54099,#54100,#54101,#54102),(#54103,#54104,#54105,#54106,
#54107,#54108,#54109,#54110,#54111,#54112,#54113),(#54114,#54115,#54116,
#54117,#54118,#54119,#54120,#54121,#54122,#54123,#54124),(#54125,#54126,
#54127,#54128,#54129,#54130,#54131,#54132,#54133,#54134,#54135),(#54136,
#54137,#54138,#54139,#54140,#54141,#54142,#54143,#54144,#54145,#54146),
(#54147,#54148,#54149,#54150,#54151,#54152,#54153,#54154,#54155,#54156,
#54157),(#54158,#54159,#54160,#54161,#54162,#54163,#54164,#54165,#54166,
#54167,#54168),(#54169,#54170,#54171,#54172,#54173,#54174,#54175,#54176,
#54177,#54178,#54179),(#54180,#54181,#54182,#54183,#54184,#54185,#54186,
#54187,#54188,#54189,#54190),(#54191,#54192,#54193,#54194,#54195,#54196,
#54197,#54198,#54199,#54200,#54201),(#54202,#54203,#54204,#54205,#54206,
#54207,#54208,#54209,#54210,#54211,#54212),(#54213,#54214,#54215,#54216,
#54217,#54218,#54219,#54220,#54221,#54222,#54223),(#54224,#54225,#54226,
#54227,#54228,#54229,#54230,#54231,#54232,#54233,#54234),(#54235,#54236,
#54237,#54238,#54239,#54240,#54241,#54242,#54243,#54244,#54245),(#54246,
#54247,#54248,#54249,#54250,#54251,#54252,#54253,#54254,#54255,#54256),
(#54257,#54258,#54259,#54260,#54261,#54262,#54263,#54264,#54265,#54266,
#54267),(#54268,#54269,#54270,#54271,#54272,#54273,#54274,#54275,#54276,
#54277,#54278),(#54279,#54280,#54281,#54282,#54283,#54284,#54285,#54286,
#54287,#54288,#54289),(#54290,#54291,#54292,#54293,#54294,#54295,#54296,
#54297,#54298,#54299,#54300),(#54301,#54302,#54303,#54304,#54305,#54306,
#54307,#54308,#54309,#54310,#54311),(#54312,#54313,#54314,#54315,#54316,
#54317,#54318,#54319,#54320,#54321,#54322),(#54323,#54324,#54325,#54326,
#54327,#54328,#54329,#54330,#54331,#54332,#54333),(#54334,#54335,#54336,
#54337,#54338,#54339,#54340,#54341,#54342,#54343,#54344)),.UNSPECIFIED.,
 .F.,.T.,.F.)
B_SPLINE_SURFACE_WITH_KNOTS((6,1,1,1,1,1,1,1,1,1,1,1,1,1,1,1,1,1,1,1,6),
(3,2,2,2,2,3),(-1.,-0.95,-0.9,-0.85,-0.8,-0.75,-0.7,-0.65,-0.6,-0.55,-0.5,
-0.45,-0.4,-0.35,-0.3,-0.25,-0.2,-0.15,-0.1,-0.05,0.),(-0.960413254722853,
0.,1.5707963267949,3.14159265358979,4.71238898038469,5.32277205245673),
 .UNSPECIFIED.)
GEOMETRIC_REPRESENTATION_ITEM()
RATIONAL_B_SPLINE_SURFACE(((0.860825335104674,0.820919794139797,1.,0.707106781186548,
1.,0.707106781186548,1.,0.707106781186548,1.,0.88618698704675,0.860825335104674),
(0.860825335104674,0.820919794139797,1.,0.707106781186548,1.,0.707106781186548,
1.,0.707106781186548,1.,0.88618698704675,0.860825335104674),(0.860825335104674,
0.820919794139797,1.,0.707106781186548,1.,0.707106781186548,1.,0.707106781186548,
1.,0.88618698704675,0.860825335104674),(0.860825335104674,0.820919794139797,
1.,0.707106781186548,1.,0.707106781186548,1.,0.707106781186548,1.,0.88618698704675,
0.860825335104674),(0.860825335104674,0.820919794139797,1.,0.707106781186548,
1.,0.707106781186548,1.,0.707106781186548,1.,0.88618698704675,0.860825335104674),
(0.860825335104674,0.820919794139797,1.,0.707106781186548,1.,0.707106781186548,
1.,0.707106781186548,1.,0.88618698704675,0.860825335104674),(0.860825335104674,
0.820919794139797,1.,0.707106781186548,1.,0.707106781186548,1.,0.707106781186548,
1.,0.88618698704675,0.860825335104674),(0.860825335104674,0.820919794139797,
1.,0.707106781186548,1.,0.707106781186548,1.,0.707106781186548,1.,0.88618698704675,
0.860825335104674),(0.860825335104674,0.820919794139797,1.,0.707106781186548,
1.,0.707106781186548,1.,0.707106781186548,1.,0.88618698704675,0.860825335104674),
(0.860825335104674,0.820919794139797,1.,0.707106781186548,1.,0.707106781186548,
1.,0.707106781186548,1.,0.88618698704675,0.860825335104674),(0.860825335104674,
0.820919794139797,1.,0.707106781186548,1.,0.707106781186548,1.,0.707106781186548,
1.,0.88618698704675,0.860825335104674),(0.860825335104674,0.820919794139797,
1.,0.707106781186548,1.,0.707106781186548,1.,0.707106781186548,1.,0.88618698704675,
0.860825335104674),(0.860825335104674,0.820919794139797,1.,0.707106781186548,
1.,0.707106781186548,1.,0.707106781186548,1.,0.88618698704675,0.860825335104674),
(0.860825335104674,0.820919794139797,1.,0.707106781186548,1.,0.707106781186548,
1.,0.707106781186548,1.,0.88618698704675,0.860825335104674),(0.860825335104674,
0.820919794139797,1.,0.707106781186548,1.,0.707106781186548,1.,0.707106781186548,
1.,0.88618698704675,0.860825335104674),(0.860825335104674,0.820919794139797,
1.,0.707106781186548,1.,0.707106781186548,1.,0.707106781186548,1.,0.88618698704675,
0.860825335104674),(0.860825335104674,0.820919794139797,1.,0.707106781186548,
1.,0.707106781186548,1.,0.707106781186548,1.,0.88618698704675,0.860825335104674),
(0.860825335104674,0.820919794139797,1.,0.707106781186548,1.,0.707106781186548,
1.,0.707106781186548,1.,0.88618698704675,0.860825335104674),(0.860825335104674,
0.820919794139797,1.,0.707106781186548,1.,0.707106781186548,1.,0.707106781186548,
1.,0.88618698704675,0.860825335104674),(0.860825335104674,0.820919794139797,
1.,0.707106781186548,1.,0.707106781186548,1.,0.707106781186548,1.,0.88618698704675,
0.860825335104674),(0.860825335104674,0.820919794139797,1.,0.707106781186548,
1.,0.707106781186548,1.,0.707106781186548,1.,0.88618698704675,0.860825335104674),
(0.860825335104674,0.820919794139797,1.,0.707106781186548,1.,0.707106781186548,
1.,0.707106781186548,1.,0.88618698704675,0.860825335104674),(0.860825335104674,
0.820919794139797,1.,0.707106781186548,1.,0.707106781186548,1.,0.707106781186548,
1.,0.88618698704675,0.860825335104674),(0.860825335104674,0.820919794139797,
1.,0.707106781186548,1.,0.707106781186548,1.,0.707106781186548,1.,0.88618698704675,
0.860825335104674),(0.860825335104674,0.820919794139797,1.,0.707106781186548,
1.,0.707106781186548,1.,0.707106781186548,1.,0.88618698704675,0.860825335104674)))
REPRESENTATION_ITEM('')
SURFACE()
);
#1094=(
BOUNDED_SURFACE()
B_SPLINE_SURFACE(5,2,((#54922,#54923,#54924,#54925,#54926,#54927,#54928,
#54929,#54930,#54931,#54932),(#54933,#54934,#54935,#54936,#54937,#54938,
#54939,#54940,#54941,#54942,#54943),(#54944,#54945,#54946,#54947,#54948,
#54949,#54950,#54951,#54952,#54953,#54954),(#54955,#54956,#54957,#54958,
#54959,#54960,#54961,#54962,#54963,#54964,#54965),(#54966,#54967,#54968,
#54969,#54970,#54971,#54972,#54973,#54974,#54975,#54976),(#54977,#54978,
#54979,#54980,#54981,#54982,#54983,#54984,#54985,#54986,#54987),(#54988,
#54989,#54990,#54991,#54992,#54993,#54994,#54995,#54996,#54997,#54998),
(#54999,#55000,#55001,#55002,#55003,#55004,#55005,#55006,#55007,#55008,
#55009),(#55010,#55011,#55012,#55013,#55014,#55015,#55016,#55017,#55018,
#55019,#55020),(#55021,#55022,#55023,#55024,#55025,#55026,#55027,#55028,
#55029,#55030,#55031),(#55032,#55033,#55034,#55035,#55036,#55037,#55038,
#55039,#55040,#55041,#55042),(#55043,#55044,#55045,#55046,#55047,#55048,
#55049,#55050,#55051,#55052,#55053),(#55054,#55055,#55056,#55057,#55058,
#55059,#55060,#55061,#55062,#55063,#55064),(#55065,#55066,#55067,#55068,
#55069,#55070,#55071,#55072,#55073,#55074,#55075),(#55076,#55077,#55078,
#55079,#55080,#55081,#55082,#55083,#55084,#55085,#55086),(#55087,#55088,
#55089,#55090,#55091,#55092,#55093,#55094,#55095,#55096,#55097),(#55098,
#55099,#55100,#55101,#55102,#55103,#55104,#55105,#55106,#55107,#55108),
(#55109,#55110,#55111,#55112,#55113,#55114,#55115,#55116,#55117,#55118,
#55119),(#55120,#55121,#55122,#55123,#55124,#55125,#55126,#55127,#55128,
#55129,#55130),(#55131,#55132,#55133,#55134,#55135,#55136,#55137,#55138,
#55139,#55140,#55141),(#55142,#55143,#55144,#55145,#55146,#55147,#55148,
#55149,#55150,#55151,#55152),(#55153,#55154,#55155,#55156,#55157,#55158,
#55159,#55160,#55161,#55162,#55163),(#55164,#55165,#55166,#55167,#55168,
#55169,#55170,#55171,#55172,#55173,#55174),(#55175,#55176,#55177,#55178,
#55179,#55180,#55181,#55182,#55183,#55184,#55185),(#55186,#55187,#55188,
#55189,#55190,#55191,#55192,#55193,#55194,#55195,#55196)),.UNSPECIFIED.,
 .F.,.T.,.F.)
B_SPLINE_SURFACE_WITH_KNOTS((6,1,1,1,1,1,1,1,1,1,1,1,1,1,1,1,1,1,1,1,6),
(3,2,2,2,2,3),(-1.,-0.95,-0.9,-0.85,-0.8,-0.75,-0.7,-0.65,-0.6,-0.55,-0.5,
-0.45,-0.4,-0.35,-0.3,-0.25,-0.2,-0.15,-0.1,-0.05,0.),(-0.960413254722853,
0.,1.5707963267949,3.14159265358979,4.71238898038469,5.32277205245673),
 .UNSPECIFIED.)
GEOMETRIC_REPRESENTATION_ITEM()
RATIONAL_B_SPLINE_SURFACE(((0.860825335104674,0.820919794139797,1.,0.707106781186548,
1.,0.707106781186548,1.,0.707106781186548,1.,0.88618698704675,0.860825335104674),
(0.860825335104674,0.820919794139797,1.,0.707106781186548,1.,0.707106781186548,
1.,0.707106781186548,1.,0.88618698704675,0.860825335104674),(0.860825335104674,
0.820919794139797,1.,0.707106781186548,1.,0.707106781186548,1.,0.707106781186548,
1.,0.88618698704675,0.860825335104674),(0.860825335104674,0.820919794139797,
1.,0.707106781186548,1.,0.707106781186548,1.,0.707106781186548,1.,0.88618698704675,
0.860825335104674),(0.860825335104674,0.820919794139797,1.,0.707106781186548,
1.,0.707106781186548,1.,0.707106781186548,1.,0.88618698704675,0.860825335104674),
(0.860825335104674,0.820919794139797,1.,0.707106781186548,1.,0.707106781186548,
1.,0.707106781186548,1.,0.88618698704675,0.860825335104674),(0.860825335104674,
0.820919794139797,1.,0.707106781186548,1.,0.707106781186548,1.,0.707106781186548,
1.,0.88618698704675,0.860825335104674),(0.860825335104674,0.820919794139797,
1.,0.707106781186548,1.,0.707106781186548,1.,0.707106781186548,1.,0.88618698704675,
0.860825335104674),(0.860825335104674,0.820919794139797,1.,0.707106781186548,
1.,0.707106781186548,1.,0.707106781186548,1.,0.88618698704675,0.860825335104674),
(0.860825335104674,0.820919794139797,1.,0.707106781186548,1.,0.707106781186548,
1.,0.707106781186548,1.,0.88618698704675,0.860825335104674),(0.860825335104674,
0.820919794139797,1.,0.707106781186548,1.,0.707106781186548,1.,0.707106781186548,
1.,0.88618698704675,0.860825335104674),(0.860825335104674,0.820919794139797,
1.,0.707106781186548,1.,0.707106781186548,1.,0.707106781186548,1.,0.88618698704675,
0.860825335104674),(0.860825335104674,0.820919794139797,1.,0.707106781186548,
1.,0.707106781186548,1.,0.707106781186548,1.,0.88618698704675,0.860825335104674),
(0.860825335104674,0.820919794139797,1.,0.707106781186548,1.,0.707106781186548,
1.,0.707106781186548,1.,0.88618698704675,0.860825335104674),(0.860825335104674,
0.820919794139797,1.,0.707106781186548,1.,0.707106781186548,1.,0.707106781186548,
1.,0.88618698704675,0.860825335104674),(0.860825335104674,0.820919794139797,
1.,0.707106781186548,1.,0.707106781186548,1.,0.707106781186548,1.,0.88618698704675,
0.860825335104674),(0.860825335104674,0.820919794139797,1.,0.707106781186548,
1.,0.707106781186548,1.,0.707106781186548,1.,0.88618698704675,0.860825335104674),
(0.860825335104674,0.820919794139797,1.,0.707106781186548,1.,0.707106781186548,
1.,0.707106781186548,1.,0.88618698704675,0.860825335104674),(0.860825335104674,
0.820919794139797,1.,0.707106781186548,1.,0.707106781186548,1.,0.707106781186548,
1.,0.88618698704675,0.860825335104674),(0.860825335104674,0.820919794139797,
1.,0.707106781186548,1.,0.707106781186548,1.,0.707106781186548,1.,0.88618698704675,
0.860825335104674),(0.860825335104674,0.820919794139797,1.,0.707106781186548,
1.,0.707106781186548,1.,0.707106781186548,1.,0.88618698704675,0.860825335104674),
(0.860825335104674,0.820919794139797,1.,0.707106781186548,1.,0.707106781186548,
1.,0.707106781186548,1.,0.88618698704675,0.860825335104674),(0.860825335104674,
0.820919794139797,1.,0.707106781186548,1.,0.707106781186548,1.,0.707106781186548,
1.,0.88618698704675,0.860825335104674),(0.860825335104674,0.820919794139797,
1.,0.707106781186548,1.,0.707106781186548,1.,0.707106781186548,1.,0.88618698704675,
0.860825335104674),(0.860825335104674,0.820919794139797,1.,0.707106781186548,
1.,0.707106781186548,1.,0.707106781186548,1.,0.88618698704675,0.860825335104674)))
REPRESENTATION_ITEM('')
SURFACE()
);
#1095=(
BOUNDED_SURFACE()
B_SPLINE_SURFACE(5,2,((#55744,#55745,#55746,#55747,#55748,#55749,#55750,
#55751,#55752,#55753,#55754),(#55755,#55756,#55757,#55758,#55759,#55760,
#55761,#55762,#55763,#55764,#55765),(#55766,#55767,#55768,#55769,#55770,
#55771,#55772,#55773,#55774,#55775,#55776),(#55777,#55778,#55779,#55780,
#55781,#55782,#55783,#55784,#55785,#55786,#55787),(#55788,#55789,#55790,
#55791,#55792,#55793,#55794,#55795,#55796,#55797,#55798),(#55799,#55800,
#55801,#55802,#55803,#55804,#55805,#55806,#55807,#55808,#55809),(#55810,
#55811,#55812,#55813,#55814,#55815,#55816,#55817,#55818,#55819,#55820),
(#55821,#55822,#55823,#55824,#55825,#55826,#55827,#55828,#55829,#55830,
#55831),(#55832,#55833,#55834,#55835,#55836,#55837,#55838,#55839,#55840,
#55841,#55842),(#55843,#55844,#55845,#55846,#55847,#55848,#55849,#55850,
#55851,#55852,#55853),(#55854,#55855,#55856,#55857,#55858,#55859,#55860,
#55861,#55862,#55863,#55864),(#55865,#55866,#55867,#55868,#55869,#55870,
#55871,#55872,#55873,#55874,#55875),(#55876,#55877,#55878,#55879,#55880,
#55881,#55882,#55883,#55884,#55885,#55886),(#55887,#55888,#55889,#55890,
#55891,#55892,#55893,#55894,#55895,#55896,#55897),(#55898,#55899,#55900,
#55901,#55902,#55903,#55904,#55905,#55906,#55907,#55908),(#55909,#55910,
#55911,#55912,#55913,#55914,#55915,#55916,#55917,#55918,#55919),(#55920,
#55921,#55922,#55923,#55924,#55925,#55926,#55927,#55928,#55929,#55930),
(#55931,#55932,#55933,#55934,#55935,#55936,#55937,#55938,#55939,#55940,
#55941),(#55942,#55943,#55944,#55945,#55946,#55947,#55948,#55949,#55950,
#55951,#55952),(#55953,#55954,#55955,#55956,#55957,#55958,#55959,#55960,
#55961,#55962,#55963),(#55964,#55965,#55966,#55967,#55968,#55969,#55970,
#55971,#55972,#55973,#55974),(#55975,#55976,#55977,#55978,#55979,#55980,
#55981,#55982,#55983,#55984,#55985),(#55986,#55987,#55988,#55989,#55990,
#55991,#55992,#55993,#55994,#55995,#55996),(#55997,#55998,#55999,#56000,
#56001,#56002,#56003,#56004,#56005,#56006,#56007),(#56008,#56009,#56010,
#56011,#56012,#56013,#56014,#56015,#56016,#56017,#56018)),.UNSPECIFIED.,
 .F.,.T.,.F.)
B_SPLINE_SURFACE_WITH_KNOTS((6,1,1,1,1,1,1,1,1,1,1,1,1,1,1,1,1,1,1,1,6),
(3,2,2,2,2,3),(-1.,-0.95,-0.9,-0.85,-0.8,-0.75,-0.7,-0.65,-0.6,-0.55,-0.5,
-0.45,-0.4,-0.35,-0.3,-0.25,-0.2,-0.15,-0.1,-0.05,0.),(-0.960413254722853,
0.,1.5707963267949,3.14159265358979,4.71238898038469,5.32277205245673),
 .UNSPECIFIED.)
GEOMETRIC_REPRESENTATION_ITEM()
RATIONAL_B_SPLINE_SURFACE(((0.860825335104674,0.820919794139797,1.,0.707106781186548,
1.,0.707106781186548,1.,0.707106781186548,1.,0.88618698704675,0.860825335104674),
(0.860825335104674,0.820919794139797,1.,0.707106781186548,1.,0.707106781186548,
1.,0.707106781186548,1.,0.88618698704675,0.860825335104674),(0.860825335104674,
0.820919794139797,1.,0.707106781186548,1.,0.707106781186548,1.,0.707106781186548,
1.,0.88618698704675,0.860825335104674),(0.860825335104674,0.820919794139797,
1.,0.707106781186548,1.,0.707106781186548,1.,0.707106781186548,1.,0.88618698704675,
0.860825335104674),(0.860825335104674,0.820919794139797,1.,0.707106781186548,
1.,0.707106781186548,1.,0.707106781186548,1.,0.88618698704675,0.860825335104674),
(0.860825335104674,0.820919794139797,1.,0.707106781186548,1.,0.707106781186548,
1.,0.707106781186548,1.,0.88618698704675,0.860825335104674),(0.860825335104674,
0.820919794139797,1.,0.707106781186548,1.,0.707106781186548,1.,0.707106781186548,
1.,0.88618698704675,0.860825335104674),(0.860825335104674,0.820919794139797,
1.,0.707106781186548,1.,0.707106781186548,1.,0.707106781186548,1.,0.88618698704675,
0.860825335104674),(0.860825335104674,0.820919794139797,1.,0.707106781186548,
1.,0.707106781186548,1.,0.707106781186548,1.,0.88618698704675,0.860825335104674),
(0.860825335104674,0.820919794139797,1.,0.707106781186548,1.,0.707106781186548,
1.,0.707106781186548,1.,0.88618698704675,0.860825335104674),(0.860825335104674,
0.820919794139797,1.,0.707106781186548,1.,0.707106781186548,1.,0.707106781186548,
1.,0.88618698704675,0.860825335104674),(0.860825335104674,0.820919794139797,
1.,0.707106781186548,1.,0.707106781186548,1.,0.707106781186548,1.,0.88618698704675,
0.860825335104674),(0.860825335104674,0.820919794139797,1.,0.707106781186548,
1.,0.707106781186548,1.,0.707106781186548,1.,0.88618698704675,0.860825335104674),
(0.860825335104674,0.820919794139797,1.,0.707106781186548,1.,0.707106781186548,
1.,0.707106781186548,1.,0.88618698704675,0.860825335104674),(0.860825335104674,
0.820919794139797,1.,0.707106781186548,1.,0.707106781186548,1.,0.707106781186548,
1.,0.88618698704675,0.860825335104674),(0.860825335104674,0.820919794139797,
1.,0.707106781186548,1.,0.707106781186548,1.,0.707106781186548,1.,0.88618698704675,
0.860825335104674),(0.860825335104674,0.820919794139797,1.,0.707106781186548,
1.,0.707106781186548,1.,0.707106781186548,1.,0.88618698704675,0.860825335104674),
(0.860825335104674,0.820919794139797,1.,0.707106781186548,1.,0.707106781186548,
1.,0.707106781186548,1.,0.88618698704675,0.860825335104674),(0.860825335104674,
0.820919794139797,1.,0.707106781186548,1.,0.707106781186548,1.,0.707106781186548,
1.,0.88618698704675,0.860825335104674),(0.860825335104674,0.820919794139797,
1.,0.707106781186548,1.,0.707106781186548,1.,0.707106781186548,1.,0.88618698704675,
0.860825335104674),(0.860825335104674,0.820919794139797,1.,0.707106781186548,
1.,0.707106781186548,1.,0.707106781186548,1.,0.88618698704675,0.860825335104674),
(0.860825335104674,0.820919794139797,1.,0.707106781186548,1.,0.707106781186548,
1.,0.707106781186548,1.,0.88618698704675,0.860825335104674),(0.860825335104674,
0.820919794139797,1.,0.707106781186548,1.,0.707106781186548,1.,0.707106781186548,
1.,0.88618698704675,0.860825335104674),(0.860825335104674,0.820919794139797,
1.,0.707106781186548,1.,0.707106781186548,1.,0.707106781186548,1.,0.88618698704675,
0.860825335104674),(0.860825335104674,0.820919794139797,1.,0.707106781186548,
1.,0.707106781186548,1.,0.707106781186548,1.,0.88618698704675,0.860825335104674)))
REPRESENTATION_ITEM('')
SURFACE()
);
#1096=(
BOUNDED_SURFACE()
B_SPLINE_SURFACE(5,2,((#56254,#56255,#56256,#56257,#56258,#56259,#56260,
#56261,#56262),(#56263,#56264,#56265,#56266,#56267,#56268,#56269,#56270,
#56271),(#56272,#56273,#56274,#56275,#56276,#56277,#56278,#56279,#56280),
(#56281,#56282,#56283,#56284,#56285,#56286,#56287,#56288,#56289),(#56290,
#56291,#56292,#56293,#56294,#56295,#56296,#56297,#56298),(#56299,#56300,
#56301,#56302,#56303,#56304,#56305,#56306,#56307),(#56308,#56309,#56310,
#56311,#56312,#56313,#56314,#56315,#56316),(#56317,#56318,#56319,#56320,
#56321,#56322,#56323,#56324,#56325),(#56326,#56327,#56328,#56329,#56330,
#56331,#56332,#56333,#56334),(#56335,#56336,#56337,#56338,#56339,#56340,
#56341,#56342,#56343),(#56344,#56345,#56346,#56347,#56348,#56349,#56350,
#56351,#56352),(#56353,#56354,#56355,#56356,#56357,#56358,#56359,#56360,
#56361),(#56362,#56363,#56364,#56365,#56366,#56367,#56368,#56369,#56370),
(#56371,#56372,#56373,#56374,#56375,#56376,#56377,#56378,#56379),(#56380,
#56381,#56382,#56383,#56384,#56385,#56386,#56387,#56388),(#56389,#56390,
#56391,#56392,#56393,#56394,#56395,#56396,#56397),(#56398,#56399,#56400,
#56401,#56402,#56403,#56404,#56405,#56406),(#56407,#56408,#56409,#56410,
#56411,#56412,#56413,#56414,#56415),(#56416,#56417,#56418,#56419,#56420,
#56421,#56422,#56423,#56424),(#56425,#56426,#56427,#56428,#56429,#56430,
#56431,#56432,#56433),(#56434,#56435,#56436,#56437,#56438,#56439,#56440,
#56441,#56442),(#56443,#56444,#56445,#56446,#56447,#56448,#56449,#56450,
#56451),(#56452,#56453,#56454,#56455,#56456,#56457,#56458,#56459,#56460),
(#56461,#56462,#56463,#56464,#56465,#56466,#56467,#56468,#56469),(#56470,
#56471,#56472,#56473,#56474,#56475,#56476,#56477,#56478),(#56479,#56480,
#56481,#56482,#56483,#56484,#56485,#56486,#56487),(#56488,#56489,#56490,
#56491,#56492,#56493,#56494,#56495,#56496),(#56497,#56498,#56499,#56500,
#56501,#56502,#56503,#56504,#56505),(#56506,#56507,#56508,#56509,#56510,
#56511,#56512,#56513,#56514),(#56515,#56516,#56517,#56518,#56519,#56520,
#56521,#56522,#56523)),.UNSPECIFIED.,.F.,.T.,.F.)
B_SPLINE_SURFACE_WITH_KNOTS((6,1,1,1,1,1,1,1,1,1,1,1,1,1,1,1,1,1,1,1,1,
1,1,1,1,6),(3,2,2,2,3),(-1.,-0.96,-0.92,-0.88,-0.84,-0.8,-0.76,-0.72,-0.68,
-0.64,-0.6,-0.56,-0.52,-0.48,-0.44,-0.4,-0.36,-0.32,-0.28,-0.24,-0.2,-0.16,
-0.12,-0.08,-0.04,0.),(0.,1.5707963267949,3.14159265358979,4.71238898038469,
6.28318530717959),.UNSPECIFIED.)
GEOMETRIC_REPRESENTATION_ITEM()
RATIONAL_B_SPLINE_SURFACE(((1.,0.707106781186548,1.,0.707106781186548,1.,
0.707106781186548,1.,0.707106781186548,1.),(1.,0.707106781186548,1.,0.707106781186548,
1.,0.707106781186548,1.,0.707106781186548,1.),(1.,0.707106781186548,1.,
0.707106781186548,1.,0.707106781186548,1.,0.707106781186548,1.),(1.,0.707106781186548,
1.,0.707106781186548,1.,0.707106781186548,1.,0.707106781186548,1.),(1.,
0.707106781186548,1.,0.707106781186548,1.,0.707106781186548,1.,0.707106781186548,
1.),(1.,0.707106781186548,1.,0.707106781186548,1.,0.707106781186548,1.,
0.707106781186548,1.),(1.,0.707106781186548,1.,0.707106781186548,1.,0.707106781186548,
1.,0.707106781186548,1.),(1.,0.707106781186548,1.,0.707106781186548,1.,
0.707106781186548,1.,0.707106781186548,1.),(1.,0.707106781186548,1.,0.707106781186548,
1.,0.707106781186548,1.,0.707106781186548,1.),(1.,0.707106781186548,1.,
0.707106781186548,1.,0.707106781186548,1.,0.707106781186548,1.),(1.,0.707106781186548,
1.,0.707106781186548,1.,0.707106781186548,1.,0.707106781186548,1.),(1.,
0.707106781186548,1.,0.707106781186548,1.,0.707106781186548,1.,0.707106781186548,
1.),(1.,0.707106781186548,1.,0.707106781186548,1.,0.707106781186548,1.,
0.707106781186548,1.),(1.,0.707106781186548,1.,0.707106781186548,1.,0.707106781186548,
1.,0.707106781186548,1.),(1.,0.707106781186548,1.,0.707106781186548,1.,
0.707106781186548,1.,0.707106781186548,1.),(1.,0.707106781186548,1.,0.707106781186548,
1.,0.707106781186548,1.,0.707106781186548,1.),(1.,0.707106781186548,1.,
0.707106781186548,1.,0.707106781186548,1.,0.707106781186548,1.),(1.,0.707106781186548,
1.,0.707106781186548,1.,0.707106781186548,1.,0.707106781186548,1.),(1.,
0.707106781186548,1.,0.707106781186548,1.,0.707106781186548,1.,0.707106781186548,
1.),(1.,0.707106781186548,1.,0.707106781186548,1.,0.707106781186548,1.,
0.707106781186548,1.),(1.,0.707106781186548,1.,0.707106781186548,1.,0.707106781186548,
1.,0.707106781186548,1.),(1.,0.707106781186548,1.,0.707106781186548,1.,
0.707106781186548,1.,0.707106781186548,1.),(1.,0.707106781186548,1.,0.707106781186548,
1.,0.707106781186548,1.,0.707106781186548,1.),(1.,0.707106781186548,1.,
0.707106781186548,1.,0.707106781186548,1.,0.707106781186548,1.),(1.,0.707106781186548,
1.,0.707106781186548,1.,0.707106781186548,1.,0.707106781186548,1.),(1.,
0.707106781186548,1.,0.707106781186548,1.,0.707106781186548,1.,0.707106781186548,
1.),(1.,0.707106781186548,1.,0.707106781186548,1.,0.707106781186548,1.,
0.707106781186548,1.),(1.,0.707106781186548,1.,0.707106781186548,1.,0.707106781186548,
1.,0.707106781186548,1.),(1.,0.707106781186548,1.,0.707106781186548,1.,
0.707106781186548,1.,0.707106781186548,1.),(1.,0.707106781186548,1.,0.707106781186548,
1.,0.707106781186548,1.,0.707106781186548,1.)))
REPRESENTATION_ITEM('')
SURFACE()
);
#1097=(
BOUNDED_SURFACE()
B_SPLINE_SURFACE(5,2,((#56834,#56835,#56836,#56837,#56838,#56839,#56840,
#56841,#56842,#56843,#56844),(#56845,#56846,#56847,#56848,#56849,#56850,
#56851,#56852,#56853,#56854,#56855),(#56856,#56857,#56858,#56859,#56860,
#56861,#56862,#56863,#56864,#56865,#56866),(#56867,#56868,#56869,#56870,
#56871,#56872,#56873,#56874,#56875,#56876,#56877),(#56878,#56879,#56880,
#56881,#56882,#56883,#56884,#56885,#56886,#56887,#56888),(#56889,#56890,
#56891,#56892,#56893,#56894,#56895,#56896,#56897,#56898,#56899),(#56900,
#56901,#56902,#56903,#56904,#56905,#56906,#56907,#56908,#56909,#56910),
(#56911,#56912,#56913,#56914,#56915,#56916,#56917,#56918,#56919,#56920,
#56921),(#56922,#56923,#56924,#56925,#56926,#56927,#56928,#56929,#56930,
#56931,#56932),(#56933,#56934,#56935,#56936,#56937,#56938,#56939,#56940,
#56941,#56942,#56943),(#56944,#56945,#56946,#56947,#56948,#56949,#56950,
#56951,#56952,#56953,#56954),(#56955,#56956,#56957,#56958,#56959,#56960,
#56961,#56962,#56963,#56964,#56965),(#56966,#56967,#56968,#56969,#56970,
#56971,#56972,#56973,#56974,#56975,#56976),(#56977,#56978,#56979,#56980,
#56981,#56982,#56983,#56984,#56985,#56986,#56987),(#56988,#56989,#56990,
#56991,#56992,#56993,#56994,#56995,#56996,#56997,#56998),(#56999,#57000,
#57001,#57002,#57003,#57004,#57005,#57006,#57007,#57008,#57009),(#57010,
#57011,#57012,#57013,#57014,#57015,#57016,#57017,#57018,#57019,#57020),
(#57021,#57022,#57023,#57024,#57025,#57026,#57027,#57028,#57029,#57030,
#57031),(#57032,#57033,#57034,#57035,#57036,#57037,#57038,#57039,#57040,
#57041,#57042),(#57043,#57044,#57045,#57046,#57047,#57048,#57049,#57050,
#57051,#57052,#57053),(#57054,#57055,#57056,#57057,#57058,#57059,#57060,
#57061,#57062,#57063,#57064),(#57065,#57066,#57067,#57068,#57069,#57070,
#57071,#57072,#57073,#57074,#57075),(#57076,#57077,#57078,#57079,#57080,
#57081,#57082,#57083,#57084,#57085,#57086),(#57087,#57088,#57089,#57090,
#57091,#57092,#57093,#57094,#57095,#57096,#57097),(#57098,#57099,#57100,
#57101,#57102,#57103,#57104,#57105,#57106,#57107,#57108)),.UNSPECIFIED.,
 .F.,.T.,.F.)
B_SPLINE_SURFACE_WITH_KNOTS((6,1,1,1,1,1,1,1,1,1,1,1,1,1,1,1,1,1,1,1,6),
(3,2,2,2,2,3),(-1.,-0.95,-0.9,-0.85,-0.8,-0.75,-0.7,-0.65,-0.6,-0.55,-0.5,
-0.45,-0.4,-0.35,-0.3,-0.25,-0.2,-0.15,-0.1,-0.05,0.),(-0.960413254722853,
0.,1.5707963267949,3.14159265358979,4.71238898038469,5.32277205245673),
 .UNSPECIFIED.)
GEOMETRIC_REPRESENTATION_ITEM()
RATIONAL_B_SPLINE_SURFACE(((0.860825335104674,0.820919794139797,1.,0.707106781186548,
1.,0.707106781186548,1.,0.707106781186548,1.,0.88618698704675,0.860825335104674),
(0.860825335104674,0.820919794139797,1.,0.707106781186548,1.,0.707106781186548,
1.,0.707106781186548,1.,0.88618698704675,0.860825335104674),(0.860825335104674,
0.820919794139797,1.,0.707106781186548,1.,0.707106781186548,1.,0.707106781186548,
1.,0.88618698704675,0.860825335104674),(0.860825335104674,0.820919794139797,
1.,0.707106781186548,1.,0.707106781186548,1.,0.707106781186548,1.,0.88618698704675,
0.860825335104674),(0.860825335104674,0.820919794139797,1.,0.707106781186548,
1.,0.707106781186548,1.,0.707106781186548,1.,0.88618698704675,0.860825335104674),
(0.860825335104674,0.820919794139797,1.,0.707106781186548,1.,0.707106781186548,
1.,0.707106781186548,1.,0.88618698704675,0.860825335104674),(0.860825335104674,
0.820919794139797,1.,0.707106781186548,1.,0.707106781186548,1.,0.707106781186548,
1.,0.88618698704675,0.860825335104674),(0.860825335104674,0.820919794139797,
1.,0.707106781186548,1.,0.707106781186548,1.,0.707106781186548,1.,0.88618698704675,
0.860825335104674),(0.860825335104674,0.820919794139797,1.,0.707106781186548,
1.,0.707106781186548,1.,0.707106781186548,1.,0.88618698704675,0.860825335104674),
(0.860825335104674,0.820919794139797,1.,0.707106781186548,1.,0.707106781186548,
1.,0.707106781186548,1.,0.88618698704675,0.860825335104674),(0.860825335104674,
0.820919794139797,1.,0.707106781186548,1.,0.707106781186548,1.,0.707106781186548,
1.,0.88618698704675,0.860825335104674),(0.860825335104674,0.820919794139797,
1.,0.707106781186548,1.,0.707106781186548,1.,0.707106781186548,1.,0.88618698704675,
0.860825335104674),(0.860825335104674,0.820919794139797,1.,0.707106781186548,
1.,0.707106781186548,1.,0.707106781186548,1.,0.88618698704675,0.860825335104674),
(0.860825335104674,0.820919794139797,1.,0.707106781186548,1.,0.707106781186548,
1.,0.707106781186548,1.,0.88618698704675,0.860825335104674),(0.860825335104674,
0.820919794139797,1.,0.707106781186548,1.,0.707106781186548,1.,0.707106781186548,
1.,0.88618698704675,0.860825335104674),(0.860825335104674,0.820919794139797,
1.,0.707106781186548,1.,0.707106781186548,1.,0.707106781186548,1.,0.88618698704675,
0.860825335104674),(0.860825335104674,0.820919794139797,1.,0.707106781186548,
1.,0.707106781186548,1.,0.707106781186548,1.,0.88618698704675,0.860825335104674),
(0.860825335104674,0.820919794139797,1.,0.707106781186548,1.,0.707106781186548,
1.,0.707106781186548,1.,0.88618698704675,0.860825335104674),(0.860825335104674,
0.820919794139797,1.,0.707106781186548,1.,0.707106781186548,1.,0.707106781186548,
1.,0.88618698704675,0.860825335104674),(0.860825335104674,0.820919794139797,
1.,0.707106781186548,1.,0.707106781186548,1.,0.707106781186548,1.,0.88618698704675,
0.860825335104674),(0.860825335104674,0.820919794139797,1.,0.707106781186548,
1.,0.707106781186548,1.,0.707106781186548,1.,0.88618698704675,0.860825335104674),
(0.860825335104674,0.820919794139797,1.,0.707106781186548,1.,0.707106781186548,
1.,0.707106781186548,1.,0.88618698704675,0.860825335104674),(0.860825335104674,
0.820919794139797,1.,0.707106781186548,1.,0.707106781186548,1.,0.707106781186548,
1.,0.88618698704675,0.860825335104674),(0.860825335104674,0.820919794139797,
1.,0.707106781186548,1.,0.707106781186548,1.,0.707106781186548,1.,0.88618698704675,
0.860825335104674),(0.860825335104674,0.820919794139797,1.,0.707106781186548,
1.,0.707106781186548,1.,0.707106781186548,1.,0.88618698704675,0.860825335104674)))
REPRESENTATION_ITEM('')
SURFACE()
);
#1098=STYLED_ITEM('',(#60527),#17349);
#1099=STYLED_ITEM('',(#60527),#17370);
#1100=STYLED_ITEM('',(#60527),#17371);
#1101=STYLED_ITEM('',(#60527),#17372);
#1102=STYLED_ITEM('',(#60527),#17374);
#1103=STYLED_ITEM('',(#60527),#17375);
#1104=STYLED_ITEM('',(#60527),#17376);
#1105=STYLED_ITEM('',(#60527),#17378);
#1106=STYLED_ITEM('',(#60527),#17379);
#1107=STYLED_ITEM('',(#60527),#17380);
#1108=STYLED_ITEM('',(#60527),#17382);
#1109=STYLED_ITEM('',(#60527),#17383);
#1110=STYLED_ITEM('',(#60527),#17384);
#1111=STYLED_ITEM('',(#60527),#17386);
#1112=STYLED_ITEM('',(#60527),#17387);
#1113=STYLED_ITEM('',(#60527),#17388);
#1114=STYLED_ITEM('',(#60527),#17390);
#1115=STYLED_ITEM('',(#60527),#17391);
#1116=STYLED_ITEM('',(#60527),#17392);
#1117=STYLED_ITEM('',(#60527),#17394);
#1118=STYLED_ITEM('',(#60527),#17395);
#1119=STYLED_ITEM('',(#60527),#17397);
#1120=STYLED_ITEM('',(#60527),#17398);
#1121=STYLED_ITEM('',(#60527),#17399);
#1122=STYLED_ITEM('',(#60527),#17401);
#1123=STYLED_ITEM('',(#60527),#17402);
#1124=STYLED_ITEM('',(#60527),#17403);
#1125=STYLED_ITEM('',(#60527),#17405);
#1126=STYLED_ITEM('',(#60527),#17406);
#1127=STYLED_ITEM('',(#60527),#17407);
#1128=STYLED_ITEM('',(#60527),#17409);
#1129=STYLED_ITEM('',(#60527),#17410);
#1130=STYLED_ITEM('',(#60527),#17411);
#1131=STYLED_ITEM('',(#60527),#17413);
#1132=STYLED_ITEM('',(#60527),#17414);
#1133=STYLED_ITEM('',(#60527),#17415);
#1134=STYLED_ITEM('',(#60527),#17417);
#1135=STYLED_ITEM('',(#60527),#17418);
#1136=STYLED_ITEM('',(#60527),#17420);
#1137=STYLED_ITEM('',(#60527),#17421);
#1138=STYLED_ITEM('',(#60527),#17423);
#1139=STYLED_ITEM('',(#60527),#17424);
#1140=STYLED_ITEM('',(#60527),#17426);
#1141=STYLED_ITEM('',(#60527),#17427);
#1142=STYLED_ITEM('',(#60527),#17429);
#1143=STYLED_ITEM('',(#60527),#17430);
#1144=STYLED_ITEM('',(#60527),#17432);
#1145=STYLED_ITEM('',(#60527),#17433);
#1146=STYLED_ITEM('',(#60527),#17435);
#1147=STYLED_ITEM('',(#60527),#17436);
#1148=STYLED_ITEM('',(#60527),#17438);
#1149=STYLED_ITEM('',(#60527),#17439);
#1150=STYLED_ITEM('',(#60527),#17441);
#1151=STYLED_ITEM('',(#60527),#17442);
#1152=STYLED_ITEM('',(#60527),#17444);
#1153=STYLED_ITEM('',(#60527),#17445);
#1154=STYLED_ITEM('',(#60527),#17447);
#1155=STYLED_ITEM('',(#60527),#17448);
#1156=STYLED_ITEM('',(#60527),#17450);
#1157=STYLED_ITEM('',(#60527),#17451);
#1158=STYLED_ITEM('',(#60527),#17460);
#1159=STYLED_ITEM('',(#60527),#17461);
#1160=STYLED_ITEM('',(#60527),#17465);
#1161=STYLED_ITEM('',(#60527),#17466);
#1162=STYLED_ITEM('',(#60527),#17470);
#1163=STYLED_ITEM('',(#60527),#17471);
#1164=STYLED_ITEM('',(#60527),#17475);
#1165=STYLED_ITEM('',(#60527),#17476);
#1166=STYLED_ITEM('',(#60527),#17480);
#1167=STYLED_ITEM('',(#60527),#17481);
#1168=STYLED_ITEM('',(#60527),#17484);
#1169=STYLED_ITEM('',(#60527),#17485);
#1170=STYLED_ITEM('',(#60527),#17487);
#1171=STYLED_ITEM('',(#60527),#17488);
#1172=STYLED_ITEM('',(#60527),#17490);
#1173=STYLED_ITEM('',(#60527),#17493);
#1174=STYLED_ITEM('',(#60527),#17495);
#1175=STYLED_ITEM('',(#60527),#17498);
#1176=STYLED_ITEM('',(#60527),#17500);
#1177=STYLED_ITEM('',(#60527),#17503);
#1178=STYLED_ITEM('',(#60527),#17505);
#1179=STYLED_ITEM('',(#60527),#17508);
#1180=STYLED_ITEM('',(#60527),#17510);
#1181=STYLED_ITEM('',(#60527),#17513);
#1182=STYLED_ITEM('',(#60527),#17515);
#1183=STYLED_ITEM('',(#60527),#17516);
#1184=STYLED_ITEM('',(#60527),#17517);
#1185=STYLED_ITEM('',(#60527),#17521);
#1186=STYLED_ITEM('',(#60527),#17522);
#1187=STYLED_ITEM('',(#60527),#17528);
#1188=STYLED_ITEM('',(#60527),#17529);
#1189=STYLED_ITEM('',(#60527),#17530);
#1190=STYLED_ITEM('',(#60527),#17531);
#1191=STYLED_ITEM('',(#60527),#17532);
#1192=STYLED_ITEM('',(#60527),#17533);
#1193=STYLED_ITEM('',(#60527),#17534);
#1194=STYLED_ITEM('',(#60527),#17535);
#1195=STYLED_ITEM('',(#60527),#17536);
#1196=STYLED_ITEM('',(#60527),#17537);
#1197=STYLED_ITEM('',(#60527),#17538);
#1198=STYLED_ITEM('',(#60527),#17539);
#1199=STYLED_ITEM('',(#60527),#17540);
#1200=STYLED_ITEM('',(#60527),#17541);
#1201=STYLED_ITEM('',(#60527),#17542);
#1202=STYLED_ITEM('',(#60527),#17543);
#1203=STYLED_ITEM('',(#60527),#17544);
#1204=STYLED_ITEM('',(#60527),#17545);
#1205=STYLED_ITEM('',(#60527),#17546);
#1206=STYLED_ITEM('',(#60527),#17547);
#1207=STYLED_ITEM('',(#60527),#17548);
#1208=STYLED_ITEM('',(#60527),#17549);
#1209=STYLED_ITEM('',(#60527),#17550);
#1210=STYLED_ITEM('',(#60527),#17551);
#1211=STYLED_ITEM('',(#60527),#17552);
#1212=STYLED_ITEM('',(#60527),#17553);
#1213=STYLED_ITEM('',(#60527),#17554);
#1214=STYLED_ITEM('',(#60527),#17555);
#1215=STYLED_ITEM('',(#60527),#17556);
#1216=STYLED_ITEM('',(#60527),#17557);
#1217=STYLED_ITEM('',(#60527),#17558);
#1218=STYLED_ITEM('',(#60527),#17559);
#1219=STYLED_ITEM('',(#60527),#17560);
#1220=STYLED_ITEM('',(#60527),#17561);
#1221=STYLED_ITEM('',(#60527),#17562);
#1222=STYLED_ITEM('',(#60527),#17563);
#1223=STYLED_ITEM('',(#60527),#17564);
#1224=STYLED_ITEM('',(#60527),#17565);
#1225=STYLED_ITEM('',(#60527),#17566);
#1226=STYLED_ITEM('',(#60527),#17567);
#1227=STYLED_ITEM('',(#60527),#17568);
#1228=STYLED_ITEM('',(#60527),#17569);
#1229=STYLED_ITEM('',(#60527),#17570);
#1230=STYLED_ITEM('',(#60527),#17571);
#1231=STYLED_ITEM('',(#60527),#17572);
#1232=STYLED_ITEM('',(#60527),#17578);
#1233=STYLED_ITEM('',(#60527),#17579);
#1234=STYLED_ITEM('',(#60527),#17580);
#1235=STYLED_ITEM('',(#60527),#17581);
#1236=STYLED_ITEM('',(#60527),#17582);
#1237=STYLED_ITEM('',(#60527),#17583);
#1238=STYLED_ITEM('',(#60527),#17584);
#1239=STYLED_ITEM('',(#60527),#17585);
#1240=STYLED_ITEM('',(#60527),#17586);
#1241=STYLED_ITEM('',(#60527),#17587);
#1242=STYLED_ITEM('',(#60527),#17588);
#1243=STYLED_ITEM('',(#60527),#17589);
#1244=STYLED_ITEM('',(#60527),#17590);
#1245=STYLED_ITEM('',(#60527),#17591);
#1246=STYLED_ITEM('',(#60527),#17592);
#1247=STYLED_ITEM('',(#60527),#17593);
#1248=STYLED_ITEM('',(#60527),#17594);
#1249=STYLED_ITEM('',(#60527),#17595);
#1250=STYLED_ITEM('',(#60527),#17596);
#1251=STYLED_ITEM('',(#60527),#17597);
#1252=STYLED_ITEM('',(#60527),#17598);
#1253=STYLED_ITEM('',(#60527),#17599);
#1254=STYLED_ITEM('',(#60527),#17600);
#1255=STYLED_ITEM('',(#60527),#17601);
#1256=STYLED_ITEM('',(#60527),#17602);
#1257=STYLED_ITEM('',(#60527),#17603);
#1258=STYLED_ITEM('',(#60527),#17604);
#1259=STYLED_ITEM('',(#60527),#17605);
#1260=STYLED_ITEM('',(#60527),#17606);
#1261=STYLED_ITEM('',(#60527),#17607);
#1262=STYLED_ITEM('',(#60527),#17608);
#1263=STYLED_ITEM('',(#60527),#17609);
#1264=STYLED_ITEM('',(#60527),#17610);
#1265=STYLED_ITEM('',(#60527),#17611);
#1266=STYLED_ITEM('',(#60527),#17612);
#1267=STYLED_ITEM('',(#60527),#17613);
#1268=STYLED_ITEM('',(#60527),#17614);
#1269=STYLED_ITEM('',(#60527),#17615);
#1270=STYLED_ITEM('',(#60527),#17616);
#1271=STYLED_ITEM('',(#60527),#17617);
#1272=STYLED_ITEM('',(#60527),#17618);
#1273=STYLED_ITEM('',(#60527),#17619);
#1274=STYLED_ITEM('',(#60527),#17620);
#1275=STYLED_ITEM('',(#60527),#17621);
#1276=STYLED_ITEM('',(#60527),#17622);
#1277=STYLED_ITEM('',(#60527),#17623);
#1278=STYLED_ITEM('',(#60527),#17624);
#1279=STYLED_ITEM('',(#60527),#17625);
#1280=STYLED_ITEM('',(#60527),#17626);
#1281=STYLED_ITEM('',(#60527),#17627);
#1282=STYLED_ITEM('',(#60527),#17628);
#1283=STYLED_ITEM('',(#60527),#17629);
#1284=STYLED_ITEM('',(#60527),#17630);
#1285=STYLED_ITEM('',(#60527),#17631);
#1286=STYLED_ITEM('',(#60527),#17632);
#1287=STYLED_ITEM('',(#60527),#17633);
#1288=STYLED_ITEM('',(#60527),#17634);
#1289=STYLED_ITEM('',(#60527),#17635);
#1290=STYLED_ITEM('',(#60527),#17636);
#1291=STYLED_ITEM('',(#60527),#17637);
#1292=STYLED_ITEM('',(#60527),#17638);
#1293=STYLED_ITEM('',(#60527),#17639);
#1294=STYLED_ITEM('',(#60527),#17640);
#1295=STYLED_ITEM('',(#60527),#87);
#1296=STYLED_ITEM('',(#60520),#88);
#1297=STYLED_ITEM('',(#60541),#89);
#1298=STYLED_ITEM('',(#60527),#90);
#1299=STYLED_ITEM('',(#60520),#91);
#1300=STYLED_ITEM('',(#60513),#92);
#1301=STYLED_ITEM('',(#60520),#93);
#1302=STYLED_ITEM('',(#60534),#94);
#1303=STYLED_ITEM('',(#60527),#95);
#1304=STYLED_ITEM('',(#60541),#96);
#1305=FACE_OUTER_BOUND('',#2269,.T.);
#1306=FACE_OUTER_BOUND('',#2270,.T.);
#1307=FACE_OUTER_BOUND('',#2271,.T.);
#1308=FACE_OUTER_BOUND('',#2272,.T.);
#1309=FACE_OUTER_BOUND('',#2273,.T.);
#1310=FACE_OUTER_BOUND('',#2274,.T.);
#1311=FACE_OUTER_BOUND('',#2275,.T.);
#1312=FACE_OUTER_BOUND('',#2276,.T.);
#1313=FACE_OUTER_BOUND('',#2277,.T.);
#1314=FACE_OUTER_BOUND('',#2278,.T.);
#1315=FACE_OUTER_BOUND('',#2279,.T.);
#1316=FACE_OUTER_BOUND('',#2280,.T.);
#1317=FACE_OUTER_BOUND('',#2281,.T.);
#1318=FACE_OUTER_BOUND('',#2282,.T.);
#1319=FACE_OUTER_BOUND('',#2283,.T.);
#1320=FACE_OUTER_BOUND('',#2284,.T.);
#1321=FACE_OUTER_BOUND('',#2285,.T.);
#1322=FACE_OUTER_BOUND('',#2286,.T.);
#1323=FACE_OUTER_BOUND('',#2287,.T.);
#1324=FACE_OUTER_BOUND('',#2288,.T.);
#1325=FACE_OUTER_BOUND('',#2289,.T.);
#1326=FACE_OUTER_BOUND('',#2290,.T.);
#1327=FACE_OUTER_BOUND('',#2291,.T.);
#1328=FACE_OUTER_BOUND('',#2292,.T.);
#1329=FACE_OUTER_BOUND('',#2293,.T.);
#1330=FACE_OUTER_BOUND('',#2294,.T.);
#1331=FACE_OUTER_BOUND('',#2295,.T.);
#1332=FACE_OUTER_BOUND('',#2296,.T.);
#1333=FACE_OUTER_BOUND('',#2297,.T.);
#1334=FACE_OUTER_BOUND('',#2298,.T.);
#1335=FACE_OUTER_BOUND('',#2299,.T.);
#1336=FACE_OUTER_BOUND('',#2300,.T.);
#1337=FACE_OUTER_BOUND('',#2301,.T.);
#1338=FACE_OUTER_BOUND('',#2302,.T.);
#1339=FACE_OUTER_BOUND('',#2303,.T.);
#1340=FACE_OUTER_BOUND('',#2304,.T.);
#1341=FACE_OUTER_BOUND('',#2306,.T.);
#1342=FACE_OUTER_BOUND('',#2307,.T.);
#1343=FACE_OUTER_BOUND('',#2308,.T.);
#1344=FACE_OUTER_BOUND('',#2309,.T.);
#1345=FACE_OUTER_BOUND('',#2310,.T.);
#1346=FACE_OUTER_BOUND('',#2311,.T.);
#1347=FACE_OUTER_BOUND('',#2312,.T.);
#1348=FACE_OUTER_BOUND('',#2313,.T.);
#1349=FACE_OUTER_BOUND('',#2314,.T.);
#1350=FACE_OUTER_BOUND('',#2315,.T.);
#1351=FACE_OUTER_BOUND('',#2316,.T.);
#1352=FACE_OUTER_BOUND('',#2317,.T.);
#1353=FACE_OUTER_BOUND('',#2318,.T.);
#1354=FACE_OUTER_BOUND('',#2319,.T.);
#1355=FACE_OUTER_BOUND('',#2320,.T.);
#1356=FACE_OUTER_BOUND('',#2321,.T.);
#1357=FACE_OUTER_BOUND('',#2322,.T.);
#1358=FACE_OUTER_BOUND('',#2323,.T.);
#1359=FACE_OUTER_BOUND('',#2324,.T.);
#1360=FACE_OUTER_BOUND('',#2325,.T.);
#1361=FACE_OUTER_BOUND('',#2326,.T.);
#1362=FACE_OUTER_BOUND('',#2327,.T.);
#1363=FACE_OUTER_BOUND('',#2328,.T.);
#1364=FACE_OUTER_BOUND('',#2329,.T.);
#1365=FACE_OUTER_BOUND('',#2330,.T.);
#1366=FACE_OUTER_BOUND('',#2331,.T.);
#1367=FACE_OUTER_BOUND('',#2332,.T.);
#1368=FACE_OUTER_BOUND('',#2333,.T.);
#1369=FACE_OUTER_BOUND('',#2334,.T.);
#1370=FACE_OUTER_BOUND('',#2335,.T.);
#1371=FACE_OUTER_BOUND('',#2336,.T.);
#1372=FACE_OUTER_BOUND('',#2337,.T.);
#1373=FACE_OUTER_BOUND('',#2338,.T.);
#1374=FACE_OUTER_BOUND('',#2339,.T.);
#1375=FACE_OUTER_BOUND('',#2340,.T.);
#1376=FACE_OUTER_BOUND('',#2341,.T.);
#1377=FACE_OUTER_BOUND('',#2342,.T.);
#1378=FACE_OUTER_BOUND('',#2343,.T.);
#1379=FACE_OUTER_BOUND('',#2344,.T.);
#1380=FACE_OUTER_BOUND('',#2345,.T.);
#1381=FACE_OUTER_BOUND('',#2346,.T.);
#1382=FACE_OUTER_BOUND('',#2347,.T.);
#1383=FACE_OUTER_BOUND('',#2348,.T.);
#1384=FACE_OUTER_BOUND('',#2349,.T.);
#1385=FACE_OUTER_BOUND('',#2350,.T.);
#1386=FACE_OUTER_BOUND('',#2351,.T.);
#1387=FACE_OUTER_BOUND('',#2352,.T.);
#1388=FACE_OUTER_BOUND('',#2353,.T.);
#1389=FACE_OUTER_BOUND('',#2354,.T.);
#1390=FACE_OUTER_BOUND('',#2355,.T.);
#1391=FACE_OUTER_BOUND('',#2356,.T.);
#1392=FACE_OUTER_BOUND('',#2357,.T.);
#1393=FACE_OUTER_BOUND('',#2358,.T.);
#1394=FACE_OUTER_BOUND('',#2359,.T.);
#1395=FACE_OUTER_BOUND('',#2360,.T.);
#1396=FACE_OUTER_BOUND('',#2361,.T.);
#1397=FACE_OUTER_BOUND('',#2362,.T.);
#1398=FACE_OUTER_BOUND('',#2363,.T.);
#1399=FACE_OUTER_BOUND('',#2364,.T.);
#1400=FACE_OUTER_BOUND('',#2365,.T.);
#1401=FACE_OUTER_BOUND('',#2366,.T.);
#1402=FACE_OUTER_BOUND('',#2367,.T.);
#1403=FACE_OUTER_BOUND('',#2368,.T.);
#1404=FACE_OUTER_BOUND('',#2369,.T.);
#1405=FACE_OUTER_BOUND('',#2370,.T.);
#1406=FACE_OUTER_BOUND('',#2371,.T.);
#1407=FACE_OUTER_BOUND('',#2372,.T.);
#1408=FACE_OUTER_BOUND('',#2373,.T.);
#1409=FACE_OUTER_BOUND('',#2374,.T.);
#1410=FACE_OUTER_BOUND('',#2375,.T.);
#1411=FACE_OUTER_BOUND('',#2376,.T.);
#1412=FACE_OUTER_BOUND('',#2377,.T.);
#1413=FACE_OUTER_BOUND('',#2378,.T.);
#1414=FACE_OUTER_BOUND('',#2379,.T.);
#1415=FACE_OUTER_BOUND('',#2380,.T.);
#1416=FACE_OUTER_BOUND('',#2381,.T.);
#1417=FACE_OUTER_BOUND('',#2382,.T.);
#1418=FACE_OUTER_BOUND('',#2383,.T.);
#1419=FACE_OUTER_BOUND('',#2384,.T.);
#1420=FACE_OUTER_BOUND('',#2385,.T.);
#1421=FACE_OUTER_BOUND('',#2386,.T.);
#1422=FACE_OUTER_BOUND('',#2387,.T.);
#1423=FACE_OUTER_BOUND('',#2388,.T.);
#1424=FACE_OUTER_BOUND('',#2389,.T.);
#1425=FACE_OUTER_BOUND('',#2390,.T.);
#1426=FACE_OUTER_BOUND('',#2392,.T.);
#1427=FACE_OUTER_BOUND('',#2393,.T.);
#1428=FACE_OUTER_BOUND('',#2394,.T.);
#1429=FACE_OUTER_BOUND('',#2396,.T.);
#1430=FACE_OUTER_BOUND('',#2397,.T.);
#1431=FACE_OUTER_BOUND('',#2398,.T.);
#1432=FACE_OUTER_BOUND('',#2399,.T.);
#1433=FACE_OUTER_BOUND('',#2400,.T.);
#1434=FACE_OUTER_BOUND('',#2401,.T.);
#1435=FACE_OUTER_BOUND('',#2402,.T.);
#1436=FACE_OUTER_BOUND('',#2403,.T.);
#1437=FACE_OUTER_BOUND('',#2404,.T.);
#1438=FACE_OUTER_BOUND('',#2405,.T.);
#1439=FACE_OUTER_BOUND('',#2406,.T.);
#1440=FACE_OUTER_BOUND('',#2407,.T.);
#1441=FACE_OUTER_BOUND('',#2408,.T.);
#1442=FACE_OUTER_BOUND('',#2409,.T.);
#1443=FACE_OUTER_BOUND('',#2410,.T.);
#1444=FACE_OUTER_BOUND('',#2411,.T.);
#1445=FACE_OUTER_BOUND('',#2412,.T.);
#1446=FACE_OUTER_BOUND('',#2413,.T.);
#1447=FACE_OUTER_BOUND('',#2414,.T.);
#1448=FACE_OUTER_BOUND('',#2415,.T.);
#1449=FACE_OUTER_BOUND('',#2416,.T.);
#1450=FACE_OUTER_BOUND('',#2417,.T.);
#1451=FACE_OUTER_BOUND('',#2418,.T.);
#1452=FACE_OUTER_BOUND('',#2419,.T.);
#1453=FACE_OUTER_BOUND('',#2420,.T.);
#1454=FACE_OUTER_BOUND('',#2421,.T.);
#1455=FACE_OUTER_BOUND('',#2422,.T.);
#1456=FACE_OUTER_BOUND('',#2423,.T.);
#1457=FACE_OUTER_BOUND('',#2425,.T.);
#1458=FACE_OUTER_BOUND('',#2426,.T.);
#1459=FACE_OUTER_BOUND('',#2427,.T.);
#1460=FACE_OUTER_BOUND('',#2428,.T.);
#1461=FACE_OUTER_BOUND('',#2429,.T.);
#1462=FACE_OUTER_BOUND('',#2430,.T.);
#1463=FACE_OUTER_BOUND('',#2431,.T.);
#1464=FACE_OUTER_BOUND('',#2432,.T.);
#1465=FACE_OUTER_BOUND('',#2433,.T.);
#1466=FACE_OUTER_BOUND('',#2434,.T.);
#1467=FACE_OUTER_BOUND('',#2435,.T.);
#1468=FACE_OUTER_BOUND('',#2436,.T.);
#1469=FACE_OUTER_BOUND('',#2437,.T.);
#1470=FACE_OUTER_BOUND('',#2438,.T.);
#1471=FACE_OUTER_BOUND('',#2439,.T.);
#1472=FACE_OUTER_BOUND('',#2440,.T.);
#1473=FACE_OUTER_BOUND('',#2441,.T.);
#1474=FACE_OUTER_BOUND('',#2442,.T.);
#1475=FACE_OUTER_BOUND('',#2443,.T.);
#1476=FACE_OUTER_BOUND('',#2444,.T.);
#1477=FACE_OUTER_BOUND('',#2445,.T.);
#1478=FACE_OUTER_BOUND('',#2446,.T.);
#1479=FACE_OUTER_BOUND('',#2447,.T.);
#1480=FACE_OUTER_BOUND('',#2448,.T.);
#1481=FACE_OUTER_BOUND('',#2449,.T.);
#1482=FACE_OUTER_BOUND('',#2450,.T.);
#1483=FACE_OUTER_BOUND('',#2451,.T.);
#1484=FACE_OUTER_BOUND('',#2452,.T.);
#1485=FACE_OUTER_BOUND('',#2453,.T.);
#1486=FACE_OUTER_BOUND('',#2454,.T.);
#1487=FACE_OUTER_BOUND('',#2455,.T.);
#1488=FACE_OUTER_BOUND('',#2456,.T.);
#1489=FACE_OUTER_BOUND('',#2457,.T.);
#1490=FACE_OUTER_BOUND('',#2458,.T.);
#1491=FACE_OUTER_BOUND('',#2459,.T.);
#1492=FACE_OUTER_BOUND('',#2460,.T.);
#1493=FACE_OUTER_BOUND('',#2461,.T.);
#1494=FACE_OUTER_BOUND('',#2462,.T.);
#1495=FACE_OUTER_BOUND('',#2463,.T.);
#1496=FACE_OUTER_BOUND('',#2464,.T.);
#1497=FACE_OUTER_BOUND('',#2465,.T.);
#1498=FACE_OUTER_BOUND('',#2466,.T.);
#1499=FACE_OUTER_BOUND('',#2467,.T.);
#1500=FACE_OUTER_BOUND('',#2468,.T.);
#1501=FACE_OUTER_BOUND('',#2469,.T.);
#1502=FACE_OUTER_BOUND('',#2470,.T.);
#1503=FACE_OUTER_BOUND('',#2471,.T.);
#1504=FACE_OUTER_BOUND('',#2472,.T.);
#1505=FACE_OUTER_BOUND('',#2473,.T.);
#1506=FACE_OUTER_BOUND('',#2474,.T.);
#1507=FACE_OUTER_BOUND('',#2475,.T.);
#1508=FACE_OUTER_BOUND('',#2476,.T.);
#1509=FACE_OUTER_BOUND('',#2477,.T.);
#1510=FACE_OUTER_BOUND('',#2478,.T.);
#1511=FACE_OUTER_BOUND('',#2479,.T.);
#1512=FACE_OUTER_BOUND('',#2480,.T.);
#1513=FACE_OUTER_BOUND('',#2481,.T.);
#1514=FACE_OUTER_BOUND('',#2482,.T.);
#1515=FACE_OUTER_BOUND('',#2483,.T.);
#1516=FACE_OUTER_BOUND('',#2484,.T.);
#1517=FACE_OUTER_BOUND('',#2485,.T.);
#1518=FACE_OUTER_BOUND('',#2486,.T.);
#1519=FACE_OUTER_BOUND('',#2487,.T.);
#1520=FACE_OUTER_BOUND('',#2488,.T.);
#1521=FACE_OUTER_BOUND('',#2489,.T.);
#1522=FACE_OUTER_BOUND('',#2490,.T.);
#1523=FACE_OUTER_BOUND('',#2491,.T.);
#1524=FACE_OUTER_BOUND('',#2492,.T.);
#1525=FACE_OUTER_BOUND('',#2493,.T.);
#1526=FACE_OUTER_BOUND('',#2494,.T.);
#1527=FACE_OUTER_BOUND('',#2495,.T.);
#1528=FACE_OUTER_BOUND('',#2496,.T.);
#1529=FACE_OUTER_BOUND('',#2497,.T.);
#1530=FACE_OUTER_BOUND('',#2498,.T.);
#1531=FACE_OUTER_BOUND('',#2499,.T.);
#1532=FACE_OUTER_BOUND('',#2500,.T.);
#1533=FACE_OUTER_BOUND('',#2501,.T.);
#1534=FACE_OUTER_BOUND('',#2502,.T.);
#1535=FACE_OUTER_BOUND('',#2503,.T.);
#1536=FACE_OUTER_BOUND('',#2504,.T.);
#1537=FACE_OUTER_BOUND('',#2505,.T.);
#1538=FACE_OUTER_BOUND('',#2506,.T.);
#1539=FACE_OUTER_BOUND('',#2507,.T.);
#1540=FACE_OUTER_BOUND('',#2508,.T.);
#1541=FACE_OUTER_BOUND('',#2509,.T.);
#1542=FACE_OUTER_BOUND('',#2510,.T.);
#1543=FACE_OUTER_BOUND('',#2511,.T.);
#1544=FACE_OUTER_BOUND('',#2512,.T.);
#1545=FACE_OUTER_BOUND('',#2513,.T.);
#1546=FACE_OUTER_BOUND('',#2514,.T.);
#1547=FACE_OUTER_BOUND('',#2516,.T.);
#1548=FACE_OUTER_BOUND('',#2518,.T.);
#1549=FACE_OUTER_BOUND('',#2519,.T.);
#1550=FACE_OUTER_BOUND('',#2520,.T.);
#1551=FACE_OUTER_BOUND('',#2521,.T.);
#1552=FACE_OUTER_BOUND('',#2522,.T.);
#1553=FACE_OUTER_BOUND('',#2523,.T.);
#1554=FACE_OUTER_BOUND('',#2524,.T.);
#1555=FACE_OUTER_BOUND('',#2525,.T.);
#1556=FACE_OUTER_BOUND('',#2526,.T.);
#1557=FACE_OUTER_BOUND('',#2527,.T.);
#1558=FACE_OUTER_BOUND('',#2528,.T.);
#1559=FACE_OUTER_BOUND('',#2529,.T.);
#1560=FACE_OUTER_BOUND('',#2530,.T.);
#1561=FACE_OUTER_BOUND('',#2531,.T.);
#1562=FACE_OUTER_BOUND('',#2532,.T.);
#1563=FACE_OUTER_BOUND('',#2533,.T.);
#1564=FACE_OUTER_BOUND('',#2534,.T.);
#1565=FACE_OUTER_BOUND('',#2535,.T.);
#1566=FACE_OUTER_BOUND('',#2536,.T.);
#1567=FACE_OUTER_BOUND('',#2537,.T.);
#1568=FACE_OUTER_BOUND('',#2538,.T.);
#1569=FACE_OUTER_BOUND('',#2539,.T.);
#1570=FACE_OUTER_BOUND('',#2540,.T.);
#1571=FACE_OUTER_BOUND('',#2541,.T.);
#1572=FACE_OUTER_BOUND('',#2542,.T.);
#1573=FACE_OUTER_BOUND('',#2543,.T.);
#1574=FACE_OUTER_BOUND('',#2544,.T.);
#1575=FACE_OUTER_BOUND('',#2545,.T.);
#1576=FACE_OUTER_BOUND('',#2546,.T.);
#1577=FACE_OUTER_BOUND('',#2547,.T.);
#1578=FACE_OUTER_BOUND('',#2548,.T.);
#1579=FACE_OUTER_BOUND('',#2549,.T.);
#1580=FACE_OUTER_BOUND('',#2550,.T.);
#1581=FACE_OUTER_BOUND('',#2551,.T.);
#1582=FACE_OUTER_BOUND('',#2552,.T.);
#1583=FACE_OUTER_BOUND('',#2553,.T.);
#1584=FACE_OUTER_BOUND('',#2554,.T.);
#1585=FACE_OUTER_BOUND('',#2555,.T.);
#1586=FACE_OUTER_BOUND('',#2556,.T.);
#1587=FACE_OUTER_BOUND('',#2557,.T.);
#1588=FACE_OUTER_BOUND('',#2558,.T.);
#1589=FACE_OUTER_BOUND('',#2559,.T.);
#1590=FACE_OUTER_BOUND('',#2560,.T.);
#1591=FACE_OUTER_BOUND('',#2561,.T.);
#1592=FACE_OUTER_BOUND('',#2562,.T.);
#1593=FACE_OUTER_BOUND('',#2563,.T.);
#1594=FACE_OUTER_BOUND('',#2564,.T.);
#1595=FACE_OUTER_BOUND('',#2565,.T.);
#1596=FACE_OUTER_BOUND('',#2566,.T.);
#1597=FACE_OUTER_BOUND('',#2567,.T.);
#1598=FACE_OUTER_BOUND('',#2568,.T.);
#1599=FACE_OUTER_BOUND('',#2569,.T.);
#1600=FACE_OUTER_BOUND('',#2570,.T.);
#1601=FACE_OUTER_BOUND('',#2571,.T.);
#1602=FACE_OUTER_BOUND('',#2572,.T.);
#1603=FACE_OUTER_BOUND('',#2573,.T.);
#1604=FACE_OUTER_BOUND('',#2574,.T.);
#1605=FACE_OUTER_BOUND('',#2575,.T.);
#1606=FACE_OUTER_BOUND('',#2576,.T.);
#1607=FACE_OUTER_BOUND('',#2577,.T.);
#1608=FACE_OUTER_BOUND('',#2578,.T.);
#1609=FACE_OUTER_BOUND('',#2579,.T.);
#1610=FACE_OUTER_BOUND('',#2580,.T.);
#1611=FACE_OUTER_BOUND('',#2581,.T.);
#1612=FACE_OUTER_BOUND('',#2582,.T.);
#1613=FACE_OUTER_BOUND('',#2584,.T.);
#1614=FACE_OUTER_BOUND('',#2585,.T.);
#1615=FACE_OUTER_BOUND('',#2586,.T.);
#1616=FACE_OUTER_BOUND('',#2587,.T.);
#1617=FACE_OUTER_BOUND('',#2588,.T.);
#1618=FACE_OUTER_BOUND('',#2590,.T.);
#1619=FACE_OUTER_BOUND('',#2591,.T.);
#1620=FACE_OUTER_BOUND('',#2592,.T.);
#1621=FACE_OUTER_BOUND('',#2593,.T.);
#1622=FACE_OUTER_BOUND('',#2594,.T.);
#1623=FACE_OUTER_BOUND('',#2596,.T.);
#1624=FACE_OUTER_BOUND('',#2597,.T.);
#1625=FACE_OUTER_BOUND('',#2598,.T.);
#1626=FACE_OUTER_BOUND('',#2599,.T.);
#1627=FACE_OUTER_BOUND('',#2600,.T.);
#1628=FACE_OUTER_BOUND('',#2601,.T.);
#1629=FACE_OUTER_BOUND('',#2602,.T.);
#1630=FACE_OUTER_BOUND('',#2603,.T.);
#1631=FACE_OUTER_BOUND('',#2604,.T.);
#1632=FACE_OUTER_BOUND('',#2605,.T.);
#1633=FACE_OUTER_BOUND('',#2606,.T.);
#1634=FACE_OUTER_BOUND('',#2607,.T.);
#1635=FACE_OUTER_BOUND('',#2608,.T.);
#1636=FACE_OUTER_BOUND('',#2609,.T.);
#1637=FACE_OUTER_BOUND('',#2610,.T.);
#1638=FACE_OUTER_BOUND('',#2611,.T.);
#1639=FACE_OUTER_BOUND('',#2612,.T.);
#1640=FACE_OUTER_BOUND('',#2613,.T.);
#1641=FACE_OUTER_BOUND('',#2614,.T.);
#1642=FACE_OUTER_BOUND('',#2615,.T.);
#1643=FACE_OUTER_BOUND('',#2616,.T.);
#1644=FACE_OUTER_BOUND('',#2617,.T.);
#1645=FACE_OUTER_BOUND('',#2618,.T.);
#1646=FACE_OUTER_BOUND('',#2620,.T.);
#1647=FACE_OUTER_BOUND('',#2621,.T.);
#1648=FACE_OUTER_BOUND('',#2622,.T.);
#1649=FACE_OUTER_BOUND('',#2623,.T.);
#1650=FACE_OUTER_BOUND('',#2625,.T.);
#1651=FACE_OUTER_BOUND('',#2626,.T.);
#1652=FACE_OUTER_BOUND('',#2628,.T.);
#1653=FACE_OUTER_BOUND('',#2629,.T.);
#1654=FACE_OUTER_BOUND('',#2640,.T.);
#1655=FACE_OUTER_BOUND('',#2641,.T.);
#1656=FACE_OUTER_BOUND('',#2642,.T.);
#1657=FACE_OUTER_BOUND('',#2643,.T.);
#1658=FACE_OUTER_BOUND('',#2644,.T.);
#1659=FACE_OUTER_BOUND('',#2645,.T.);
#1660=FACE_OUTER_BOUND('',#2656,.T.);
#1661=FACE_OUTER_BOUND('',#2657,.T.);
#1662=FACE_OUTER_BOUND('',#2658,.T.);
#1663=FACE_OUTER_BOUND('',#2659,.T.);
#1664=FACE_OUTER_BOUND('',#2660,.T.);
#1665=FACE_OUTER_BOUND('',#2661,.T.);
#1666=FACE_OUTER_BOUND('',#2662,.T.);
#1667=FACE_OUTER_BOUND('',#2663,.T.);
#1668=FACE_OUTER_BOUND('',#2664,.T.);
#1669=FACE_OUTER_BOUND('',#2665,.T.);
#1670=FACE_OUTER_BOUND('',#2666,.T.);
#1671=FACE_OUTER_BOUND('',#2667,.T.);
#1672=FACE_OUTER_BOUND('',#2668,.T.);
#1673=FACE_OUTER_BOUND('',#2669,.T.);
#1674=FACE_OUTER_BOUND('',#2670,.T.);
#1675=FACE_OUTER_BOUND('',#2671,.T.);
#1676=FACE_OUTER_BOUND('',#2672,.T.);
#1677=FACE_OUTER_BOUND('',#2673,.T.);
#1678=FACE_OUTER_BOUND('',#2674,.T.);
#1679=FACE_OUTER_BOUND('',#2675,.T.);
#1680=FACE_OUTER_BOUND('',#2676,.T.);
#1681=FACE_OUTER_BOUND('',#2677,.T.);
#1682=FACE_OUTER_BOUND('',#2678,.T.);
#1683=FACE_OUTER_BOUND('',#2679,.T.);
#1684=FACE_OUTER_BOUND('',#2680,.T.);
#1685=FACE_OUTER_BOUND('',#2681,.T.);
#1686=FACE_OUTER_BOUND('',#2682,.T.);
#1687=FACE_OUTER_BOUND('',#2683,.T.);
#1688=FACE_OUTER_BOUND('',#2684,.T.);
#1689=FACE_OUTER_BOUND('',#2685,.T.);
#1690=FACE_OUTER_BOUND('',#2686,.T.);
#1691=FACE_OUTER_BOUND('',#2687,.T.);
#1692=FACE_OUTER_BOUND('',#2688,.T.);
#1693=FACE_OUTER_BOUND('',#2689,.T.);
#1694=FACE_OUTER_BOUND('',#2690,.T.);
#1695=FACE_OUTER_BOUND('',#2691,.T.);
#1696=FACE_OUTER_BOUND('',#2692,.T.);
#1697=FACE_OUTER_BOUND('',#2693,.T.);
#1698=FACE_OUTER_BOUND('',#2694,.T.);
#1699=FACE_OUTER_BOUND('',#2695,.T.);
#1700=FACE_OUTER_BOUND('',#2696,.T.);
#1701=FACE_OUTER_BOUND('',#2697,.T.);
#1702=FACE_OUTER_BOUND('',#2698,.T.);
#1703=FACE_OUTER_BOUND('',#2699,.T.);
#1704=FACE_OUTER_BOUND('',#2700,.T.);
#1705=FACE_OUTER_BOUND('',#2701,.T.);
#1706=FACE_OUTER_BOUND('',#2702,.T.);
#1707=FACE_OUTER_BOUND('',#2703,.T.);
#1708=FACE_OUTER_BOUND('',#2704,.T.);
#1709=FACE_OUTER_BOUND('',#2705,.T.);
#1710=FACE_OUTER_BOUND('',#2706,.T.);
#1711=FACE_OUTER_BOUND('',#2707,.T.);
#1712=FACE_OUTER_BOUND('',#2708,.T.);
#1713=FACE_OUTER_BOUND('',#2709,.T.);
#1714=FACE_OUTER_BOUND('',#2710,.T.);
#1715=FACE_OUTER_BOUND('',#2711,.T.);
#1716=FACE_OUTER_BOUND('',#2712,.T.);
#1717=FACE_OUTER_BOUND('',#2713,.T.);
#1718=FACE_OUTER_BOUND('',#2714,.T.);
#1719=FACE_OUTER_BOUND('',#2715,.T.);
#1720=FACE_OUTER_BOUND('',#2716,.T.);
#1721=FACE_OUTER_BOUND('',#2717,.T.);
#1722=FACE_OUTER_BOUND('',#2718,.T.);
#1723=FACE_OUTER_BOUND('',#2719,.T.);
#1724=FACE_OUTER_BOUND('',#2720,.T.);
#1725=FACE_OUTER_BOUND('',#2721,.T.);
#1726=FACE_OUTER_BOUND('',#2722,.T.);
#1727=FACE_OUTER_BOUND('',#2723,.T.);
#1728=FACE_OUTER_BOUND('',#2724,.T.);
#1729=FACE_OUTER_BOUND('',#2725,.T.);
#1730=FACE_OUTER_BOUND('',#2726,.T.);
#1731=FACE_OUTER_BOUND('',#2727,.T.);
#1732=FACE_OUTER_BOUND('',#2728,.T.);
#1733=FACE_OUTER_BOUND('',#2729,.T.);
#1734=FACE_OUTER_BOUND('',#2730,.T.);
#1735=FACE_OUTER_BOUND('',#2731,.T.);
#1736=FACE_OUTER_BOUND('',#2732,.T.);
#1737=FACE_OUTER_BOUND('',#2733,.T.);
#1738=FACE_OUTER_BOUND('',#2734,.T.);
#1739=FACE_OUTER_BOUND('',#2735,.T.);
#1740=FACE_OUTER_BOUND('',#2736,.T.);
#1741=FACE_OUTER_BOUND('',#2737,.T.);
#1742=FACE_OUTER_BOUND('',#2738,.T.);
#1743=FACE_OUTER_BOUND('',#2739,.T.);
#1744=FACE_OUTER_BOUND('',#2740,.T.);
#1745=FACE_OUTER_BOUND('',#2741,.T.);
#1746=FACE_OUTER_BOUND('',#2742,.T.);
#1747=FACE_OUTER_BOUND('',#2743,.T.);
#1748=FACE_OUTER_BOUND('',#2744,.T.);
#1749=FACE_OUTER_BOUND('',#2745,.T.);
#1750=FACE_OUTER_BOUND('',#2746,.T.);
#1751=FACE_OUTER_BOUND('',#2747,.T.);
#1752=FACE_OUTER_BOUND('',#2748,.T.);
#1753=FACE_OUTER_BOUND('',#2749,.T.);
#1754=FACE_OUTER_BOUND('',#2750,.T.);
#1755=FACE_OUTER_BOUND('',#2751,.T.);
#1756=FACE_OUTER_BOUND('',#2752,.T.);
#1757=FACE_OUTER_BOUND('',#2753,.T.);
#1758=FACE_OUTER_BOUND('',#2754,.T.);
#1759=FACE_OUTER_BOUND('',#2755,.T.);
#1760=FACE_OUTER_BOUND('',#2756,.T.);
#1761=FACE_OUTER_BOUND('',#2757,.T.);
#1762=FACE_OUTER_BOUND('',#2758,.T.);
#1763=FACE_OUTER_BOUND('',#2759,.T.);
#1764=FACE_OUTER_BOUND('',#2760,.T.);
#1765=FACE_OUTER_BOUND('',#2761,.T.);
#1766=FACE_OUTER_BOUND('',#2762,.T.);
#1767=FACE_OUTER_BOUND('',#2763,.T.);
#1768=FACE_OUTER_BOUND('',#2764,.T.);
#1769=FACE_OUTER_BOUND('',#2765,.T.);
#1770=FACE_OUTER_BOUND('',#2766,.T.);
#1771=FACE_OUTER_BOUND('',#2767,.T.);
#1772=FACE_OUTER_BOUND('',#2768,.T.);
#1773=FACE_OUTER_BOUND('',#2769,.T.);
#1774=FACE_OUTER_BOUND('',#2770,.T.);
#1775=FACE_OUTER_BOUND('',#2771,.T.);
#1776=FACE_OUTER_BOUND('',#2772,.T.);
#1777=FACE_OUTER_BOUND('',#2773,.T.);
#1778=FACE_OUTER_BOUND('',#2774,.T.);
#1779=FACE_OUTER_BOUND('',#2775,.T.);
#1780=FACE_OUTER_BOUND('',#2776,.T.);
#1781=FACE_OUTER_BOUND('',#2777,.T.);
#1782=FACE_OUTER_BOUND('',#2778,.T.);
#1783=FACE_OUTER_BOUND('',#2779,.T.);
#1784=FACE_OUTER_BOUND('',#2780,.T.);
#1785=FACE_OUTER_BOUND('',#2781,.T.);
#1786=FACE_OUTER_BOUND('',#2782,.T.);
#1787=FACE_OUTER_BOUND('',#2783,.T.);
#1788=FACE_OUTER_BOUND('',#2784,.T.);
#1789=FACE_OUTER_BOUND('',#2785,.T.);
#1790=FACE_OUTER_BOUND('',#2786,.T.);
#1791=FACE_OUTER_BOUND('',#2787,.T.);
#1792=FACE_OUTER_BOUND('',#2788,.T.);
#1793=FACE_OUTER_BOUND('',#2789,.T.);
#1794=FACE_OUTER_BOUND('',#2790,.T.);
#1795=FACE_OUTER_BOUND('',#2791,.T.);
#1796=FACE_OUTER_BOUND('',#2792,.T.);
#1797=FACE_OUTER_BOUND('',#2793,.T.);
#1798=FACE_OUTER_BOUND('',#2794,.T.);
#1799=FACE_OUTER_BOUND('',#2795,.T.);
#1800=FACE_OUTER_BOUND('',#2796,.T.);
#1801=FACE_OUTER_BOUND('',#2797,.T.);
#1802=FACE_OUTER_BOUND('',#2798,.T.);
#1803=FACE_OUTER_BOUND('',#2799,.T.);
#1804=FACE_OUTER_BOUND('',#2800,.T.);
#1805=FACE_OUTER_BOUND('',#2801,.T.);
#1806=FACE_OUTER_BOUND('',#2802,.T.);
#1807=FACE_OUTER_BOUND('',#2803,.T.);
#1808=FACE_OUTER_BOUND('',#2804,.T.);
#1809=FACE_OUTER_BOUND('',#2805,.T.);
#1810=FACE_OUTER_BOUND('',#2806,.T.);
#1811=FACE_OUTER_BOUND('',#2807,.T.);
#1812=FACE_OUTER_BOUND('',#2808,.T.);
#1813=FACE_OUTER_BOUND('',#2809,.T.);
#1814=FACE_OUTER_BOUND('',#2810,.T.);
#1815=FACE_OUTER_BOUND('',#2811,.T.);
#1816=FACE_OUTER_BOUND('',#2812,.T.);
#1817=FACE_OUTER_BOUND('',#2813,.T.);
#1818=FACE_OUTER_BOUND('',#2814,.T.);
#1819=FACE_OUTER_BOUND('',#2815,.T.);
#1820=FACE_OUTER_BOUND('',#2816,.T.);
#1821=FACE_OUTER_BOUND('',#2817,.T.);
#1822=FACE_OUTER_BOUND('',#2818,.T.);
#1823=FACE_OUTER_BOUND('',#2819,.T.);
#1824=FACE_OUTER_BOUND('',#2820,.T.);
#1825=FACE_OUTER_BOUND('',#2821,.T.);
#1826=FACE_OUTER_BOUND('',#2822,.T.);
#1827=FACE_OUTER_BOUND('',#2823,.T.);
#1828=FACE_OUTER_BOUND('',#2824,.T.);
#1829=FACE_OUTER_BOUND('',#2825,.T.);
#1830=FACE_OUTER_BOUND('',#2826,.T.);
#1831=FACE_OUTER_BOUND('',#2827,.T.);
#1832=FACE_OUTER_BOUND('',#2828,.T.);
#1833=FACE_OUTER_BOUND('',#2829,.T.);
#1834=FACE_OUTER_BOUND('',#2830,.T.);
#1835=FACE_OUTER_BOUND('',#2831,.T.);
#1836=FACE_OUTER_BOUND('',#2832,.T.);
#1837=FACE_OUTER_BOUND('',#2833,.T.);
#1838=FACE_OUTER_BOUND('',#2834,.T.);
#1839=FACE_OUTER_BOUND('',#2835,.T.);
#1840=FACE_OUTER_BOUND('',#2836,.T.);
#1841=FACE_OUTER_BOUND('',#2837,.T.);
#1842=FACE_OUTER_BOUND('',#2838,.T.);
#1843=FACE_OUTER_BOUND('',#2839,.T.);
#1844=FACE_OUTER_BOUND('',#2840,.T.);
#1845=FACE_OUTER_BOUND('',#2841,.T.);
#1846=FACE_OUTER_BOUND('',#2842,.T.);
#1847=FACE_OUTER_BOUND('',#2843,.T.);
#1848=FACE_OUTER_BOUND('',#2844,.T.);
#1849=FACE_OUTER_BOUND('',#2845,.T.);
#1850=FACE_OUTER_BOUND('',#2846,.T.);
#1851=FACE_OUTER_BOUND('',#2847,.T.);
#1852=FACE_OUTER_BOUND('',#2848,.T.);
#1853=FACE_OUTER_BOUND('',#2849,.T.);
#1854=FACE_OUTER_BOUND('',#2850,.T.);
#1855=FACE_OUTER_BOUND('',#2851,.T.);
#1856=FACE_OUTER_BOUND('',#2852,.T.);
#1857=FACE_OUTER_BOUND('',#2853,.T.);
#1858=FACE_OUTER_BOUND('',#2854,.T.);
#1859=FACE_OUTER_BOUND('',#2855,.T.);
#1860=FACE_OUTER_BOUND('',#2856,.T.);
#1861=FACE_OUTER_BOUND('',#2857,.T.);
#1862=FACE_OUTER_BOUND('',#2858,.T.);
#1863=FACE_OUTER_BOUND('',#2859,.T.);
#1864=FACE_OUTER_BOUND('',#2860,.T.);
#1865=FACE_OUTER_BOUND('',#2861,.T.);
#1866=FACE_OUTER_BOUND('',#2862,.T.);
#1867=FACE_OUTER_BOUND('',#2863,.T.);
#1868=FACE_OUTER_BOUND('',#2865,.T.);
#1869=FACE_OUTER_BOUND('',#2867,.T.);
#1870=FACE_OUTER_BOUND('',#2868,.T.);
#1871=FACE_OUTER_BOUND('',#2869,.T.);
#1872=FACE_OUTER_BOUND('',#2870,.T.);
#1873=FACE_OUTER_BOUND('',#2878,.T.);
#1874=FACE_OUTER_BOUND('',#2879,.T.);
#1875=FACE_OUTER_BOUND('',#2880,.T.);
#1876=FACE_OUTER_BOUND('',#2881,.T.);
#1877=FACE_OUTER_BOUND('',#2883,.T.);
#1878=FACE_OUTER_BOUND('',#2884,.T.);
#1879=FACE_OUTER_BOUND('',#2885,.T.);
#1880=FACE_OUTER_BOUND('',#2886,.T.);
#1881=FACE_OUTER_BOUND('',#2888,.T.);
#1882=FACE_OUTER_BOUND('',#2889,.T.);
#1883=FACE_OUTER_BOUND('',#2890,.T.);
#1884=FACE_OUTER_BOUND('',#2891,.T.);
#1885=FACE_OUTER_BOUND('',#2893,.T.);
#1886=FACE_OUTER_BOUND('',#2894,.T.);
#1887=FACE_OUTER_BOUND('',#2895,.T.);
#1888=FACE_OUTER_BOUND('',#2896,.T.);
#1889=FACE_OUTER_BOUND('',#2897,.T.);
#1890=FACE_OUTER_BOUND('',#2898,.T.);
#1891=FACE_OUTER_BOUND('',#2899,.T.);
#1892=FACE_OUTER_BOUND('',#2900,.T.);
#1893=FACE_OUTER_BOUND('',#2901,.T.);
#1894=FACE_OUTER_BOUND('',#2902,.T.);
#1895=FACE_OUTER_BOUND('',#2903,.T.);
#1896=FACE_OUTER_BOUND('',#2904,.T.);
#1897=FACE_OUTER_BOUND('',#2905,.T.);
#1898=FACE_OUTER_BOUND('',#2906,.T.);
#1899=FACE_OUTER_BOUND('',#2907,.T.);
#1900=FACE_OUTER_BOUND('',#2908,.T.);
#1901=FACE_OUTER_BOUND('',#2909,.T.);
#1902=FACE_OUTER_BOUND('',#2910,.T.);
#1903=FACE_OUTER_BOUND('',#2911,.T.);
#1904=FACE_OUTER_BOUND('',#2912,.T.);
#1905=FACE_OUTER_BOUND('',#2913,.T.);
#1906=FACE_OUTER_BOUND('',#2914,.T.);
#1907=FACE_OUTER_BOUND('',#2915,.T.);
#1908=FACE_OUTER_BOUND('',#2916,.T.);
#1909=FACE_OUTER_BOUND('',#2917,.T.);
#1910=FACE_OUTER_BOUND('',#2918,.T.);
#1911=FACE_OUTER_BOUND('',#2919,.T.);
#1912=FACE_OUTER_BOUND('',#2920,.T.);
#1913=FACE_OUTER_BOUND('',#2921,.T.);
#1914=FACE_OUTER_BOUND('',#2923,.T.);
#1915=FACE_OUTER_BOUND('',#2924,.T.);
#1916=FACE_OUTER_BOUND('',#2926,.T.);
#1917=FACE_OUTER_BOUND('',#2927,.T.);
#1918=FACE_OUTER_BOUND('',#2928,.T.);
#1919=FACE_OUTER_BOUND('',#2929,.T.);
#1920=FACE_OUTER_BOUND('',#2930,.T.);
#1921=FACE_OUTER_BOUND('',#2931,.T.);
#1922=FACE_OUTER_BOUND('',#2932,.T.);
#1923=FACE_OUTER_BOUND('',#2933,.T.);
#1924=FACE_OUTER_BOUND('',#2934,.T.);
#1925=FACE_OUTER_BOUND('',#2935,.T.);
#1926=FACE_OUTER_BOUND('',#2936,.T.);
#1927=FACE_OUTER_BOUND('',#2937,.T.);
#1928=FACE_OUTER_BOUND('',#2938,.T.);
#1929=FACE_OUTER_BOUND('',#2939,.T.);
#1930=FACE_OUTER_BOUND('',#2940,.T.);
#1931=FACE_OUTER_BOUND('',#2941,.T.);
#1932=FACE_OUTER_BOUND('',#2942,.T.);
#1933=FACE_OUTER_BOUND('',#2943,.T.);
#1934=FACE_OUTER_BOUND('',#2944,.T.);
#1935=FACE_OUTER_BOUND('',#2945,.T.);
#1936=FACE_OUTER_BOUND('',#2946,.T.);
#1937=FACE_OUTER_BOUND('',#2947,.T.);
#1938=FACE_OUTER_BOUND('',#2948,.T.);
#1939=FACE_OUTER_BOUND('',#2949,.T.);
#1940=FACE_OUTER_BOUND('',#2950,.T.);
#1941=FACE_OUTER_BOUND('',#2951,.T.);
#1942=FACE_OUTER_BOUND('',#2952,.T.);
#1943=FACE_OUTER_BOUND('',#2953,.T.);
#1944=FACE_OUTER_BOUND('',#2954,.T.);
#1945=FACE_OUTER_BOUND('',#2955,.T.);
#1946=FACE_OUTER_BOUND('',#2956,.T.);
#1947=FACE_OUTER_BOUND('',#2957,.T.);
#1948=FACE_OUTER_BOUND('',#2958,.T.);
#1949=FACE_OUTER_BOUND('',#2959,.T.);
#1950=FACE_OUTER_BOUND('',#2960,.T.);
#1951=FACE_OUTER_BOUND('',#2961,.T.);
#1952=FACE_OUTER_BOUND('',#2962,.T.);
#1953=FACE_OUTER_BOUND('',#2963,.T.);
#1954=FACE_OUTER_BOUND('',#2964,.T.);
#1955=FACE_OUTER_BOUND('',#2965,.T.);
#1956=FACE_OUTER_BOUND('',#2966,.T.);
#1957=FACE_OUTER_BOUND('',#2967,.T.);
#1958=FACE_OUTER_BOUND('',#2968,.T.);
#1959=FACE_OUTER_BOUND('',#2969,.T.);
#1960=FACE_OUTER_BOUND('',#2970,.T.);
#1961=FACE_OUTER_BOUND('',#2971,.T.);
#1962=FACE_OUTER_BOUND('',#2972,.T.);
#1963=FACE_OUTER_BOUND('',#2973,.T.);
#1964=FACE_OUTER_BOUND('',#2974,.T.);
#1965=FACE_OUTER_BOUND('',#2975,.T.);
#1966=FACE_OUTER_BOUND('',#2976,.T.);
#1967=FACE_OUTER_BOUND('',#2977,.T.);
#1968=FACE_OUTER_BOUND('',#2978,.T.);
#1969=FACE_OUTER_BOUND('',#2979,.T.);
#1970=FACE_OUTER_BOUND('',#2980,.T.);
#1971=FACE_OUTER_BOUND('',#2981,.T.);
#1972=FACE_OUTER_BOUND('',#2982,.T.);
#1973=FACE_OUTER_BOUND('',#2983,.T.);
#1974=FACE_OUTER_BOUND('',#2984,.T.);
#1975=FACE_OUTER_BOUND('',#2985,.T.);
#1976=FACE_OUTER_BOUND('',#2986,.T.);
#1977=FACE_OUTER_BOUND('',#2987,.T.);
#1978=FACE_OUTER_BOUND('',#2988,.T.);
#1979=FACE_OUTER_BOUND('',#2989,.T.);
#1980=FACE_OUTER_BOUND('',#2990,.T.);
#1981=FACE_OUTER_BOUND('',#2991,.T.);
#1982=FACE_OUTER_BOUND('',#2992,.T.);
#1983=FACE_OUTER_BOUND('',#2993,.T.);
#1984=FACE_OUTER_BOUND('',#2994,.T.);
#1985=FACE_OUTER_BOUND('',#2995,.T.);
#1986=FACE_OUTER_BOUND('',#2996,.T.);
#1987=FACE_OUTER_BOUND('',#2997,.T.);
#1988=FACE_OUTER_BOUND('',#2998,.T.);
#1989=FACE_OUTER_BOUND('',#2999,.T.);
#1990=FACE_OUTER_BOUND('',#3000,.T.);
#1991=FACE_OUTER_BOUND('',#3001,.T.);
#1992=FACE_OUTER_BOUND('',#3002,.T.);
#1993=FACE_OUTER_BOUND('',#3003,.T.);
#1994=FACE_OUTER_BOUND('',#3004,.T.);
#1995=FACE_OUTER_BOUND('',#3005,.T.);
#1996=FACE_OUTER_BOUND('',#3006,.T.);
#1997=FACE_OUTER_BOUND('',#3007,.T.);
#1998=FACE_OUTER_BOUND('',#3008,.T.);
#1999=FACE_OUTER_BOUND('',#3009,.T.);
#2000=FACE_OUTER_BOUND('',#3010,.T.);
#2001=FACE_OUTER_BOUND('',#3011,.T.);
#2002=FACE_OUTER_BOUND('',#3012,.T.);
#2003=FACE_OUTER_BOUND('',#3013,.T.);
#2004=FACE_OUTER_BOUND('',#3014,.T.);
#2005=FACE_OUTER_BOUND('',#3015,.T.);
#2006=FACE_OUTER_BOUND('',#3016,.T.);
#2007=FACE_OUTER_BOUND('',#3017,.T.);
#2008=FACE_OUTER_BOUND('',#3018,.T.);
#2009=FACE_OUTER_BOUND('',#3019,.T.);
#2010=FACE_OUTER_BOUND('',#3020,.T.);
#2011=FACE_OUTER_BOUND('',#3021,.T.);
#2012=FACE_OUTER_BOUND('',#3022,.T.);
#2013=FACE_OUTER_BOUND('',#3023,.T.);
#2014=FACE_OUTER_BOUND('',#3024,.T.);
#2015=FACE_OUTER_BOUND('',#3025,.T.);
#2016=FACE_OUTER_BOUND('',#3026,.T.);
#2017=FACE_OUTER_BOUND('',#3027,.T.);
#2018=FACE_OUTER_BOUND('',#3028,.T.);
#2019=FACE_OUTER_BOUND('',#3029,.T.);
#2020=FACE_OUTER_BOUND('',#3030,.T.);
#2021=FACE_OUTER_BOUND('',#3031,.T.);
#2022=FACE_OUTER_BOUND('',#3032,.T.);
#2023=FACE_OUTER_BOUND('',#3033,.T.);
#2024=FACE_OUTER_BOUND('',#3034,.T.);
#2025=FACE_OUTER_BOUND('',#3035,.T.);
#2026=FACE_OUTER_BOUND('',#3036,.T.);
#2027=FACE_OUTER_BOUND('',#3037,.T.);
#2028=FACE_OUTER_BOUND('',#3038,.T.);
#2029=FACE_OUTER_BOUND('',#3039,.T.);
#2030=FACE_OUTER_BOUND('',#3040,.T.);
#2031=FACE_OUTER_BOUND('',#3041,.T.);
#2032=FACE_OUTER_BOUND('',#3042,.T.);
#2033=FACE_OUTER_BOUND('',#3043,.T.);
#2034=FACE_OUTER_BOUND('',#3044,.T.);
#2035=FACE_OUTER_BOUND('',#3045,.T.);
#2036=FACE_OUTER_BOUND('',#3046,.T.);
#2037=FACE_OUTER_BOUND('',#3047,.T.);
#2038=FACE_OUTER_BOUND('',#3048,.T.);
#2039=FACE_OUTER_BOUND('',#3049,.T.);
#2040=FACE_OUTER_BOUND('',#3050,.T.);
#2041=FACE_OUTER_BOUND('',#3051,.T.);
#2042=FACE_OUTER_BOUND('',#3052,.T.);
#2043=FACE_OUTER_BOUND('',#3053,.T.);
#2044=FACE_OUTER_BOUND('',#3054,.T.);
#2045=FACE_OUTER_BOUND('',#3055,.T.);
#2046=FACE_OUTER_BOUND('',#3056,.T.);
#2047=FACE_OUTER_BOUND('',#3057,.T.);
#2048=FACE_OUTER_BOUND('',#3058,.T.);
#2049=FACE_OUTER_BOUND('',#3059,.T.);
#2050=FACE_OUTER_BOUND('',#3060,.T.);
#2051=FACE_OUTER_BOUND('',#3061,.T.);
#2052=FACE_OUTER_BOUND('',#3062,.T.);
#2053=FACE_OUTER_BOUND('',#3063,.T.);
#2054=FACE_OUTER_BOUND('',#3064,.T.);
#2055=FACE_OUTER_BOUND('',#3065,.T.);
#2056=FACE_OUTER_BOUND('',#3066,.T.);
#2057=FACE_OUTER_BOUND('',#3067,.T.);
#2058=FACE_OUTER_BOUND('',#3068,.T.);
#2059=FACE_OUTER_BOUND('',#3070,.T.);
#2060=FACE_OUTER_BOUND('',#3071,.T.);
#2061=FACE_OUTER_BOUND('',#3072,.T.);
#2062=FACE_OUTER_BOUND('',#3073,.T.);
#2063=FACE_OUTER_BOUND('',#3074,.T.);
#2064=FACE_OUTER_BOUND('',#3075,.T.);
#2065=FACE_OUTER_BOUND('',#3076,.T.);
#2066=FACE_OUTER_BOUND('',#3077,.T.);
#2067=FACE_OUTER_BOUND('',#3078,.T.);
#2068=FACE_OUTER_BOUND('',#3079,.T.);
#2069=FACE_OUTER_BOUND('',#3080,.T.);
#2070=FACE_OUTER_BOUND('',#3081,.T.);
#2071=FACE_OUTER_BOUND('',#3082,.T.);
#2072=FACE_OUTER_BOUND('',#3083,.T.);
#2073=FACE_OUTER_BOUND('',#3084,.T.);
#2074=FACE_OUTER_BOUND('',#3085,.T.);
#2075=FACE_OUTER_BOUND('',#3086,.T.);
#2076=FACE_OUTER_BOUND('',#3087,.T.);
#2077=FACE_OUTER_BOUND('',#3088,.T.);
#2078=FACE_OUTER_BOUND('',#3089,.T.);
#2079=FACE_OUTER_BOUND('',#3091,.T.);
#2080=FACE_OUTER_BOUND('',#3092,.T.);
#2081=FACE_OUTER_BOUND('',#3093,.T.);
#2082=FACE_OUTER_BOUND('',#3094,.T.);
#2083=FACE_OUTER_BOUND('',#3096,.T.);
#2084=FACE_OUTER_BOUND('',#3097,.T.);
#2085=FACE_OUTER_BOUND('',#3098,.T.);
#2086=FACE_OUTER_BOUND('',#3099,.T.);
#2087=FACE_OUTER_BOUND('',#3100,.T.);
#2088=FACE_OUTER_BOUND('',#3101,.T.);
#2089=FACE_OUTER_BOUND('',#3102,.T.);
#2090=FACE_OUTER_BOUND('',#3103,.T.);
#2091=FACE_OUTER_BOUND('',#3104,.T.);
#2092=FACE_OUTER_BOUND('',#3105,.T.);
#2093=FACE_OUTER_BOUND('',#3106,.T.);
#2094=FACE_OUTER_BOUND('',#3107,.T.);
#2095=FACE_OUTER_BOUND('',#3108,.T.);
#2096=FACE_OUTER_BOUND('',#3109,.T.);
#2097=FACE_OUTER_BOUND('',#3110,.T.);
#2098=FACE_OUTER_BOUND('',#3111,.T.);
#2099=FACE_OUTER_BOUND('',#3112,.T.);
#2100=FACE_OUTER_BOUND('',#3116,.T.);
#2101=FACE_OUTER_BOUND('',#3118,.T.);
#2102=FACE_OUTER_BOUND('',#3120,.T.);
#2103=FACE_OUTER_BOUND('',#3121,.T.);
#2104=FACE_OUTER_BOUND('',#3122,.T.);
#2105=FACE_OUTER_BOUND('',#3123,.T.);
#2106=FACE_OUTER_BOUND('',#3124,.T.);
#2107=FACE_OUTER_BOUND('',#3126,.T.);
#2108=FACE_OUTER_BOUND('',#3127,.T.);
#2109=FACE_OUTER_BOUND('',#3135,.T.);
#2110=FACE_OUTER_BOUND('',#3136,.T.);
#2111=FACE_OUTER_BOUND('',#3138,.T.);
#2112=FACE_OUTER_BOUND('',#3139,.T.);
#2113=FACE_OUTER_BOUND('',#3140,.T.);
#2114=FACE_OUTER_BOUND('',#3143,.T.);
#2115=FACE_OUTER_BOUND('',#3144,.T.);
#2116=FACE_OUTER_BOUND('',#3147,.T.);
#2117=FACE_OUTER_BOUND('',#3148,.T.);
#2118=FACE_OUTER_BOUND('',#3149,.T.);
#2119=FACE_OUTER_BOUND('',#3150,.T.);
#2120=FACE_OUTER_BOUND('',#3151,.T.);
#2121=FACE_OUTER_BOUND('',#3152,.T.);
#2122=FACE_OUTER_BOUND('',#3153,.T.);
#2123=FACE_OUTER_BOUND('',#3154,.T.);
#2124=FACE_OUTER_BOUND('',#3155,.T.);
#2125=FACE_OUTER_BOUND('',#3156,.T.);
#2126=FACE_OUTER_BOUND('',#3157,.T.);
#2127=FACE_OUTER_BOUND('',#3158,.T.);
#2128=FACE_OUTER_BOUND('',#3159,.T.);
#2129=FACE_OUTER_BOUND('',#3160,.T.);
#2130=FACE_OUTER_BOUND('',#3161,.T.);
#2131=FACE_OUTER_BOUND('',#3162,.T.);
#2132=FACE_OUTER_BOUND('',#3163,.T.);
#2133=FACE_OUTER_BOUND('',#3164,.T.);
#2134=FACE_OUTER_BOUND('',#3165,.T.);
#2135=FACE_OUTER_BOUND('',#3166,.T.);
#2136=FACE_OUTER_BOUND('',#3167,.T.);
#2137=FACE_OUTER_BOUND('',#3168,.T.);
#2138=FACE_OUTER_BOUND('',#3169,.T.);
#2139=FACE_OUTER_BOUND('',#3170,.T.);
#2140=FACE_OUTER_BOUND('',#3171,.T.);
#2141=FACE_OUTER_BOUND('',#3172,.T.);
#2142=FACE_OUTER_BOUND('',#3173,.T.);
#2143=FACE_OUTER_BOUND('',#3174,.T.);
#2144=FACE_OUTER_BOUND('',#3175,.T.);
#2145=FACE_OUTER_BOUND('',#3176,.T.);
#2146=FACE_OUTER_BOUND('',#3177,.T.);
#2147=FACE_OUTER_BOUND('',#3178,.T.);
#2148=FACE_OUTER_BOUND('',#3179,.T.);
#2149=FACE_OUTER_BOUND('',#3180,.T.);
#2150=FACE_OUTER_BOUND('',#3181,.T.);
#2151=FACE_OUTER_BOUND('',#3182,.T.);
#2152=FACE_OUTER_BOUND('',#3183,.T.);
#2153=FACE_OUTER_BOUND('',#3184,.T.);
#2154=FACE_OUTER_BOUND('',#3185,.T.);
#2155=FACE_OUTER_BOUND('',#3186,.T.);
#2156=FACE_OUTER_BOUND('',#3187,.T.);
#2157=FACE_OUTER_BOUND('',#3188,.T.);
#2158=FACE_OUTER_BOUND('',#3189,.T.);
#2159=FACE_OUTER_BOUND('',#3190,.T.);
#2160=FACE_OUTER_BOUND('',#3191,.T.);
#2161=FACE_OUTER_BOUND('',#3192,.T.);
#2162=FACE_OUTER_BOUND('',#3193,.T.);
#2163=FACE_OUTER_BOUND('',#3194,.T.);
#2164=FACE_OUTER_BOUND('',#3195,.T.);
#2165=FACE_OUTER_BOUND('',#3196,.T.);
#2166=FACE_OUTER_BOUND('',#3197,.T.);
#2167=FACE_OUTER_BOUND('',#3198,.T.);
#2168=FACE_OUTER_BOUND('',#3199,.T.);
#2169=FACE_OUTER_BOUND('',#3200,.T.);
#2170=FACE_OUTER_BOUND('',#3201,.T.);
#2171=FACE_OUTER_BOUND('',#3202,.T.);
#2172=FACE_OUTER_BOUND('',#3203,.T.);
#2173=FACE_OUTER_BOUND('',#3204,.T.);
#2174=FACE_OUTER_BOUND('',#3205,.T.);
#2175=FACE_OUTER_BOUND('',#3206,.T.);
#2176=FACE_OUTER_BOUND('',#3207,.T.);
#2177=FACE_OUTER_BOUND('',#3208,.T.);
#2178=FACE_OUTER_BOUND('',#3209,.T.);
#2179=FACE_OUTER_BOUND('',#3210,.T.);
#2180=FACE_OUTER_BOUND('',#3211,.T.);
#2181=FACE_OUTER_BOUND('',#3212,.T.);
#2182=FACE_OUTER_BOUND('',#3213,.T.);
#2183=FACE_OUTER_BOUND('',#3214,.T.);
#2184=FACE_OUTER_BOUND('',#3215,.T.);
#2185=FACE_OUTER_BOUND('',#3216,.T.);
#2186=FACE_OUTER_BOUND('',#3217,.T.);
#2187=FACE_OUTER_BOUND('',#3218,.T.);
#2188=FACE_OUTER_BOUND('',#3219,.T.);
#2189=FACE_OUTER_BOUND('',#3220,.T.);
#2190=FACE_OUTER_BOUND('',#3221,.T.);
#2191=FACE_OUTER_BOUND('',#3222,.T.);
#2192=FACE_OUTER_BOUND('',#3223,.T.);
#2193=FACE_OUTER_BOUND('',#3224,.T.);
#2194=FACE_OUTER_BOUND('',#3225,.T.);
#2195=FACE_OUTER_BOUND('',#3226,.T.);
#2196=FACE_OUTER_BOUND('',#3227,.T.);
#2197=FACE_OUTER_BOUND('',#3228,.T.);
#2198=FACE_OUTER_BOUND('',#3229,.T.);
#2199=FACE_OUTER_BOUND('',#3230,.T.);
#2200=FACE_OUTER_BOUND('',#3231,.T.);
#2201=FACE_OUTER_BOUND('',#3232,.T.);
#2202=FACE_OUTER_BOUND('',#3233,.T.);
#2203=FACE_OUTER_BOUND('',#3234,.T.);
#2204=FACE_OUTER_BOUND('',#3235,.T.);
#2205=FACE_OUTER_BOUND('',#3236,.T.);
#2206=FACE_OUTER_BOUND('',#3237,.T.);
#2207=FACE_OUTER_BOUND('',#3238,.T.);
#2208=FACE_OUTER_BOUND('',#3239,.T.);
#2209=FACE_OUTER_BOUND('',#3240,.T.);
#2210=FACE_OUTER_BOUND('',#3241,.T.);
#2211=FACE_OUTER_BOUND('',#3242,.T.);
#2212=FACE_OUTER_BOUND('',#3243,.T.);
#2213=FACE_OUTER_BOUND('',#3244,.T.);
#2214=FACE_OUTER_BOUND('',#3245,.T.);
#2215=FACE_OUTER_BOUND('',#3246,.T.);
#2216=FACE_OUTER_BOUND('',#3247,.T.);
#2217=FACE_OUTER_BOUND('',#3248,.T.);
#2218=FACE_OUTER_BOUND('',#3249,.T.);
#2219=FACE_OUTER_BOUND('',#3250,.T.);
#2220=FACE_OUTER_BOUND('',#3251,.T.);
#2221=FACE_OUTER_BOUND('',#3252,.T.);
#2222=FACE_OUTER_BOUND('',#3253,.T.);
#2223=FACE_OUTER_BOUND('',#3254,.T.);
#2224=FACE_OUTER_BOUND('',#3255,.T.);
#2225=FACE_OUTER_BOUND('',#3256,.T.);
#2226=FACE_OUTER_BOUND('',#3257,.T.);
#2227=FACE_OUTER_BOUND('',#3258,.T.);
#2228=FACE_OUTER_BOUND('',#3259,.T.);
#2229=FACE_OUTER_BOUND('',#3260,.T.);
#2230=FACE_OUTER_BOUND('',#3261,.T.);
#2231=FACE_OUTER_BOUND('',#3262,.T.);
#2232=FACE_OUTER_BOUND('',#3263,.T.);
#2233=FACE_OUTER_BOUND('',#3264,.T.);
#2234=FACE_OUTER_BOUND('',#3265,.T.);
#2235=FACE_OUTER_BOUND('',#3266,.T.);
#2236=FACE_OUTER_BOUND('',#3267,.T.);
#2237=FACE_OUTER_BOUND('',#3268,.T.);
#2238=FACE_OUTER_BOUND('',#3269,.T.);
#2239=FACE_OUTER_BOUND('',#3270,.T.);
#2240=FACE_OUTER_BOUND('',#3271,.T.);
#2241=FACE_OUTER_BOUND('',#3272,.T.);
#2242=FACE_OUTER_BOUND('',#3273,.T.);
#2243=FACE_OUTER_BOUND('',#3274,.T.);
#2244=FACE_OUTER_BOUND('',#3275,.T.);
#2245=FACE_OUTER_BOUND('',#3276,.T.);
#2246=FACE_OUTER_BOUND('',#3277,.T.);
#2247=FACE_OUTER_BOUND('',#3278,.T.);
#2248=FACE_OUTER_BOUND('',#3279,.T.);
#2249=FACE_OUTER_BOUND('',#3280,.T.);
#2250=FACE_OUTER_BOUND('',#3281,.T.);
#2251=FACE_OUTER_BOUND('',#3282,.T.);
#2252=FACE_OUTER_BOUND('',#3283,.T.);
#2253=FACE_OUTER_BOUND('',#3284,.T.);
#2254=FACE_OUTER_BOUND('',#3285,.T.);
#2255=FACE_OUTER_BOUND('',#3286,.T.);
#2256=FACE_OUTER_BOUND('',#3287,.T.);
#2257=FACE_OUTER_BOUND('',#3288,.T.);
#2258=FACE_OUTER_BOUND('',#3289,.T.);
#2259=FACE_OUTER_BOUND('',#3290,.T.);
#2260=FACE_OUTER_BOUND('',#3291,.T.);
#2261=FACE_OUTER_BOUND('',#3292,.T.);
#2262=FACE_OUTER_BOUND('',#3293,.T.);
#2263=FACE_OUTER_BOUND('',#3294,.T.);
#2264=FACE_OUTER_BOUND('',#3295,.T.);
#2265=FACE_OUTER_BOUND('',#3296,.T.);
#2266=FACE_OUTER_BOUND('',#3297,.T.);
#2267=FACE_OUTER_BOUND('',#3298,.T.);
#2268=FACE_OUTER_BOUND('',#3299,.T.);
#2269=EDGE_LOOP('',(#11815,#11816,#11817,#11818));
#2270=EDGE_LOOP('',(#11819,#11820,#11821,#11822));
#2271=EDGE_LOOP('',(#11823,#11824,#11825,#11826));
#2272=EDGE_LOOP('',(#11827,#11828,#11829,#11830));
#2273=EDGE_LOOP('',(#11831,#11832,#11833,#11834));
#2274=EDGE_LOOP('',(#11835,#11836,#11837,#11838));
#2275=EDGE_LOOP('',(#11839,#11840,#11841,#11842));
#2276=EDGE_LOOP('',(#11843,#11844,#11845,#11846));
#2277=EDGE_LOOP('',(#11847,#11848,#11849,#11850));
#2278=EDGE_LOOP('',(#11851,#11852,#11853,#11854));
#2279=EDGE_LOOP('',(#11855,#11856,#11857,#11858));
#2280=EDGE_LOOP('',(#11859,#11860,#11861,#11862));
#2281=EDGE_LOOP('',(#11863,#11864,#11865,#11866));
#2282=EDGE_LOOP('',(#11867,#11868,#11869,#11870));
#2283=EDGE_LOOP('',(#11871,#11872,#11873,#11874));
#2284=EDGE_LOOP('',(#11875,#11876,#11877,#11878));
#2285=EDGE_LOOP('',(#11879,#11880,#11881,#11882,#11883,#11884,#11885,#11886,
#11887,#11888,#11889,#11890,#11891,#11892,#11893,#11894,#11895,#11896,#11897,
#11898,#11899,#11900,#11901,#11902,#11903,#11904,#11905,#11906,#11907,#11908,
#11909,#11910,#11911,#11912,#11913,#11914,#11915,#11916,#11917,#11918,#11919,
#11920,#11921,#11922,#11923,#11924,#11925,#11926,#11927,#11928,#11929,#11930,
#11931,#11932,#11933,#11934,#11935,#11936,#11937,#11938,#11939,#11940,#11941,
#11942,#11943,#11944,#11945,#11946,#11947,#11948,#11949,#11950,#11951,#11952,
#11953,#11954,#11955,#11956,#11957,#11958,#11959,#11960,#11961,#11962,#11963,
#11964,#11965,#11966,#11967,#11968,#11969,#11970,#11971,#11972,#11973,#11974));
#2286=EDGE_LOOP('',(#11975,#11976,#11977,#11978));
#2287=EDGE_LOOP('',(#11979,#11980,#11981,#11982));
#2288=EDGE_LOOP('',(#11983,#11984,#11985,#11986));
#2289=EDGE_LOOP('',(#11987,#11988,#11989,#11990));
#2290=EDGE_LOOP('',(#11991,#11992,#11993,#11994));
#2291=EDGE_LOOP('',(#11995,#11996,#11997,#11998));
#2292=EDGE_LOOP('',(#11999,#12000,#12001,#12002));
#2293=EDGE_LOOP('',(#12003,#12004,#12005,#12006));
#2294=EDGE_LOOP('',(#12007,#12008,#12009,#12010));
#2295=EDGE_LOOP('',(#12011,#12012,#12013,#12014));
#2296=EDGE_LOOP('',(#12015,#12016,#12017,#12018));
#2297=EDGE_LOOP('',(#12019,#12020,#12021,#12022));
#2298=EDGE_LOOP('',(#12023,#12024,#12025,#12026));
#2299=EDGE_LOOP('',(#12027,#12028,#12029,#12030));
#2300=EDGE_LOOP('',(#12031,#12032,#12033,#12034));
#2301=EDGE_LOOP('',(#12035,#12036,#12037,#12038));
#2302=EDGE_LOOP('',(#12039,#12040,#12041,#12042,#12043));
#2303=EDGE_LOOP('',(#12044,#12045,#12046,#12047,#12048));
#2304=EDGE_LOOP('',(#12049));
#2305=EDGE_LOOP('',(#12050));
#2306=EDGE_LOOP('',(#12051,#12052,#12053,#12054,#12055));
#2307=EDGE_LOOP('',(#12056,#12057,#12058,#12059));
#2308=EDGE_LOOP('',(#12060,#12061,#12062,#12063,#12064));
#2309=EDGE_LOOP('',(#12065,#12066,#12067,#12068,#12069));
#2310=EDGE_LOOP('',(#12070,#12071,#12072,#12073,#12074));
#2311=EDGE_LOOP('',(#12075,#12076,#12077,#12078));
#2312=EDGE_LOOP('',(#12079,#12080,#12081,#12082,#12083));
#2313=EDGE_LOOP('',(#12084,#12085,#12086,#12087,#12088));
#2314=EDGE_LOOP('',(#12089,#12090,#12091,#12092,#12093));
#2315=EDGE_LOOP('',(#12094,#12095,#12096,#12097));
#2316=EDGE_LOOP('',(#12098,#12099,#12100,#12101,#12102));
#2317=EDGE_LOOP('',(#12103,#12104,#12105,#12106,#12107));
#2318=EDGE_LOOP('',(#12108,#12109,#12110,#12111,#12112));
#2319=EDGE_LOOP('',(#12113,#12114,#12115,#12116));
#2320=EDGE_LOOP('',(#12117,#12118,#12119,#12120,#12121));
#2321=EDGE_LOOP('',(#12122,#12123,#12124,#12125,#12126));
#2322=EDGE_LOOP('',(#12127,#12128,#12129,#12130,#12131));
#2323=EDGE_LOOP('',(#12132,#12133,#12134,#12135));
#2324=EDGE_LOOP('',(#12136,#12137,#12138,#12139,#12140));
#2325=EDGE_LOOP('',(#12141,#12142,#12143,#12144,#12145));
#2326=EDGE_LOOP('',(#12146,#12147,#12148,#12149,#12150));
#2327=EDGE_LOOP('',(#12151,#12152,#12153,#12154));
#2328=EDGE_LOOP('',(#12155,#12156,#12157,#12158,#12159));
#2329=EDGE_LOOP('',(#12160,#12161,#12162,#12163,#12164));
#2330=EDGE_LOOP('',(#12165,#12166,#12167,#12168,#12169));
#2331=EDGE_LOOP('',(#12170,#12171,#12172,#12173));
#2332=EDGE_LOOP('',(#12174,#12175,#12176,#12177,#12178));
#2333=EDGE_LOOP('',(#12179,#12180,#12181,#12182,#12183));
#2334=EDGE_LOOP('',(#12184,#12185,#12186,#12187));
#2335=EDGE_LOOP('',(#12188,#12189,#12190,#12191,#12192));
#2336=EDGE_LOOP('',(#12193,#12194,#12195,#12196,#12197));
#2337=EDGE_LOOP('',(#12198,#12199,#12200,#12201,#12202));
#2338=EDGE_LOOP('',(#12203,#12204,#12205,#12206));
#2339=EDGE_LOOP('',(#12207,#12208,#12209,#12210,#12211));
#2340=EDGE_LOOP('',(#12212,#12213,#12214,#12215,#12216));
#2341=EDGE_LOOP('',(#12217,#12218,#12219,#12220,#12221));
#2342=EDGE_LOOP('',(#12222,#12223,#12224,#12225));
#2343=EDGE_LOOP('',(#12226,#12227,#12228,#12229,#12230));
#2344=EDGE_LOOP('',(#12231,#12232,#12233,#12234,#12235));
#2345=EDGE_LOOP('',(#12236,#12237,#12238,#12239,#12240));
#2346=EDGE_LOOP('',(#12241,#12242,#12243,#12244));
#2347=EDGE_LOOP('',(#12245,#12246,#12247,#12248,#12249));
#2348=EDGE_LOOP('',(#12250,#12251,#12252,#12253,#12254));
#2349=EDGE_LOOP('',(#12255,#12256,#12257,#12258,#12259));
#2350=EDGE_LOOP('',(#12260,#12261,#12262,#12263));
#2351=EDGE_LOOP('',(#12264,#12265,#12266,#12267,#12268));
#2352=EDGE_LOOP('',(#12269,#12270,#12271,#12272,#12273));
#2353=EDGE_LOOP('',(#12274,#12275,#12276,#12277));
#2354=EDGE_LOOP('',(#12278,#12279,#12280,#12281));
#2355=EDGE_LOOP('',(#12282,#12283,#12284,#12285,#12286,#12287,#12288,#12289,
#12290,#12291));
#2356=EDGE_LOOP('',(#12292,#12293,#12294,#12295));
#2357=EDGE_LOOP('',(#12296,#12297,#12298,#12299));
#2358=EDGE_LOOP('',(#12300,#12301,#12302,#12303,#12304,#12305,#12306,#12307,
#12308));
#2359=EDGE_LOOP('',(#12309,#12310,#12311,#12312));
#2360=EDGE_LOOP('',(#12313,#12314,#12315,#12316));
#2361=EDGE_LOOP('',(#12317,#12318,#12319,#12320,#12321,#12322,#12323,#12324,
#12325));
#2362=EDGE_LOOP('',(#12326,#12327,#12328,#12329));
#2363=EDGE_LOOP('',(#12330,#12331,#12332,#12333));
#2364=EDGE_LOOP('',(#12334,#12335,#12336,#12337,#12338,#12339,#12340,#12341,
#12342));
#2365=EDGE_LOOP('',(#12343,#12344,#12345,#12346));
#2366=EDGE_LOOP('',(#12347,#12348,#12349,#12350));
#2367=EDGE_LOOP('',(#12351,#12352,#12353,#12354,#12355,#12356,#12357,#12358,
#12359));
#2368=EDGE_LOOP('',(#12360,#12361,#12362,#12363));
#2369=EDGE_LOOP('',(#12364,#12365,#12366,#12367));
#2370=EDGE_LOOP('',(#12368,#12369,#12370,#12371,#12372,#12373,#12374,#12375,
#12376));
#2371=EDGE_LOOP('',(#12377,#12378,#12379,#12380));
#2372=EDGE_LOOP('',(#12381,#12382,#12383,#12384));
#2373=EDGE_LOOP('',(#12385,#12386,#12387,#12388,#12389,#12390,#12391,#12392,
#12393));
#2374=EDGE_LOOP('',(#12394,#12395,#12396,#12397));
#2375=EDGE_LOOP('',(#12398,#12399,#12400,#12401));
#2376=EDGE_LOOP('',(#12402,#12403,#12404,#12405,#12406,#12407,#12408,#12409,
#12410));
#2377=EDGE_LOOP('',(#12411,#12412,#12413,#12414));
#2378=EDGE_LOOP('',(#12415,#12416,#12417,#12418));
#2379=EDGE_LOOP('',(#12419,#12420,#12421,#12422,#12423,#12424,#12425,#12426,
#12427));
#2380=EDGE_LOOP('',(#12428,#12429,#12430,#12431));
#2381=EDGE_LOOP('',(#12432,#12433,#12434,#12435));
#2382=EDGE_LOOP('',(#12436,#12437,#12438,#12439,#12440,#12441,#12442,#12443,
#12444));
#2383=EDGE_LOOP('',(#12445,#12446,#12447,#12448));
#2384=EDGE_LOOP('',(#12449,#12450,#12451,#12452));
#2385=EDGE_LOOP('',(#12453,#12454,#12455,#12456,#12457,#12458,#12459,#12460,
#12461));
#2386=EDGE_LOOP('',(#12462,#12463,#12464,#12465));
#2387=EDGE_LOOP('',(#12466,#12467,#12468,#12469));
#2388=EDGE_LOOP('',(#12470,#12471,#12472,#12473,#12474,#12475,#12476,#12477,
#12478,#12479));
#2389=EDGE_LOOP('',(#12480,#12481,#12482,#12483));
#2390=EDGE_LOOP('',(#12484));
#2391=EDGE_LOOP('',(#12485));
#2392=EDGE_LOOP('',(#12486,#12487,#12488,#12489));
#2393=EDGE_LOOP('',(#12490,#12491,#12492,#12493));
#2394=EDGE_LOOP('',(#12494));
#2395=EDGE_LOOP('',(#12495));
#2396=EDGE_LOOP('',(#12496,#12497,#12498,#12499));
#2397=EDGE_LOOP('',(#12500,#12501,#12502,#12503,#12504));
#2398=EDGE_LOOP('',(#12505,#12506,#12507,#12508,#12509,#12510));
#2399=EDGE_LOOP('',(#12511,#12512,#12513,#12514,#12515,#12516));
#2400=EDGE_LOOP('',(#12517,#12518,#12519,#12520,#12521,#12522,#12523,#12524));
#2401=EDGE_LOOP('',(#12525,#12526,#12527,#12528,#12529));
#2402=EDGE_LOOP('',(#12530,#12531,#12532,#12533,#12534,#12535));
#2403=EDGE_LOOP('',(#12536,#12537,#12538,#12539,#12540));
#2404=EDGE_LOOP('',(#12541,#12542,#12543,#12544,#12545,#12546));
#2405=EDGE_LOOP('',(#12547,#12548,#12549,#12550,#12551,#12552,#12553,#12554));
#2406=EDGE_LOOP('',(#12555,#12556,#12557,#12558,#12559));
#2407=EDGE_LOOP('',(#12560,#12561,#12562,#12563,#12564,#12565));
#2408=EDGE_LOOP('',(#12566,#12567,#12568,#12569,#12570));
#2409=EDGE_LOOP('',(#12571,#12572,#12573,#12574,#12575,#12576));
#2410=EDGE_LOOP('',(#12577,#12578,#12579,#12580,#12581,#12582,#12583,#12584));
#2411=EDGE_LOOP('',(#12585,#12586,#12587,#12588,#12589));
#2412=EDGE_LOOP('',(#12590,#12591,#12592,#12593,#12594,#12595));
#2413=EDGE_LOOP('',(#12596,#12597,#12598,#12599,#12600));
#2414=EDGE_LOOP('',(#12601,#12602,#12603,#12604,#12605,#12606));
#2415=EDGE_LOOP('',(#12607,#12608,#12609,#12610,#12611,#12612,#12613,#12614));
#2416=EDGE_LOOP('',(#12615,#12616,#12617,#12618,#12619));
#2417=EDGE_LOOP('',(#12620,#12621,#12622,#12623,#12624,#12625));
#2418=EDGE_LOOP('',(#12626,#12627,#12628,#12629,#12630));
#2419=EDGE_LOOP('',(#12631,#12632,#12633,#12634,#12635,#12636));
#2420=EDGE_LOOP('',(#12637,#12638,#12639,#12640,#12641,#12642,#12643,#12644));
#2421=EDGE_LOOP('',(#12645,#12646,#12647,#12648,#12649));
#2422=EDGE_LOOP('',(#12650,#12651,#12652,#12653,#12654,#12655));
#2423=EDGE_LOOP('',(#12656,#12657,#12658,#12659,#12660,#12661,#12662,#12663,
#12664,#12665,#12666,#12667,#12668,#12669,#12670,#12671,#12672,#12673,#12674,
#12675,#12676,#12677,#12678,#12679));
#2424=EDGE_LOOP('',(#12680));
#2425=EDGE_LOOP('',(#12681,#12682,#12683,#12684,#12685,#12686));
#2426=EDGE_LOOP('',(#12687,#12688,#12689,#12690,#12691));
#2427=EDGE_LOOP('',(#12692,#12693,#12694,#12695,#12696,#12697,#12698,#12699));
#2428=EDGE_LOOP('',(#12700,#12701,#12702,#12703,#12704,#12705,#12706,#12707));
#2429=EDGE_LOOP('',(#12708,#12709,#12710,#12711,#12712));
#2430=EDGE_LOOP('',(#12713,#12714,#12715,#12716,#12717,#12718,#12719,#12720));
#2431=EDGE_LOOP('',(#12721,#12722,#12723,#12724,#12725));
#2432=EDGE_LOOP('',(#12726,#12727,#12728,#12729,#12730,#12731));
#2433=EDGE_LOOP('',(#12732,#12733,#12734,#12735,#12736,#12737));
#2434=EDGE_LOOP('',(#12738,#12739,#12740,#12741,#12742));
#2435=EDGE_LOOP('',(#12743,#12744,#12745,#12746,#12747,#12748,#12749,#12750));
#2436=EDGE_LOOP('',(#12751,#12752,#12753,#12754,#12755));
#2437=EDGE_LOOP('',(#12756,#12757,#12758,#12759,#12760,#12761));
#2438=EDGE_LOOP('',(#12762,#12763,#12764,#12765,#12766,#12767));
#2439=EDGE_LOOP('',(#12768,#12769,#12770,#12771,#12772));
#2440=EDGE_LOOP('',(#12773,#12774,#12775,#12776,#12777,#12778,#12779,#12780));
#2441=EDGE_LOOP('',(#12781,#12782,#12783,#12784,#12785));
#2442=EDGE_LOOP('',(#12786,#12787,#12788,#12789,#12790,#12791));
#2443=EDGE_LOOP('',(#12792,#12793,#12794,#12795,#12796,#12797));
#2444=EDGE_LOOP('',(#12798,#12799,#12800,#12801,#12802));
#2445=EDGE_LOOP('',(#12803,#12804,#12805,#12806,#12807,#12808,#12809,#12810));
#2446=EDGE_LOOP('',(#12811,#12812,#12813,#12814,#12815));
#2447=EDGE_LOOP('',(#12816,#12817,#12818,#12819,#12820,#12821));
#2448=EDGE_LOOP('',(#12822,#12823,#12824,#12825,#12826,#12827));
#2449=EDGE_LOOP('',(#12828,#12829,#12830,#12831,#12832));
#2450=EDGE_LOOP('',(#12833,#12834,#12835,#12836,#12837,#12838,#12839,#12840));
#2451=EDGE_LOOP('',(#12841,#12842,#12843,#12844,#12845));
#2452=EDGE_LOOP('',(#12846,#12847,#12848,#12849,#12850,#12851));
#2453=EDGE_LOOP('',(#12852,#12853,#12854,#12855,#12856,#12857));
#2454=EDGE_LOOP('',(#12858,#12859,#12860,#12861,#12862));
#2455=EDGE_LOOP('',(#12863,#12864,#12865,#12866,#12867,#12868,#12869,#12870));
#2456=EDGE_LOOP('',(#12871,#12872,#12873,#12874,#12875,#12876));
#2457=EDGE_LOOP('',(#12877,#12878,#12879,#12880,#12881,#12882,#12883,#12884));
#2458=EDGE_LOOP('',(#12885,#12886,#12887,#12888,#12889));
#2459=EDGE_LOOP('',(#12890,#12891,#12892,#12893,#12894,#12895));
#2460=EDGE_LOOP('',(#12896,#12897,#12898,#12899,#12900));
#2461=EDGE_LOOP('',(#12901,#12902,#12903,#12904,#12905));
#2462=EDGE_LOOP('',(#12906,#12907,#12908,#12909,#12910,#12911,#12912,#12913));
#2463=EDGE_LOOP('',(#12914,#12915,#12916,#12917,#12918));
#2464=EDGE_LOOP('',(#12919,#12920,#12921,#12922,#12923,#12924,#12925,#12926,
#12927,#12928,#12929,#12930,#12931,#12932,#12933,#12934,#12935,#12936,#12937,
#12938,#12939,#12940,#12941,#12942,#12943,#12944,#12945,#12946,#12947,#12948,
#12949,#12950,#12951,#12952,#12953,#12954));
#2465=EDGE_LOOP('',(#12955,#12956,#12957,#12958,#12959));
#2466=EDGE_LOOP('',(#12960,#12961,#12962,#12963));
#2467=EDGE_LOOP('',(#12964,#12965,#12966,#12967,#12968,#12969,#12970,#12971,
#12972,#12973,#12974,#12975,#12976,#12977,#12978,#12979,#12980,#12981,#12982,
#12983,#12984,#12985,#12986,#12987,#12988,#12989,#12990,#12991,#12992,#12993,
#12994,#12995,#12996,#12997,#12998,#12999));
#2468=EDGE_LOOP('',(#13000,#13001));
#2469=EDGE_LOOP('',(#13002,#13003,#13004,#13005,#13006,#13007,#13008,#13009));
#2470=EDGE_LOOP('',(#13010,#13011,#13012,#13013,#13014));
#2471=EDGE_LOOP('',(#13015,#13016));
#2472=EDGE_LOOP('',(#13017,#13018,#13019,#13020,#13021,#13022,#13023,#13024));
#2473=EDGE_LOOP('',(#13025,#13026,#13027,#13028,#13029));
#2474=EDGE_LOOP('',(#13030,#13031,#13032,#13033,#13034));
#2475=EDGE_LOOP('',(#13035,#13036));
#2476=EDGE_LOOP('',(#13037,#13038,#13039,#13040,#13041,#13042,#13043,#13044));
#2477=EDGE_LOOP('',(#13045,#13046,#13047,#13048,#13049));
#2478=EDGE_LOOP('',(#13050,#13051,#13052,#13053,#13054));
#2479=EDGE_LOOP('',(#13055,#13056));
#2480=EDGE_LOOP('',(#13057,#13058,#13059,#13060,#13061,#13062,#13063,#13064));
#2481=EDGE_LOOP('',(#13065,#13066,#13067,#13068,#13069));
#2482=EDGE_LOOP('',(#13070,#13071,#13072,#13073,#13074));
#2483=EDGE_LOOP('',(#13075,#13076));
#2484=EDGE_LOOP('',(#13077,#13078,#13079,#13080,#13081,#13082,#13083,#13084));
#2485=EDGE_LOOP('',(#13085,#13086,#13087,#13088,#13089));
#2486=EDGE_LOOP('',(#13090,#13091,#13092,#13093,#13094));
#2487=EDGE_LOOP('',(#13095,#13096));
#2488=EDGE_LOOP('',(#13097,#13098,#13099,#13100,#13101,#13102,#13103,#13104));
#2489=EDGE_LOOP('',(#13105,#13106,#13107,#13108,#13109));
#2490=EDGE_LOOP('',(#13110,#13111,#13112,#13113,#13114));
#2491=EDGE_LOOP('',(#13115,#13116));
#2492=EDGE_LOOP('',(#13117,#13118,#13119,#13120,#13121,#13122,#13123,#13124));
#2493=EDGE_LOOP('',(#13125,#13126,#13127,#13128,#13129));
#2494=EDGE_LOOP('',(#13130,#13131,#13132,#13133,#13134));
#2495=EDGE_LOOP('',(#13135,#13136));
#2496=EDGE_LOOP('',(#13137,#13138,#13139,#13140,#13141,#13142,#13143,#13144));
#2497=EDGE_LOOP('',(#13145,#13146,#13147,#13148,#13149));
#2498=EDGE_LOOP('',(#13150,#13151,#13152,#13153,#13154));
#2499=EDGE_LOOP('',(#13155,#13156));
#2500=EDGE_LOOP('',(#13157,#13158,#13159,#13160,#13161,#13162,#13163,#13164));
#2501=EDGE_LOOP('',(#13165,#13166,#13167,#13168,#13169));
#2502=EDGE_LOOP('',(#13170,#13171,#13172,#13173,#13174));
#2503=EDGE_LOOP('',(#13175,#13176));
#2504=EDGE_LOOP('',(#13177,#13178,#13179,#13180,#13181,#13182,#13183,#13184));
#2505=EDGE_LOOP('',(#13185,#13186,#13187,#13188,#13189));
#2506=EDGE_LOOP('',(#13190,#13191,#13192,#13193,#13194));
#2507=EDGE_LOOP('',(#13195,#13196));
#2508=EDGE_LOOP('',(#13197,#13198,#13199,#13200,#13201));
#2509=EDGE_LOOP('',(#13202,#13203,#13204,#13205,#13206));
#2510=EDGE_LOOP('',(#13207,#13208));
#2511=EDGE_LOOP('',(#13209,#13210,#13211,#13212,#13213));
#2512=EDGE_LOOP('',(#13214,#13215,#13216,#13217,#13218));
#2513=EDGE_LOOP('',(#13219,#13220,#13221,#13222));
#2514=EDGE_LOOP('',(#13223));
#2515=EDGE_LOOP('',(#13224));
#2516=EDGE_LOOP('',(#13225));
#2517=EDGE_LOOP('',(#13226));
#2518=EDGE_LOOP('',(#13227,#13228,#13229,#13230));
#2519=EDGE_LOOP('',(#13231,#13232,#13233,#13234));
#2520=EDGE_LOOP('',(#13235,#13236,#13237,#13238));
#2521=EDGE_LOOP('',(#13239,#13240,#13241,#13242));
#2522=EDGE_LOOP('',(#13243,#13244,#13245,#13246,#13247));
#2523=EDGE_LOOP('',(#13248,#13249,#13250,#13251,#13252,#13253,#13254,#13255,
#13256));
#2524=EDGE_LOOP('',(#13257,#13258,#13259,#13260));
#2525=EDGE_LOOP('',(#13261,#13262,#13263,#13264));
#2526=EDGE_LOOP('',(#13265,#13266,#13267,#13268,#13269));
#2527=EDGE_LOOP('',(#13270,#13271,#13272,#13273,#13274,#13275,#13276,#13277));
#2528=EDGE_LOOP('',(#13278,#13279,#13280,#13281));
#2529=EDGE_LOOP('',(#13282,#13283,#13284,#13285));
#2530=EDGE_LOOP('',(#13286,#13287,#13288,#13289,#13290));
#2531=EDGE_LOOP('',(#13291,#13292,#13293,#13294,#13295,#13296,#13297,#13298));
#2532=EDGE_LOOP('',(#13299,#13300,#13301,#13302));
#2533=EDGE_LOOP('',(#13303,#13304,#13305,#13306));
#2534=EDGE_LOOP('',(#13307,#13308,#13309,#13310,#13311));
#2535=EDGE_LOOP('',(#13312,#13313,#13314,#13315,#13316,#13317,#13318,#13319));
#2536=EDGE_LOOP('',(#13320,#13321,#13322,#13323));
#2537=EDGE_LOOP('',(#13324,#13325,#13326,#13327));
#2538=EDGE_LOOP('',(#13328,#13329,#13330,#13331,#13332));
#2539=EDGE_LOOP('',(#13333,#13334,#13335,#13336,#13337,#13338,#13339,#13340));
#2540=EDGE_LOOP('',(#13341,#13342,#13343,#13344));
#2541=EDGE_LOOP('',(#13345,#13346,#13347,#13348));
#2542=EDGE_LOOP('',(#13349,#13350,#13351,#13352,#13353));
#2543=EDGE_LOOP('',(#13354,#13355,#13356,#13357,#13358,#13359,#13360,#13361));
#2544=EDGE_LOOP('',(#13362,#13363,#13364,#13365));
#2545=EDGE_LOOP('',(#13366,#13367,#13368,#13369));
#2546=EDGE_LOOP('',(#13370,#13371,#13372,#13373,#13374));
#2547=EDGE_LOOP('',(#13375,#13376,#13377,#13378,#13379,#13380,#13381,#13382));
#2548=EDGE_LOOP('',(#13383,#13384,#13385,#13386));
#2549=EDGE_LOOP('',(#13387,#13388,#13389,#13390));
#2550=EDGE_LOOP('',(#13391,#13392,#13393,#13394,#13395));
#2551=EDGE_LOOP('',(#13396,#13397,#13398,#13399,#13400,#13401,#13402,#13403));
#2552=EDGE_LOOP('',(#13404,#13405,#13406,#13407));
#2553=EDGE_LOOP('',(#13408,#13409,#13410,#13411));
#2554=EDGE_LOOP('',(#13412,#13413,#13414,#13415,#13416));
#2555=EDGE_LOOP('',(#13417,#13418,#13419,#13420,#13421,#13422,#13423,#13424));
#2556=EDGE_LOOP('',(#13425,#13426,#13427,#13428));
#2557=EDGE_LOOP('',(#13429,#13430,#13431,#13432));
#2558=EDGE_LOOP('',(#13433,#13434,#13435,#13436,#13437));
#2559=EDGE_LOOP('',(#13438,#13439,#13440,#13441,#13442,#13443,#13444,#13445));
#2560=EDGE_LOOP('',(#13446,#13447,#13448,#13449));
#2561=EDGE_LOOP('',(#13450,#13451,#13452,#13453));
#2562=EDGE_LOOP('',(#13454,#13455,#13456,#13457,#13458));
#2563=EDGE_LOOP('',(#13459,#13460,#13461,#13462,#13463,#13464,#13465,#13466));
#2564=EDGE_LOOP('',(#13467,#13468,#13469,#13470));
#2565=EDGE_LOOP('',(#13471,#13472,#13473,#13474));
#2566=EDGE_LOOP('',(#13475,#13476,#13477,#13478,#13479));
#2567=EDGE_LOOP('',(#13480,#13481,#13482,#13483,#13484,#13485,#13486,#13487));
#2568=EDGE_LOOP('',(#13488,#13489,#13490,#13491,#13492));
#2569=EDGE_LOOP('',(#13493,#13494,#13495,#13496));
#2570=EDGE_LOOP('',(#13497,#13498,#13499,#13500));
#2571=EDGE_LOOP('',(#13501,#13502,#13503,#13504));
#2572=EDGE_LOOP('',(#13505,#13506,#13507,#13508));
#2573=EDGE_LOOP('',(#13509,#13510,#13511,#13512));
#2574=EDGE_LOOP('',(#13513,#13514,#13515,#13516));
#2575=EDGE_LOOP('',(#13517,#13518,#13519,#13520,#13521,#13522,#13523,#13524,
#13525,#13526,#13527,#13528,#13529,#13530,#13531,#13532,#13533,#13534,#13535,
#13536,#13537,#13538,#13539,#13540));
#2576=EDGE_LOOP('',(#13541,#13542,#13543,#13544));
#2577=EDGE_LOOP('',(#13545,#13546,#13547,#13548));
#2578=EDGE_LOOP('',(#13549,#13550,#13551,#13552));
#2579=EDGE_LOOP('',(#13553,#13554,#13555,#13556));
#2580=EDGE_LOOP('',(#13557,#13558,#13559,#13560));
#2581=EDGE_LOOP('',(#13561,#13562,#13563,#13564));
#2582=EDGE_LOOP('',(#13565));
#2583=EDGE_LOOP('',(#13566,#13567,#13568,#13569,#13570,#13571,#13572,#13573,
#13574,#13575,#13576,#13577,#13578,#13579,#13580,#13581,#13582,#13583,#13584,
#13585,#13586,#13587,#13588,#13589,#13590,#13591,#13592,#13593,#13594,#13595,
#13596,#13597,#13598,#13599,#13600,#13601));
#2584=EDGE_LOOP('',(#13602,#13603,#13604,#13605));
#2585=EDGE_LOOP('',(#13606,#13607,#13608,#13609));
#2586=EDGE_LOOP('',(#13610,#13611,#13612,#13613));
#2587=EDGE_LOOP('',(#13614,#13615,#13616,#13617));
#2588=EDGE_LOOP('',(#13618));
#2589=EDGE_LOOP('',(#13619));
#2590=EDGE_LOOP('',(#13620,#13621,#13622,#13623));
#2591=EDGE_LOOP('',(#13624,#13625,#13626,#13627));
#2592=EDGE_LOOP('',(#13628,#13629,#13630,#13631));
#2593=EDGE_LOOP('',(#13632,#13633,#13634,#13635));
#2594=EDGE_LOOP('',(#13636));
#2595=EDGE_LOOP('',(#13637));
#2596=EDGE_LOOP('',(#13638,#13639,#13640,#13641));
#2597=EDGE_LOOP('',(#13642,#13643,#13644,#13645));
#2598=EDGE_LOOP('',(#13646,#13647,#13648,#13649));
#2599=EDGE_LOOP('',(#13650,#13651,#13652,#13653));
#2600=EDGE_LOOP('',(#13654,#13655,#13656,#13657));
#2601=EDGE_LOOP('',(#13658,#13659,#13660,#13661,#13662,#13663));
#2602=EDGE_LOOP('',(#13664,#13665,#13666,#13667));
#2603=EDGE_LOOP('',(#13668,#13669,#13670,#13671,#13672,#13673));
#2604=EDGE_LOOP('',(#13674));
#2605=EDGE_LOOP('',(#13675,#13676,#13677,#13678));
#2606=EDGE_LOOP('',(#13679,#13680,#13681,#13682,#13683,#13684,#13685,#13686));
#2607=EDGE_LOOP('',(#13687,#13688,#13689,#13690));
#2608=EDGE_LOOP('',(#13691,#13692,#13693,#13694));
#2609=EDGE_LOOP('',(#13695,#13696,#13697,#13698));
#2610=EDGE_LOOP('',(#13699,#13700,#13701,#13702));
#2611=EDGE_LOOP('',(#13703,#13704,#13705,#13706));
#2612=EDGE_LOOP('',(#13707,#13708,#13709,#13710,#13711,#13712,#13713,#13714));
#2613=EDGE_LOOP('',(#13715,#13716,#13717,#13718));
#2614=EDGE_LOOP('',(#13719,#13720,#13721,#13722));
#2615=EDGE_LOOP('',(#13723,#13724,#13725,#13726));
#2616=EDGE_LOOP('',(#13727,#13728,#13729,#13730));
#2617=EDGE_LOOP('',(#13731,#13732,#13733,#13734));
#2618=EDGE_LOOP('',(#13735));
#2619=EDGE_LOOP('',(#13736));
#2620=EDGE_LOOP('',(#13737,#13738,#13739,#13740));
#2621=EDGE_LOOP('',(#13741,#13742,#13743,#13744));
#2622=EDGE_LOOP('',(#13745,#13746,#13747,#13748));
#2623=EDGE_LOOP('',(#13749));
#2624=EDGE_LOOP('',(#13750));
#2625=EDGE_LOOP('',(#13751,#13752,#13753,#13754));
#2626=EDGE_LOOP('',(#13755,#13756,#13757,#13758));
#2627=EDGE_LOOP('',(#13759));
#2628=EDGE_LOOP('',(#13760,#13761,#13762,#13763));
#2629=EDGE_LOOP('',(#13764,#13765,#13766,#13767));
#2630=EDGE_LOOP('',(#13768));
#2631=EDGE_LOOP('',(#13769));
#2632=EDGE_LOOP('',(#13770));
#2633=EDGE_LOOP('',(#13771,#13772,#13773,#13774,#13775,#13776,#13777,#13778,
#13779,#13780,#13781,#13782,#13783,#13784));
#2634=EDGE_LOOP('',(#13785,#13786,#13787,#13788,#13789,#13790,#13791,#13792,
#13793,#13794,#13795,#13796,#13797,#13798));
#2635=EDGE_LOOP('',(#13799,#13800,#13801,#13802,#13803,#13804,#13805,#13806,
#13807,#13808,#13809,#13810,#13811,#13812));
#2636=EDGE_LOOP('',(#13813,#13814,#13815,#13816,#13817,#13818,#13819,#13820,
#13821,#13822,#13823,#13824,#13825,#13826));
#2637=EDGE_LOOP('',(#13827,#13828,#13829,#13830,#13831,#13832,#13833,#13834,
#13835,#13836,#13837,#13838,#13839,#13840));
#2638=EDGE_LOOP('',(#13841,#13842,#13843,#13844,#13845,#13846,#13847,#13848,
#13849,#13850,#13851,#13852,#13853,#13854));
#2639=EDGE_LOOP('',(#13855));
#2640=EDGE_LOOP('',(#13856,#13857,#13858,#13859,#13860,#13861));
#2641=EDGE_LOOP('',(#13862,#13863,#13864,#13865));
#2642=EDGE_LOOP('',(#13866,#13867,#13868,#13869,#13870,#13871));
#2643=EDGE_LOOP('',(#13872,#13873,#13874,#13875));
#2644=EDGE_LOOP('',(#13876,#13877,#13878,#13879,#13880,#13881,#13882,#13883));
#2645=EDGE_LOOP('',(#13884,#13885,#13886,#13887));
#2646=EDGE_LOOP('',(#13888));
#2647=EDGE_LOOP('',(#13889));
#2648=EDGE_LOOP('',(#13890));
#2649=EDGE_LOOP('',(#13891,#13892,#13893,#13894,#13895,#13896,#13897,#13898,
#13899,#13900,#13901,#13902,#13903,#13904));
#2650=EDGE_LOOP('',(#13905,#13906,#13907,#13908,#13909,#13910,#13911,#13912,
#13913,#13914,#13915,#13916,#13917,#13918));
#2651=EDGE_LOOP('',(#13919,#13920,#13921,#13922,#13923,#13924,#13925,#13926,
#13927,#13928,#13929,#13930,#13931,#13932));
#2652=EDGE_LOOP('',(#13933,#13934,#13935,#13936,#13937,#13938,#13939,#13940,
#13941,#13942,#13943,#13944,#13945,#13946));
#2653=EDGE_LOOP('',(#13947,#13948,#13949,#13950,#13951,#13952,#13953,#13954,
#13955,#13956,#13957,#13958,#13959,#13960));
#2654=EDGE_LOOP('',(#13961,#13962,#13963,#13964,#13965,#13966,#13967,#13968,
#13969,#13970,#13971,#13972,#13973,#13974));
#2655=EDGE_LOOP('',(#13975));
#2656=EDGE_LOOP('',(#13976,#13977,#13978,#13979));
#2657=EDGE_LOOP('',(#13980,#13981,#13982,#13983));
#2658=EDGE_LOOP('',(#13984,#13985,#13986,#13987));
#2659=EDGE_LOOP('',(#13988,#13989,#13990,#13991));
#2660=EDGE_LOOP('',(#13992,#13993,#13994,#13995));
#2661=EDGE_LOOP('',(#13996,#13997,#13998,#13999));
#2662=EDGE_LOOP('',(#14000,#14001,#14002,#14003));
#2663=EDGE_LOOP('',(#14004,#14005,#14006,#14007));
#2664=EDGE_LOOP('',(#14008,#14009,#14010,#14011));
#2665=EDGE_LOOP('',(#14012,#14013,#14014,#14015));
#2666=EDGE_LOOP('',(#14016,#14017,#14018,#14019));
#2667=EDGE_LOOP('',(#14020,#14021,#14022,#14023,#14024,#14025));
#2668=EDGE_LOOP('',(#14026,#14027,#14028,#14029));
#2669=EDGE_LOOP('',(#14030,#14031,#14032,#14033));
#2670=EDGE_LOOP('',(#14034,#14035,#14036,#14037));
#2671=EDGE_LOOP('',(#14038,#14039,#14040,#14041));
#2672=EDGE_LOOP('',(#14042,#14043,#14044,#14045));
#2673=EDGE_LOOP('',(#14046,#14047,#14048,#14049));
#2674=EDGE_LOOP('',(#14050,#14051,#14052,#14053));
#2675=EDGE_LOOP('',(#14054,#14055,#14056,#14057));
#2676=EDGE_LOOP('',(#14058,#14059,#14060,#14061));
#2677=EDGE_LOOP('',(#14062,#14063,#14064,#14065));
#2678=EDGE_LOOP('',(#14066,#14067,#14068,#14069));
#2679=EDGE_LOOP('',(#14070,#14071,#14072,#14073));
#2680=EDGE_LOOP('',(#14074,#14075,#14076,#14077));
#2681=EDGE_LOOP('',(#14078,#14079,#14080,#14081));
#2682=EDGE_LOOP('',(#14082,#14083,#14084,#14085,#14086,#14087,#14088,#14089,
#14090,#14091,#14092,#14093,#14094,#14095));
#2683=EDGE_LOOP('',(#14096,#14097,#14098,#14099));
#2684=EDGE_LOOP('',(#14100,#14101,#14102,#14103));
#2685=EDGE_LOOP('',(#14104,#14105,#14106,#14107));
#2686=EDGE_LOOP('',(#14108,#14109,#14110,#14111));
#2687=EDGE_LOOP('',(#14112,#14113,#14114,#14115));
#2688=EDGE_LOOP('',(#14116,#14117,#14118,#14119));
#2689=EDGE_LOOP('',(#14120,#14121,#14122,#14123));
#2690=EDGE_LOOP('',(#14124,#14125,#14126,#14127));
#2691=EDGE_LOOP('',(#14128,#14129,#14130,#14131));
#2692=EDGE_LOOP('',(#14132,#14133,#14134,#14135));
#2693=EDGE_LOOP('',(#14136,#14137,#14138,#14139));
#2694=EDGE_LOOP('',(#14140,#14141,#14142,#14143));
#2695=EDGE_LOOP('',(#14144,#14145,#14146,#14147));
#2696=EDGE_LOOP('',(#14148,#14149,#14150,#14151));
#2697=EDGE_LOOP('',(#14152,#14153,#14154,#14155,#14156,#14157,#14158,#14159,
#14160,#14161,#14162,#14163,#14164,#14165));
#2698=EDGE_LOOP('',(#14166,#14167,#14168,#14169));
#2699=EDGE_LOOP('',(#14170,#14171,#14172,#14173));
#2700=EDGE_LOOP('',(#14174,#14175,#14176,#14177));
#2701=EDGE_LOOP('',(#14178,#14179,#14180,#14181));
#2702=EDGE_LOOP('',(#14182,#14183,#14184,#14185));
#2703=EDGE_LOOP('',(#14186,#14187,#14188,#14189));
#2704=EDGE_LOOP('',(#14190,#14191,#14192,#14193));
#2705=EDGE_LOOP('',(#14194,#14195,#14196,#14197));
#2706=EDGE_LOOP('',(#14198,#14199,#14200,#14201));
#2707=EDGE_LOOP('',(#14202,#14203,#14204,#14205));
#2708=EDGE_LOOP('',(#14206,#14207,#14208,#14209));
#2709=EDGE_LOOP('',(#14210,#14211,#14212,#14213));
#2710=EDGE_LOOP('',(#14214,#14215,#14216,#14217));
#2711=EDGE_LOOP('',(#14218,#14219,#14220,#14221));
#2712=EDGE_LOOP('',(#14222,#14223,#14224,#14225,#14226,#14227,#14228,#14229,
#14230,#14231,#14232,#14233,#14234,#14235));
#2713=EDGE_LOOP('',(#14236,#14237,#14238,#14239));
#2714=EDGE_LOOP('',(#14240,#14241,#14242,#14243));
#2715=EDGE_LOOP('',(#14244,#14245,#14246,#14247));
#2716=EDGE_LOOP('',(#14248,#14249,#14250,#14251));
#2717=EDGE_LOOP('',(#14252,#14253,#14254,#14255));
#2718=EDGE_LOOP('',(#14256,#14257,#14258,#14259));
#2719=EDGE_LOOP('',(#14260,#14261,#14262,#14263));
#2720=EDGE_LOOP('',(#14264,#14265,#14266,#14267));
#2721=EDGE_LOOP('',(#14268,#14269,#14270,#14271));
#2722=EDGE_LOOP('',(#14272,#14273,#14274,#14275));
#2723=EDGE_LOOP('',(#14276,#14277,#14278,#14279));
#2724=EDGE_LOOP('',(#14280,#14281,#14282,#14283));
#2725=EDGE_LOOP('',(#14284,#14285,#14286,#14287));
#2726=EDGE_LOOP('',(#14288,#14289,#14290,#14291));
#2727=EDGE_LOOP('',(#14292,#14293,#14294,#14295,#14296,#14297,#14298,#14299,
#14300,#14301,#14302,#14303,#14304,#14305));
#2728=EDGE_LOOP('',(#14306,#14307,#14308,#14309));
#2729=EDGE_LOOP('',(#14310,#14311,#14312,#14313));
#2730=EDGE_LOOP('',(#14314,#14315,#14316,#14317));
#2731=EDGE_LOOP('',(#14318,#14319,#14320,#14321));
#2732=EDGE_LOOP('',(#14322,#14323,#14324,#14325));
#2733=EDGE_LOOP('',(#14326,#14327,#14328,#14329));
#2734=EDGE_LOOP('',(#14330,#14331,#14332,#14333));
#2735=EDGE_LOOP('',(#14334,#14335,#14336,#14337));
#2736=EDGE_LOOP('',(#14338,#14339,#14340,#14341));
#2737=EDGE_LOOP('',(#14342,#14343,#14344,#14345));
#2738=EDGE_LOOP('',(#14346,#14347,#14348,#14349));
#2739=EDGE_LOOP('',(#14350,#14351,#14352,#14353));
#2740=EDGE_LOOP('',(#14354,#14355,#14356,#14357));
#2741=EDGE_LOOP('',(#14358,#14359,#14360,#14361));
#2742=EDGE_LOOP('',(#14362,#14363,#14364,#14365,#14366,#14367,#14368,#14369,
#14370,#14371,#14372,#14373,#14374,#14375));
#2743=EDGE_LOOP('',(#14376,#14377,#14378,#14379));
#2744=EDGE_LOOP('',(#14380,#14381,#14382,#14383));
#2745=EDGE_LOOP('',(#14384,#14385,#14386,#14387));
#2746=EDGE_LOOP('',(#14388,#14389,#14390,#14391));
#2747=EDGE_LOOP('',(#14392,#14393,#14394,#14395));
#2748=EDGE_LOOP('',(#14396,#14397,#14398,#14399));
#2749=EDGE_LOOP('',(#14400,#14401,#14402,#14403));
#2750=EDGE_LOOP('',(#14404,#14405,#14406,#14407));
#2751=EDGE_LOOP('',(#14408,#14409,#14410,#14411));
#2752=EDGE_LOOP('',(#14412,#14413,#14414,#14415));
#2753=EDGE_LOOP('',(#14416,#14417,#14418,#14419));
#2754=EDGE_LOOP('',(#14420,#14421,#14422,#14423));
#2755=EDGE_LOOP('',(#14424,#14425,#14426,#14427));
#2756=EDGE_LOOP('',(#14428,#14429,#14430,#14431));
#2757=EDGE_LOOP('',(#14432,#14433,#14434,#14435,#14436,#14437,#14438,#14439,
#14440,#14441,#14442,#14443,#14444,#14445));
#2758=EDGE_LOOP('',(#14446,#14447,#14448,#14449));
#2759=EDGE_LOOP('',(#14450,#14451,#14452,#14453));
#2760=EDGE_LOOP('',(#14454,#14455,#14456,#14457));
#2761=EDGE_LOOP('',(#14458,#14459,#14460,#14461));
#2762=EDGE_LOOP('',(#14462,#14463,#14464,#14465));
#2763=EDGE_LOOP('',(#14466,#14467,#14468,#14469));
#2764=EDGE_LOOP('',(#14470,#14471,#14472,#14473));
#2765=EDGE_LOOP('',(#14474,#14475,#14476,#14477));
#2766=EDGE_LOOP('',(#14478,#14479,#14480,#14481));
#2767=EDGE_LOOP('',(#14482,#14483,#14484,#14485));
#2768=EDGE_LOOP('',(#14486,#14487,#14488,#14489));
#2769=EDGE_LOOP('',(#14490,#14491,#14492,#14493));
#2770=EDGE_LOOP('',(#14494,#14495,#14496,#14497));
#2771=EDGE_LOOP('',(#14498,#14499,#14500,#14501));
#2772=EDGE_LOOP('',(#14502,#14503,#14504,#14505,#14506,#14507,#14508,#14509,
#14510,#14511,#14512,#14513,#14514,#14515));
#2773=EDGE_LOOP('',(#14516,#14517,#14518,#14519));
#2774=EDGE_LOOP('',(#14520,#14521,#14522,#14523));
#2775=EDGE_LOOP('',(#14524,#14525,#14526,#14527));
#2776=EDGE_LOOP('',(#14528,#14529,#14530,#14531));
#2777=EDGE_LOOP('',(#14532,#14533,#14534,#14535));
#2778=EDGE_LOOP('',(#14536,#14537,#14538,#14539));
#2779=EDGE_LOOP('',(#14540,#14541,#14542,#14543));
#2780=EDGE_LOOP('',(#14544,#14545,#14546,#14547));
#2781=EDGE_LOOP('',(#14548,#14549,#14550,#14551));
#2782=EDGE_LOOP('',(#14552,#14553,#14554,#14555));
#2783=EDGE_LOOP('',(#14556,#14557,#14558,#14559));
#2784=EDGE_LOOP('',(#14560,#14561,#14562,#14563));
#2785=EDGE_LOOP('',(#14564,#14565,#14566,#14567));
#2786=EDGE_LOOP('',(#14568,#14569,#14570,#14571));
#2787=EDGE_LOOP('',(#14572,#14573,#14574,#14575,#14576,#14577,#14578,#14579,
#14580,#14581,#14582,#14583,#14584,#14585));
#2788=EDGE_LOOP('',(#14586,#14587,#14588,#14589));
#2789=EDGE_LOOP('',(#14590,#14591,#14592,#14593));
#2790=EDGE_LOOP('',(#14594,#14595,#14596,#14597));
#2791=EDGE_LOOP('',(#14598,#14599,#14600,#14601));
#2792=EDGE_LOOP('',(#14602,#14603,#14604,#14605));
#2793=EDGE_LOOP('',(#14606,#14607,#14608,#14609));
#2794=EDGE_LOOP('',(#14610,#14611,#14612,#14613));
#2795=EDGE_LOOP('',(#14614,#14615,#14616,#14617));
#2796=EDGE_LOOP('',(#14618,#14619,#14620,#14621));
#2797=EDGE_LOOP('',(#14622,#14623,#14624,#14625));
#2798=EDGE_LOOP('',(#14626,#14627,#14628,#14629));
#2799=EDGE_LOOP('',(#14630,#14631,#14632,#14633));
#2800=EDGE_LOOP('',(#14634,#14635,#14636,#14637));
#2801=EDGE_LOOP('',(#14638,#14639,#14640,#14641));
#2802=EDGE_LOOP('',(#14642,#14643,#14644,#14645,#14646,#14647,#14648,#14649,
#14650,#14651,#14652,#14653,#14654,#14655));
#2803=EDGE_LOOP('',(#14656,#14657,#14658,#14659));
#2804=EDGE_LOOP('',(#14660,#14661,#14662,#14663));
#2805=EDGE_LOOP('',(#14664,#14665,#14666,#14667));
#2806=EDGE_LOOP('',(#14668,#14669,#14670,#14671));
#2807=EDGE_LOOP('',(#14672,#14673,#14674,#14675));
#2808=EDGE_LOOP('',(#14676,#14677,#14678,#14679));
#2809=EDGE_LOOP('',(#14680,#14681,#14682,#14683));
#2810=EDGE_LOOP('',(#14684,#14685,#14686,#14687));
#2811=EDGE_LOOP('',(#14688,#14689,#14690,#14691));
#2812=EDGE_LOOP('',(#14692,#14693,#14694,#14695));
#2813=EDGE_LOOP('',(#14696,#14697,#14698,#14699));
#2814=EDGE_LOOP('',(#14700,#14701,#14702,#14703));
#2815=EDGE_LOOP('',(#14704,#14705,#14706,#14707));
#2816=EDGE_LOOP('',(#14708,#14709,#14710,#14711));
#2817=EDGE_LOOP('',(#14712,#14713,#14714,#14715,#14716,#14717,#14718,#14719,
#14720,#14721,#14722,#14723,#14724,#14725));
#2818=EDGE_LOOP('',(#14726,#14727,#14728,#14729));
#2819=EDGE_LOOP('',(#14730,#14731,#14732,#14733));
#2820=EDGE_LOOP('',(#14734,#14735,#14736,#14737));
#2821=EDGE_LOOP('',(#14738,#14739,#14740,#14741));
#2822=EDGE_LOOP('',(#14742,#14743,#14744,#14745));
#2823=EDGE_LOOP('',(#14746,#14747,#14748,#14749));
#2824=EDGE_LOOP('',(#14750,#14751,#14752,#14753));
#2825=EDGE_LOOP('',(#14754,#14755,#14756,#14757));
#2826=EDGE_LOOP('',(#14758,#14759,#14760,#14761));
#2827=EDGE_LOOP('',(#14762,#14763,#14764,#14765));
#2828=EDGE_LOOP('',(#14766,#14767,#14768,#14769));
#2829=EDGE_LOOP('',(#14770,#14771,#14772,#14773));
#2830=EDGE_LOOP('',(#14774,#14775,#14776,#14777));
#2831=EDGE_LOOP('',(#14778,#14779,#14780,#14781));
#2832=EDGE_LOOP('',(#14782,#14783,#14784,#14785,#14786,#14787,#14788,#14789,
#14790,#14791,#14792,#14793,#14794,#14795));
#2833=EDGE_LOOP('',(#14796,#14797,#14798,#14799));
#2834=EDGE_LOOP('',(#14800,#14801,#14802,#14803));
#2835=EDGE_LOOP('',(#14804,#14805,#14806,#14807));
#2836=EDGE_LOOP('',(#14808,#14809,#14810,#14811));
#2837=EDGE_LOOP('',(#14812,#14813,#14814,#14815));
#2838=EDGE_LOOP('',(#14816,#14817,#14818,#14819));
#2839=EDGE_LOOP('',(#14820,#14821,#14822,#14823));
#2840=EDGE_LOOP('',(#14824,#14825,#14826,#14827));
#2841=EDGE_LOOP('',(#14828,#14829,#14830,#14831));
#2842=EDGE_LOOP('',(#14832,#14833,#14834,#14835));
#2843=EDGE_LOOP('',(#14836,#14837,#14838,#14839));
#2844=EDGE_LOOP('',(#14840,#14841,#14842,#14843));
#2845=EDGE_LOOP('',(#14844,#14845,#14846,#14847));
#2846=EDGE_LOOP('',(#14848,#14849,#14850,#14851));
#2847=EDGE_LOOP('',(#14852,#14853,#14854,#14855,#14856,#14857,#14858,#14859,
#14860,#14861,#14862,#14863,#14864,#14865));
#2848=EDGE_LOOP('',(#14866,#14867,#14868,#14869,#14870,#14871,#14872,#14873,
#14874));
#2849=EDGE_LOOP('',(#14875,#14876,#14877,#14878,#14879,#14880,#14881,#14882));
#2850=EDGE_LOOP('',(#14883,#14884,#14885,#14886));
#2851=EDGE_LOOP('',(#14887));
#2852=EDGE_LOOP('',(#14888,#14889,#14890,#14891));
#2853=EDGE_LOOP('',(#14892));
#2854=EDGE_LOOP('',(#14893,#14894,#14895,#14896));
#2855=EDGE_LOOP('',(#14897));
#2856=EDGE_LOOP('',(#14898,#14899,#14900,#14901));
#2857=EDGE_LOOP('',(#14902));
#2858=EDGE_LOOP('',(#14903,#14904,#14905,#14906));
#2859=EDGE_LOOP('',(#14907));
#2860=EDGE_LOOP('',(#14908,#14909,#14910,#14911));
#2861=EDGE_LOOP('',(#14912));
#2862=EDGE_LOOP('',(#14913,#14914,#14915,#14916));
#2863=EDGE_LOOP('',(#14917));
#2864=EDGE_LOOP('',(#14918));
#2865=EDGE_LOOP('',(#14919));
#2866=EDGE_LOOP('',(#14920));
#2867=EDGE_LOOP('',(#14921,#14922,#14923,#14924));
#2868=EDGE_LOOP('',(#14925,#14926,#14927,#14928));
#2869=EDGE_LOOP('',(#14929,#14930,#14931,#14932));
#2870=EDGE_LOOP('',(#14933));
#2871=EDGE_LOOP('',(#14934));
#2872=EDGE_LOOP('',(#14935));
#2873=EDGE_LOOP('',(#14936));
#2874=EDGE_LOOP('',(#14937));
#2875=EDGE_LOOP('',(#14938));
#2876=EDGE_LOOP('',(#14939));
#2877=EDGE_LOOP('',(#14940));
#2878=EDGE_LOOP('',(#14941,#14942,#14943,#14944));
#2879=EDGE_LOOP('',(#14945,#14946,#14947,#14948));
#2880=EDGE_LOOP('',(#14949,#14950,#14951,#14952));
#2881=EDGE_LOOP('',(#14953));
#2882=EDGE_LOOP('',(#14954));
#2883=EDGE_LOOP('',(#14955,#14956,#14957,#14958));
#2884=EDGE_LOOP('',(#14959,#14960,#14961,#14962));
#2885=EDGE_LOOP('',(#14963,#14964,#14965,#14966));
#2886=EDGE_LOOP('',(#14967));
#2887=EDGE_LOOP('',(#14968));
#2888=EDGE_LOOP('',(#14969,#14970,#14971,#14972));
#2889=EDGE_LOOP('',(#14973,#14974,#14975,#14976));
#2890=EDGE_LOOP('',(#14977,#14978,#14979,#14980));
#2891=EDGE_LOOP('',(#14981));
#2892=EDGE_LOOP('',(#14982));
#2893=EDGE_LOOP('',(#14983,#14984,#14985,#14986));
#2894=EDGE_LOOP('',(#14987,#14988,#14989,#14990,#14991,#14992,#14993,#14994));
#2895=EDGE_LOOP('',(#14995,#14996,#14997,#14998));
#2896=EDGE_LOOP('',(#14999,#15000,#15001,#15002));
#2897=EDGE_LOOP('',(#15003,#15004,#15005,#15006));
#2898=EDGE_LOOP('',(#15007,#15008,#15009,#15010));
#2899=EDGE_LOOP('',(#15011,#15012,#15013,#15014));
#2900=EDGE_LOOP('',(#15015,#15016,#15017,#15018,#15019,#15020,#15021,#15022));
#2901=EDGE_LOOP('',(#15023,#15024,#15025,#15026));
#2902=EDGE_LOOP('',(#15027,#15028,#15029,#15030));
#2903=EDGE_LOOP('',(#15031,#15032,#15033,#15034,#15035,#15036,#15037,#15038));
#2904=EDGE_LOOP('',(#15039,#15040,#15041,#15042));
#2905=EDGE_LOOP('',(#15043,#15044,#15045,#15046,#15047,#15048,#15049,#15050,
#15051,#15052,#15053,#15054,#15055,#15056,#15057,#15058,#15059,#15060,#15061,
#15062,#15063,#15064,#15065,#15066,#15067,#15068,#15069,#15070,#15071,#15072,
#15073,#15074,#15075,#15076,#15077,#15078,#15079,#15080,#15081,#15082,#15083,
#15084,#15085,#15086,#15087,#15088,#15089,#15090,#15091,#15092,#15093,#15094,
#15095,#15096,#15097,#15098,#15099,#15100,#15101,#15102,#15103,#15104,#15105,
#15106,#15107,#15108,#15109,#15110,#15111,#15112,#15113,#15114,#15115,#15116,
#15117,#15118,#15119,#15120,#15121,#15122,#15123,#15124,#15125,#15126,#15127,
#15128,#15129,#15130));
#2906=EDGE_LOOP('',(#15131,#15132,#15133,#15134));
#2907=EDGE_LOOP('',(#15135,#15136,#15137,#15138));
#2908=EDGE_LOOP('',(#15139,#15140,#15141,#15142));
#2909=EDGE_LOOP('',(#15143,#15144,#15145,#15146));
#2910=EDGE_LOOP('',(#15147,#15148,#15149,#15150));
#2911=EDGE_LOOP('',(#15151,#15152,#15153,#15154));
#2912=EDGE_LOOP('',(#15155,#15156,#15157,#15158));
#2913=EDGE_LOOP('',(#15159,#15160,#15161,#15162));
#2914=EDGE_LOOP('',(#15163,#15164,#15165,#15166));
#2915=EDGE_LOOP('',(#15167,#15168,#15169,#15170));
#2916=EDGE_LOOP('',(#15171,#15172,#15173,#15174));
#2917=EDGE_LOOP('',(#15175,#15176,#15177,#15178));
#2918=EDGE_LOOP('',(#15179,#15180,#15181,#15182));
#2919=EDGE_LOOP('',(#15183,#15184,#15185,#15186,#15187));
#2920=EDGE_LOOP('',(#15188,#15189,#15190,#15191,#15192,#15193));
#2921=EDGE_LOOP('',(#15194));
#2922=EDGE_LOOP('',(#15195));
#2923=EDGE_LOOP('',(#15196,#15197,#15198,#15199,#15200));
#2924=EDGE_LOOP('',(#15201));
#2925=EDGE_LOOP('',(#15202));
#2926=EDGE_LOOP('',(#15203,#15204,#15205,#15206,#15207,#15208,#15209));
#2927=EDGE_LOOP('',(#15210,#15211,#15212,#15213));
#2928=EDGE_LOOP('',(#15214,#15215,#15216,#15217));
#2929=EDGE_LOOP('',(#15218,#15219,#15220,#15221,#15222,#15223,#15224));
#2930=EDGE_LOOP('',(#15225,#15226,#15227,#15228));
#2931=EDGE_LOOP('',(#15229,#15230,#15231,#15232,#15233,#15234,#15235));
#2932=EDGE_LOOP('',(#15236,#15237,#15238,#15239));
#2933=EDGE_LOOP('',(#15240,#15241,#15242,#15243));
#2934=EDGE_LOOP('',(#15244,#15245,#15246,#15247,#15248,#15249,#15250));
#2935=EDGE_LOOP('',(#15251,#15252,#15253,#15254));
#2936=EDGE_LOOP('',(#15255,#15256,#15257,#15258,#15259,#15260,#15261));
#2937=EDGE_LOOP('',(#15262,#15263,#15264,#15265));
#2938=EDGE_LOOP('',(#15266,#15267,#15268,#15269));
#2939=EDGE_LOOP('',(#15270,#15271,#15272,#15273,#15274,#15275,#15276));
#2940=EDGE_LOOP('',(#15277,#15278,#15279,#15280));
#2941=EDGE_LOOP('',(#15281,#15282,#15283,#15284,#15285,#15286,#15287));
#2942=EDGE_LOOP('',(#15288,#15289,#15290,#15291));
#2943=EDGE_LOOP('',(#15292,#15293,#15294,#15295,#15296));
#2944=EDGE_LOOP('',(#15297,#15298,#15299,#15300,#15301,#15302,#15303));
#2945=EDGE_LOOP('',(#15304,#15305,#15306,#15307));
#2946=EDGE_LOOP('',(#15308,#15309,#15310,#15311,#15312,#15313,#15314));
#2947=EDGE_LOOP('',(#15315,#15316,#15317,#15318));
#2948=EDGE_LOOP('',(#15319,#15320,#15321,#15322));
#2949=EDGE_LOOP('',(#15323,#15324,#15325,#15326,#15327,#15328,#15329));
#2950=EDGE_LOOP('',(#15330,#15331,#15332,#15333));
#2951=EDGE_LOOP('',(#15334,#15335,#15336,#15337,#15338,#15339,#15340));
#2952=EDGE_LOOP('',(#15341,#15342,#15343,#15344));
#2953=EDGE_LOOP('',(#15345,#15346,#15347,#15348));
#2954=EDGE_LOOP('',(#15349,#15350,#15351,#15352,#15353,#15354,#15355));
#2955=EDGE_LOOP('',(#15356,#15357,#15358,#15359));
#2956=EDGE_LOOP('',(#15360,#15361,#15362,#15363,#15364,#15365,#15366));
#2957=EDGE_LOOP('',(#15367,#15368,#15369,#15370));
#2958=EDGE_LOOP('',(#15371,#15372,#15373,#15374));
#2959=EDGE_LOOP('',(#15375,#15376,#15377,#15378,#15379,#15380,#15381));
#2960=EDGE_LOOP('',(#15382,#15383,#15384,#15385));
#2961=EDGE_LOOP('',(#15386,#15387,#15388,#15389,#15390,#15391,#15392,#15393));
#2962=EDGE_LOOP('',(#15394,#15395,#15396,#15397));
#2963=EDGE_LOOP('',(#15398,#15399,#15400,#15401,#15402));
#2964=EDGE_LOOP('',(#15403,#15404,#15405,#15406,#15407,#15408,#15409));
#2965=EDGE_LOOP('',(#15410,#15411,#15412,#15413));
#2966=EDGE_LOOP('',(#15414,#15415,#15416,#15417,#15418,#15419,#15420,#15421));
#2967=EDGE_LOOP('',(#15422,#15423,#15424,#15425));
#2968=EDGE_LOOP('',(#15426,#15427,#15428,#15429,#15430));
#2969=EDGE_LOOP('',(#15431,#15432,#15433,#15434,#15435,#15436,#15437));
#2970=EDGE_LOOP('',(#15438,#15439,#15440,#15441));
#2971=EDGE_LOOP('',(#15442,#15443,#15444,#15445,#15446,#15447,#15448,#15449));
#2972=EDGE_LOOP('',(#15450,#15451,#15452,#15453));
#2973=EDGE_LOOP('',(#15454,#15455,#15456,#15457,#15458));
#2974=EDGE_LOOP('',(#15459,#15460,#15461,#15462,#15463,#15464,#15465));
#2975=EDGE_LOOP('',(#15466,#15467,#15468,#15469));
#2976=EDGE_LOOP('',(#15470,#15471,#15472,#15473,#15474,#15475,#15476,#15477));
#2977=EDGE_LOOP('',(#15478,#15479,#15480,#15481));
#2978=EDGE_LOOP('',(#15482,#15483,#15484,#15485,#15486));
#2979=EDGE_LOOP('',(#15487,#15488,#15489,#15490,#15491,#15492,#15493));
#2980=EDGE_LOOP('',(#15494,#15495,#15496,#15497));
#2981=EDGE_LOOP('',(#15498,#15499,#15500,#15501,#15502,#15503,#15504,#15505));
#2982=EDGE_LOOP('',(#15506,#15507,#15508,#15509));
#2983=EDGE_LOOP('',(#15510,#15511,#15512,#15513,#15514));
#2984=EDGE_LOOP('',(#15515,#15516,#15517,#15518,#15519,#15520,#15521));
#2985=EDGE_LOOP('',(#15522,#15523,#15524,#15525));
#2986=EDGE_LOOP('',(#15526,#15527,#15528,#15529,#15530,#15531,#15532,#15533));
#2987=EDGE_LOOP('',(#15534,#15535,#15536,#15537,#15538));
#2988=EDGE_LOOP('',(#15539,#15540,#15541,#15542,#15543));
#2989=EDGE_LOOP('',(#15544,#15545,#15546,#15547,#15548,#15549,#15550,#15551));
#2990=EDGE_LOOP('',(#15552,#15553,#15554,#15555));
#2991=EDGE_LOOP('',(#15556,#15557,#15558,#15559,#15560,#15561,#15562,#15563,
#15564,#15565,#15566,#15567,#15568,#15569,#15570,#15571,#15572,#15573,#15574,
#15575,#15576,#15577,#15578,#15579,#15580,#15581,#15582,#15583,#15584,#15585,
#15586,#15587,#15588,#15589,#15590,#15591,#15592,#15593,#15594,#15595,#15596,
#15597,#15598,#15599,#15600,#15601,#15602,#15603,#15604,#15605,#15606,#15607,
#15608,#15609,#15610,#15611,#15612));
#2992=EDGE_LOOP('',(#15613,#15614,#15615,#15616,#15617,#15618,#15619,#15620,
#15621));
#2993=EDGE_LOOP('',(#15622,#15623,#15624,#15625));
#2994=EDGE_LOOP('',(#15626,#15627,#15628,#15629,#15630));
#2995=EDGE_LOOP('',(#15631,#15632,#15633,#15634,#15635,#15636,#15637));
#2996=EDGE_LOOP('',(#15638,#15639,#15640,#15641));
#2997=EDGE_LOOP('',(#15642,#15643,#15644,#15645));
#2998=EDGE_LOOP('',(#15646,#15647,#15648,#15649,#15650));
#2999=EDGE_LOOP('',(#15651,#15652,#15653,#15654));
#3000=EDGE_LOOP('',(#15655,#15656,#15657,#15658));
#3001=EDGE_LOOP('',(#15659,#15660,#15661,#15662,#15663));
#3002=EDGE_LOOP('',(#15664,#15665,#15666,#15667));
#3003=EDGE_LOOP('',(#15668,#15669,#15670,#15671,#15672,#15673));
#3004=EDGE_LOOP('',(#15674,#15675,#15676,#15677,#15678));
#3005=EDGE_LOOP('',(#15679,#15680,#15681,#15682));
#3006=EDGE_LOOP('',(#15683,#15684,#15685,#15686,#15687,#15688));
#3007=EDGE_LOOP('',(#15689,#15690,#15691,#15692,#15693));
#3008=EDGE_LOOP('',(#15694,#15695,#15696,#15697));
#3009=EDGE_LOOP('',(#15698,#15699,#15700,#15701,#15702,#15703));
#3010=EDGE_LOOP('',(#15704,#15705,#15706,#15707));
#3011=EDGE_LOOP('',(#15708,#15709,#15710,#15711,#15712,#15713));
#3012=EDGE_LOOP('',(#15714,#15715,#15716,#15717,#15718,#15719,#15720,#15721,
#15722,#15723,#15724,#15725,#15726,#15727,#15728));
#3013=EDGE_LOOP('',(#15729,#15730,#15731,#15732));
#3014=EDGE_LOOP('',(#15733,#15734,#15735,#15736));
#3015=EDGE_LOOP('',(#15737,#15738,#15739,#15740,#15741));
#3016=EDGE_LOOP('',(#15742,#15743,#15744,#15745));
#3017=EDGE_LOOP('',(#15746,#15747,#15748,#15749,#15750,#15751));
#3018=EDGE_LOOP('',(#15752,#15753,#15754,#15755,#15756,#15757));
#3019=EDGE_LOOP('',(#15758,#15759,#15760,#15761,#15762));
#3020=EDGE_LOOP('',(#15763,#15764,#15765,#15766));
#3021=EDGE_LOOP('',(#15767,#15768,#15769,#15770,#15771,#15772));
#3022=EDGE_LOOP('',(#15773,#15774,#15775,#15776,#15777,#15778));
#3023=EDGE_LOOP('',(#15779,#15780,#15781,#15782,#15783));
#3024=EDGE_LOOP('',(#15784,#15785,#15786,#15787));
#3025=EDGE_LOOP('',(#15788,#15789,#15790,#15791,#15792,#15793));
#3026=EDGE_LOOP('',(#15794,#15795,#15796,#15797,#15798));
#3027=EDGE_LOOP('',(#15799,#15800,#15801,#15802));
#3028=EDGE_LOOP('',(#15803,#15804,#15805,#15806,#15807));
#3029=EDGE_LOOP('',(#15808,#15809,#15810,#15811,#15812,#15813));
#3030=EDGE_LOOP('',(#15814,#15815,#15816,#15817,#15818));
#3031=EDGE_LOOP('',(#15819,#15820,#15821,#15822));
#3032=EDGE_LOOP('',(#15823,#15824,#15825,#15826,#15827,#15828));
#3033=EDGE_LOOP('',(#15829,#15830,#15831,#15832,#15833,#15834));
#3034=EDGE_LOOP('',(#15835,#15836,#15837,#15838,#15839));
#3035=EDGE_LOOP('',(#15840,#15841,#15842,#15843));
#3036=EDGE_LOOP('',(#15844,#15845,#15846,#15847,#15848,#15849));
#3037=EDGE_LOOP('',(#15850,#15851,#15852,#15853,#15854,#15855));
#3038=EDGE_LOOP('',(#15856,#15857,#15858,#15859,#15860));
#3039=EDGE_LOOP('',(#15861,#15862,#15863,#15864));
#3040=EDGE_LOOP('',(#15865,#15866,#15867,#15868,#15869,#15870));
#3041=EDGE_LOOP('',(#15871,#15872,#15873,#15874,#15875,#15876));
#3042=EDGE_LOOP('',(#15877,#15878,#15879,#15880));
#3043=EDGE_LOOP('',(#15881,#15882,#15883,#15884));
#3044=EDGE_LOOP('',(#15885,#15886,#15887,#15888));
#3045=EDGE_LOOP('',(#15889,#15890,#15891,#15892));
#3046=EDGE_LOOP('',(#15893,#15894,#15895,#15896));
#3047=EDGE_LOOP('',(#15897,#15898,#15899,#15900));
#3048=EDGE_LOOP('',(#15901,#15902,#15903,#15904,#15905,#15906));
#3049=EDGE_LOOP('',(#15907,#15908,#15909,#15910));
#3050=EDGE_LOOP('',(#15911,#15912,#15913,#15914,#15915,#15916));
#3051=EDGE_LOOP('',(#15917,#15918,#15919,#15920));
#3052=EDGE_LOOP('',(#15921,#15922,#15923,#15924,#15925,#15926));
#3053=EDGE_LOOP('',(#15927,#15928,#15929,#15930));
#3054=EDGE_LOOP('',(#15931,#15932,#15933,#15934,#15935));
#3055=EDGE_LOOP('',(#15936,#15937,#15938,#15939));
#3056=EDGE_LOOP('',(#15940,#15941,#15942,#15943));
#3057=EDGE_LOOP('',(#15944,#15945,#15946,#15947));
#3058=EDGE_LOOP('',(#15948,#15949,#15950,#15951));
#3059=EDGE_LOOP('',(#15952,#15953,#15954,#15955));
#3060=EDGE_LOOP('',(#15956,#15957,#15958,#15959));
#3061=EDGE_LOOP('',(#15960,#15961,#15962,#15963));
#3062=EDGE_LOOP('',(#15964,#15965,#15966,#15967));
#3063=EDGE_LOOP('',(#15968,#15969,#15970,#15971));
#3064=EDGE_LOOP('',(#15972,#15973,#15974,#15975));
#3065=EDGE_LOOP('',(#15976,#15977,#15978,#15979));
#3066=EDGE_LOOP('',(#15980,#15981,#15982,#15983));
#3067=EDGE_LOOP('',(#15984,#15985,#15986,#15987));
#3068=EDGE_LOOP('',(#15988,#15989,#15990,#15991,#15992,#15993,#15994,#15995,
#15996,#15997,#15998,#15999,#16000,#16001,#16002,#16003,#16004,#16005,#16006,
#16007,#16008,#16009,#16010,#16011,#16012,#16013,#16014));
#3069=EDGE_LOOP('',(#16015));
#3070=EDGE_LOOP('',(#16016,#16017,#16018,#16019,#16020));
#3071=EDGE_LOOP('',(#16021,#16022,#16023,#16024,#16025));
#3072=EDGE_LOOP('',(#16026,#16027,#16028,#16029,#16030));
#3073=EDGE_LOOP('',(#16031,#16032,#16033,#16034,#16035));
#3074=EDGE_LOOP('',(#16036,#16037,#16038,#16039,#16040));
#3075=EDGE_LOOP('',(#16041,#16042,#16043,#16044,#16045));
#3076=EDGE_LOOP('',(#16046,#16047,#16048,#16049,#16050));
#3077=EDGE_LOOP('',(#16051,#16052,#16053,#16054,#16055));
#3078=EDGE_LOOP('',(#16056,#16057,#16058,#16059));
#3079=EDGE_LOOP('',(#16060,#16061,#16062,#16063));
#3080=EDGE_LOOP('',(#16064,#16065,#16066,#16067));
#3081=EDGE_LOOP('',(#16068,#16069,#16070,#16071));
#3082=EDGE_LOOP('',(#16072,#16073,#16074,#16075,#16076,#16077));
#3083=EDGE_LOOP('',(#16078,#16079,#16080,#16081));
#3084=EDGE_LOOP('',(#16082,#16083,#16084,#16085));
#3085=EDGE_LOOP('',(#16086,#16087,#16088,#16089));
#3086=EDGE_LOOP('',(#16090,#16091,#16092,#16093));
#3087=EDGE_LOOP('',(#16094,#16095,#16096,#16097));
#3088=EDGE_LOOP('',(#16098,#16099,#16100,#16101));
#3089=EDGE_LOOP('',(#16102));
#3090=EDGE_LOOP('',(#16103));
#3091=EDGE_LOOP('',(#16104,#16105,#16106,#16107));
#3092=EDGE_LOOP('',(#16108,#16109,#16110,#16111));
#3093=EDGE_LOOP('',(#16112,#16113,#16114,#16115));
#3094=EDGE_LOOP('',(#16116));
#3095=EDGE_LOOP('',(#16117,#16118,#16119,#16120,#16121,#16122,#16123,#16124,
#16125,#16126,#16127,#16128,#16129,#16130,#16131,#16132,#16133,#16134,#16135,
#16136,#16137,#16138,#16139,#16140,#16141,#16142,#16143,#16144,#16145,#16146,
#16147,#16148,#16149,#16150,#16151,#16152));
#3096=EDGE_LOOP('',(#16153,#16154));
#3097=EDGE_LOOP('',(#16155,#16156,#16157,#16158));
#3098=EDGE_LOOP('',(#16159,#16160));
#3099=EDGE_LOOP('',(#16161,#16162));
#3100=EDGE_LOOP('',(#16163,#16164,#16165,#16166));
#3101=EDGE_LOOP('',(#16167,#16168));
#3102=EDGE_LOOP('',(#16169,#16170));
#3103=EDGE_LOOP('',(#16171,#16172,#16173,#16174));
#3104=EDGE_LOOP('',(#16175,#16176));
#3105=EDGE_LOOP('',(#16177,#16178));
#3106=EDGE_LOOP('',(#16179,#16180,#16181,#16182));
#3107=EDGE_LOOP('',(#16183,#16184));
#3108=EDGE_LOOP('',(#16185,#16186,#16187,#16188,#16189,#16190));
#3109=EDGE_LOOP('',(#16191,#16192,#16193,#16194,#16195,#16196));
#3110=EDGE_LOOP('',(#16197,#16198,#16199,#16200,#16201,#16202,#16203));
#3111=EDGE_LOOP('',(#16204,#16205,#16206,#16207,#16208,#16209));
#3112=EDGE_LOOP('',(#16210,#16211,#16212,#16213,#16214,#16215,#16216,#16217));
#3113=EDGE_LOOP('',(#16218,#16219));
#3114=EDGE_LOOP('',(#16220,#16221));
#3115=EDGE_LOOP('',(#16222,#16223));
#3116=EDGE_LOOP('',(#16224));
#3117=EDGE_LOOP('',(#16225));
#3118=EDGE_LOOP('',(#16226));
#3119=EDGE_LOOP('',(#16227));
#3120=EDGE_LOOP('',(#16228,#16229,#16230,#16231));
#3121=EDGE_LOOP('',(#16232,#16233,#16234,#16235));
#3122=EDGE_LOOP('',(#16236,#16237,#16238,#16239));
#3123=EDGE_LOOP('',(#16240,#16241,#16242,#16243));
#3124=EDGE_LOOP('',(#16244));
#3125=EDGE_LOOP('',(#16245));
#3126=EDGE_LOOP('',(#16246,#16247,#16248,#16249));
#3127=EDGE_LOOP('',(#16250,#16251,#16252,#16253,#16254,#16255,#16256,#16257,
#16258));
#3128=EDGE_LOOP('',(#16259,#16260,#16261,#16262));
#3129=EDGE_LOOP('',(#16263,#16264,#16265,#16266));
#3130=EDGE_LOOP('',(#16267,#16268,#16269,#16270));
#3131=EDGE_LOOP('',(#16271,#16272,#16273,#16274));
#3132=EDGE_LOOP('',(#16275,#16276));
#3133=EDGE_LOOP('',(#16277,#16278));
#3134=EDGE_LOOP('',(#16279,#16280));
#3135=EDGE_LOOP('',(#16281,#16282,#16283,#16284));
#3136=EDGE_LOOP('',(#16285));
#3137=EDGE_LOOP('',(#16286));
#3138=EDGE_LOOP('',(#16287,#16288,#16289,#16290));
#3139=EDGE_LOOP('',(#16291,#16292,#16293,#16294));
#3140=EDGE_LOOP('',(#16295,#16296,#16297,#16298,#16299,#16300,#16301,#16302,
#16303,#16304,#16305,#16306,#16307,#16308,#16309,#16310,#16311,#16312,#16313,
#16314,#16315,#16316,#16317,#16318,#16319,#16320,#16321,#16322,#16323,#16324,
#16325,#16326,#16327,#16328,#16329,#16330,#16331,#16332,#16333,#16334,#16335,
#16336,#16337,#16338,#16339,#16340,#16341,#16342,#16343,#16344,#16345,#16346,
#16347,#16348,#16349,#16350,#16351,#16352,#16353,#16354,#16355,#16356,#16357,
#16358,#16359,#16360,#16361,#16362,#16363,#16364,#16365,#16366,#16367,#16368,
#16369,#16370,#16371,#16372,#16373,#16374,#16375,#16376,#16377,#16378,#16379,
#16380,#16381,#16382,#16383,#16384,#16385,#16386,#16387,#16388,#16389,#16390,
#16391,#16392,#16393,#16394,#16395,#16396,#16397,#16398,#16399,#16400,#16401,
#16402,#16403,#16404,#16405,#16406,#16407,#16408,#16409,#16410,#16411,#16412,
#16413,#16414,#16415,#16416,#16417,#16418,#16419,#16420,#16421,#16422,#16423,
#16424,#16425,#16426,#16427,#16428,#16429,#16430,#16431,#16432,#16433,#16434,
#16435,#16436,#16437,#16438,#16439,#16440,#16441,#16442,#16443,#16444));
#3141=EDGE_LOOP('',(#16445));
#3142=EDGE_LOOP('',(#16446));
#3143=EDGE_LOOP('',(#16447,#16448,#16449,#16450));
#3144=EDGE_LOOP('',(#16451,#16452,#16453,#16454,#16455,#16456,#16457,#16458,
#16459,#16460,#16461,#16462,#16463,#16464,#16465,#16466,#16467,#16468,#16469,
#16470,#16471,#16472,#16473,#16474,#16475,#16476,#16477,#16478,#16479,#16480,
#16481,#16482,#16483,#16484,#16485,#16486,#16487,#16488,#16489,#16490,#16491,
#16492,#16493,#16494,#16495,#16496,#16497,#16498,#16499,#16500,#16501,#16502,
#16503,#16504,#16505,#16506,#16507,#16508,#16509,#16510,#16511,#16512,#16513,
#16514,#16515,#16516,#16517,#16518,#16519,#16520,#16521,#16522,#16523,#16524,
#16525,#16526,#16527,#16528,#16529,#16530,#16531,#16532,#16533,#16534,#16535,
#16536,#16537,#16538,#16539,#16540,#16541,#16542,#16543,#16544,#16545,#16546,
#16547,#16548,#16549,#16550,#16551,#16552,#16553,#16554,#16555,#16556,#16557,
#16558,#16559,#16560,#16561,#16562,#16563,#16564,#16565,#16566,#16567,#16568,
#16569,#16570,#16571,#16572,#16573,#16574,#16575,#16576,#16577,#16578,#16579,
#16580,#16581,#16582,#16583,#16584,#16585,#16586,#16587,#16588,#16589,#16590,
#16591,#16592,#16593,#16594,#16595,#16596,#16597,#16598,#16599,#16600));
#3145=EDGE_LOOP('',(#16601));
#3146=EDGE_LOOP('',(#16602));
#3147=EDGE_LOOP('',(#16603,#16604,#16605,#16606));
#3148=EDGE_LOOP('',(#16607,#16608,#16609,#16610));
#3149=EDGE_LOOP('',(#16611,#16612,#16613,#16614));
#3150=EDGE_LOOP('',(#16615,#16616,#16617,#16618));
#3151=EDGE_LOOP('',(#16619,#16620,#16621,#16622));
#3152=EDGE_LOOP('',(#16623,#16624,#16625,#16626));
#3153=EDGE_LOOP('',(#16627,#16628,#16629,#16630));
#3154=EDGE_LOOP('',(#16631,#16632,#16633,#16634));
#3155=EDGE_LOOP('',(#16635,#16636,#16637,#16638));
#3156=EDGE_LOOP('',(#16639,#16640,#16641,#16642));
#3157=EDGE_LOOP('',(#16643,#16644,#16645,#16646));
#3158=EDGE_LOOP('',(#16647,#16648,#16649,#16650));
#3159=EDGE_LOOP('',(#16651,#16652,#16653,#16654));
#3160=EDGE_LOOP('',(#16655,#16656,#16657,#16658));
#3161=EDGE_LOOP('',(#16659,#16660,#16661,#16662));
#3162=EDGE_LOOP('',(#16663,#16664,#16665,#16666));
#3163=EDGE_LOOP('',(#16667,#16668,#16669,#16670));
#3164=EDGE_LOOP('',(#16671,#16672,#16673,#16674));
#3165=EDGE_LOOP('',(#16675,#16676,#16677,#16678));
#3166=EDGE_LOOP('',(#16679,#16680,#16681,#16682));
#3167=EDGE_LOOP('',(#16683,#16684,#16685,#16686));
#3168=EDGE_LOOP('',(#16687,#16688,#16689,#16690));
#3169=EDGE_LOOP('',(#16691,#16692,#16693,#16694));
#3170=EDGE_LOOP('',(#16695,#16696,#16697,#16698));
#3171=EDGE_LOOP('',(#16699,#16700,#16701,#16702));
#3172=EDGE_LOOP('',(#16703,#16704,#16705,#16706));
#3173=EDGE_LOOP('',(#16707,#16708,#16709,#16710));
#3174=EDGE_LOOP('',(#16711,#16712,#16713,#16714));
#3175=EDGE_LOOP('',(#16715,#16716,#16717,#16718));
#3176=EDGE_LOOP('',(#16719,#16720,#16721,#16722));
#3177=EDGE_LOOP('',(#16723,#16724,#16725,#16726));
#3178=EDGE_LOOP('',(#16727,#16728,#16729,#16730));
#3179=EDGE_LOOP('',(#16731,#16732,#16733,#16734));
#3180=EDGE_LOOP('',(#16735,#16736,#16737,#16738));
#3181=EDGE_LOOP('',(#16739,#16740,#16741,#16742));
#3182=EDGE_LOOP('',(#16743,#16744,#16745,#16746));
#3183=EDGE_LOOP('',(#16747,#16748,#16749,#16750));
#3184=EDGE_LOOP('',(#16751,#16752,#16753,#16754));
#3185=EDGE_LOOP('',(#16755,#16756,#16757,#16758));
#3186=EDGE_LOOP('',(#16759,#16760,#16761,#16762));
#3187=EDGE_LOOP('',(#16763,#16764,#16765,#16766));
#3188=EDGE_LOOP('',(#16767,#16768,#16769,#16770));
#3189=EDGE_LOOP('',(#16771,#16772,#16773,#16774));
#3190=EDGE_LOOP('',(#16775,#16776,#16777,#16778));
#3191=EDGE_LOOP('',(#16779,#16780,#16781,#16782));
#3192=EDGE_LOOP('',(#16783,#16784,#16785,#16786));
#3193=EDGE_LOOP('',(#16787,#16788,#16789,#16790));
#3194=EDGE_LOOP('',(#16791,#16792,#16793,#16794));
#3195=EDGE_LOOP('',(#16795,#16796,#16797,#16798));
#3196=EDGE_LOOP('',(#16799,#16800,#16801,#16802));
#3197=EDGE_LOOP('',(#16803,#16804,#16805,#16806));
#3198=EDGE_LOOP('',(#16807,#16808,#16809,#16810));
#3199=EDGE_LOOP('',(#16811,#16812,#16813,#16814));
#3200=EDGE_LOOP('',(#16815,#16816,#16817,#16818));
#3201=EDGE_LOOP('',(#16819,#16820,#16821,#16822));
#3202=EDGE_LOOP('',(#16823,#16824,#16825,#16826));
#3203=EDGE_LOOP('',(#16827,#16828,#16829,#16830));
#3204=EDGE_LOOP('',(#16831,#16832,#16833,#16834));
#3205=EDGE_LOOP('',(#16835,#16836,#16837,#16838));
#3206=EDGE_LOOP('',(#16839,#16840,#16841,#16842));
#3207=EDGE_LOOP('',(#16843,#16844,#16845,#16846));
#3208=EDGE_LOOP('',(#16847,#16848,#16849,#16850));
#3209=EDGE_LOOP('',(#16851,#16852,#16853,#16854));
#3210=EDGE_LOOP('',(#16855,#16856,#16857,#16858));
#3211=EDGE_LOOP('',(#16859,#16860,#16861,#16862));
#3212=EDGE_LOOP('',(#16863,#16864,#16865,#16866));
#3213=EDGE_LOOP('',(#16867,#16868,#16869,#16870));
#3214=EDGE_LOOP('',(#16871,#16872,#16873,#16874));
#3215=EDGE_LOOP('',(#16875,#16876,#16877,#16878));
#3216=EDGE_LOOP('',(#16879,#16880,#16881,#16882));
#3217=EDGE_LOOP('',(#16883,#16884,#16885,#16886));
#3218=EDGE_LOOP('',(#16887,#16888,#16889,#16890));
#3219=EDGE_LOOP('',(#16891,#16892,#16893,#16894));
#3220=EDGE_LOOP('',(#16895,#16896,#16897,#16898));
#3221=EDGE_LOOP('',(#16899,#16900,#16901,#16902));
#3222=EDGE_LOOP('',(#16903,#16904,#16905,#16906));
#3223=EDGE_LOOP('',(#16907,#16908,#16909,#16910));
#3224=EDGE_LOOP('',(#16911,#16912,#16913,#16914));
#3225=EDGE_LOOP('',(#16915,#16916,#16917,#16918));
#3226=EDGE_LOOP('',(#16919,#16920,#16921,#16922));
#3227=EDGE_LOOP('',(#16923,#16924,#16925,#16926));
#3228=EDGE_LOOP('',(#16927,#16928,#16929,#16930));
#3229=EDGE_LOOP('',(#16931,#16932,#16933,#16934));
#3230=EDGE_LOOP('',(#16935,#16936,#16937,#16938));
#3231=EDGE_LOOP('',(#16939,#16940,#16941,#16942));
#3232=EDGE_LOOP('',(#16943,#16944,#16945,#16946));
#3233=EDGE_LOOP('',(#16947,#16948,#16949,#16950));
#3234=EDGE_LOOP('',(#16951,#16952,#16953,#16954));
#3235=EDGE_LOOP('',(#16955,#16956,#16957,#16958));
#3236=EDGE_LOOP('',(#16959,#16960,#16961,#16962));
#3237=EDGE_LOOP('',(#16963,#16964,#16965,#16966));
#3238=EDGE_LOOP('',(#16967,#16968,#16969,#16970));
#3239=EDGE_LOOP('',(#16971,#16972,#16973,#16974));
#3240=EDGE_LOOP('',(#16975,#16976,#16977,#16978));
#3241=EDGE_LOOP('',(#16979,#16980,#16981,#16982));
#3242=EDGE_LOOP('',(#16983,#16984,#16985,#16986));
#3243=EDGE_LOOP('',(#16987,#16988,#16989,#16990));
#3244=EDGE_LOOP('',(#16991,#16992,#16993,#16994));
#3245=EDGE_LOOP('',(#16995,#16996,#16997,#16998));
#3246=EDGE_LOOP('',(#16999,#17000,#17001,#17002));
#3247=EDGE_LOOP('',(#17003,#17004,#17005,#17006));
#3248=EDGE_LOOP('',(#17007,#17008,#17009,#17010));
#3249=EDGE_LOOP('',(#17011,#17012,#17013,#17014));
#3250=EDGE_LOOP('',(#17015,#17016,#17017,#17018));
#3251=EDGE_LOOP('',(#17019,#17020,#17021,#17022));
#3252=EDGE_LOOP('',(#17023,#17024,#17025,#17026));
#3253=EDGE_LOOP('',(#17027,#17028,#17029,#17030));
#3254=EDGE_LOOP('',(#17031,#17032,#17033,#17034));
#3255=EDGE_LOOP('',(#17035,#17036,#17037,#17038));
#3256=EDGE_LOOP('',(#17039,#17040,#17041,#17042));
#3257=EDGE_LOOP('',(#17043,#17044,#17045,#17046));
#3258=EDGE_LOOP('',(#17047,#17048,#17049,#17050));
#3259=EDGE_LOOP('',(#17051,#17052,#17053,#17054));
#3260=EDGE_LOOP('',(#17055,#17056,#17057,#17058));
#3261=EDGE_LOOP('',(#17059,#17060,#17061,#17062));
#3262=EDGE_LOOP('',(#17063,#17064,#17065,#17066));
#3263=EDGE_LOOP('',(#17067,#17068,#17069,#17070));
#3264=EDGE_LOOP('',(#17071,#17072,#17073,#17074));
#3265=EDGE_LOOP('',(#17075,#17076,#17077,#17078));
#3266=EDGE_LOOP('',(#17079,#17080,#17081,#17082));
#3267=EDGE_LOOP('',(#17083,#17084,#17085,#17086));
#3268=EDGE_LOOP('',(#17087,#17088,#17089,#17090));
#3269=EDGE_LOOP('',(#17091,#17092,#17093,#17094));
#3270=EDGE_LOOP('',(#17095,#17096,#17097,#17098));
#3271=EDGE_LOOP('',(#17099,#17100,#17101,#17102));
#3272=EDGE_LOOP('',(#17103,#17104,#17105,#17106));
#3273=EDGE_LOOP('',(#17107,#17108,#17109,#17110));
#3274=EDGE_LOOP('',(#17111,#17112,#17113,#17114));
#3275=EDGE_LOOP('',(#17115,#17116,#17117,#17118));
#3276=EDGE_LOOP('',(#17119,#17120,#17121,#17122));
#3277=EDGE_LOOP('',(#17123,#17124,#17125,#17126));
#3278=EDGE_LOOP('',(#17127,#17128,#17129,#17130));
#3279=EDGE_LOOP('',(#17131,#17132,#17133,#17134));
#3280=EDGE_LOOP('',(#17135,#17136,#17137,#17138));
#3281=EDGE_LOOP('',(#17139,#17140,#17141,#17142));
#3282=EDGE_LOOP('',(#17143,#17144,#17145,#17146));
#3283=EDGE_LOOP('',(#17147,#17148,#17149,#17150));
#3284=EDGE_LOOP('',(#17151,#17152,#17153,#17154));
#3285=EDGE_LOOP('',(#17155,#17156,#17157,#17158));
#3286=EDGE_LOOP('',(#17159,#17160,#17161,#17162));
#3287=EDGE_LOOP('',(#17163,#17164,#17165,#17166));
#3288=EDGE_LOOP('',(#17167,#17168,#17169,#17170));
#3289=EDGE_LOOP('',(#17171,#17172,#17173,#17174));
#3290=EDGE_LOOP('',(#17175,#17176,#17177,#17178));
#3291=EDGE_LOOP('',(#17179,#17180,#17181,#17182));
#3292=EDGE_LOOP('',(#17183,#17184,#17185,#17186));
#3293=EDGE_LOOP('',(#17187,#17188,#17189,#17190));
#3294=EDGE_LOOP('',(#17191,#17192,#17193,#17194));
#3295=EDGE_LOOP('',(#17195,#17196,#17197,#17198));
#3296=EDGE_LOOP('',(#17199,#17200,#17201,#17202));
#3297=EDGE_LOOP('',(#17203,#17204,#17205,#17206));
#3298=EDGE_LOOP('',(#17207,#17208,#17209,#17210));
#3299=EDGE_LOOP('',(#17211,#17212,#17213,#17214));
#3300=CIRCLE('',#18421,3.442);
#3301=CIRCLE('',#18437,11.);
#3302=CIRCLE('',#18438,32.4);
#3303=CIRCLE('',#18439,32.4);
#3304=CIRCLE('',#18440,32.4);
#3305=CIRCLE('',#18441,32.4);
#3306=CIRCLE('',#18442,32.4);
#3307=CIRCLE('',#18443,32.4);
#3308=CIRCLE('',#18444,32.4);
#3309=CIRCLE('',#18445,32.4);
#3310=CIRCLE('',#18446,32.4);
#3311=CIRCLE('',#18447,32.4);
#3312=CIRCLE('',#18448,32.4);
#3313=CIRCLE('',#18449,32.4);
#3314=CIRCLE('',#18450,32.4);
#3315=CIRCLE('',#18451,32.4);
#3316=CIRCLE('',#18452,32.4);
#3317=CIRCLE('',#18453,32.4);
#3318=CIRCLE('',#18454,32.4);
#3319=CIRCLE('',#18455,32.4);
#3320=CIRCLE('',#18456,32.4);
#3321=CIRCLE('',#18457,32.4);
#3322=CIRCLE('',#18458,32.4);
#3323=CIRCLE('',#18459,32.4);
#3324=CIRCLE('',#18461,2.872);
#3325=CIRCLE('',#18478,9.5);
#3326=CIRCLE('',#18479,10.2572478777138);
#3327=CIRCLE('',#18480,10.2572478777138);
#3328=CIRCLE('',#18482,10.6);
#3329=CIRCLE('',#18484,8.8);
#3330=CIRCLE('',#18533,34.5);
#3331=CIRCLE('',#18534,35.);
#3332=CIRCLE('',#18536,35.);
#3333=CIRCLE('',#18538,34.5);
#3334=CIRCLE('',#18539,35.);
#3335=CIRCLE('',#18541,35.);
#3336=CIRCLE('',#18543,34.5);
#3337=CIRCLE('',#18544,35.);
#3338=CIRCLE('',#18546,35.);
#3339=CIRCLE('',#18548,34.5);
#3340=CIRCLE('',#18549,35.);
#3341=CIRCLE('',#18551,35.);
#3342=CIRCLE('',#18553,34.5);
#3343=CIRCLE('',#18554,35.);
#3344=CIRCLE('',#18556,35.);
#3345=CIRCLE('',#18558,34.5);
#3346=CIRCLE('',#18559,35.);
#3347=CIRCLE('',#18561,35.);
#3348=CIRCLE('',#18563,34.5);
#3349=CIRCLE('',#18564,35.);
#3350=CIRCLE('',#18566,35.);
#3351=CIRCLE('',#18568,34.5);
#3352=CIRCLE('',#18569,35.);
#3353=CIRCLE('',#18571,35.);
#3354=CIRCLE('',#18573,34.5);
#3355=CIRCLE('',#18574,35.);
#3356=CIRCLE('',#18576,35.);
#3357=CIRCLE('',#18578,34.5);
#3358=CIRCLE('',#18579,35.);
#3359=CIRCLE('',#18581,35.);
#3360=CIRCLE('',#18583,34.5);
#3361=CIRCLE('',#18584,35.);
#3362=CIRCLE('',#18586,35.);
#3363=CIRCLE('',#18588,34.5);
#3364=CIRCLE('',#18589,35.);
#3365=CIRCLE('',#18591,35.);
#3366=CIRCLE('',#18593,9.2);
#3367=CIRCLE('',#18594,8.7);
#3368=CIRCLE('',#18596,7.7);
#3369=CIRCLE('',#18598,9.2);
#3370=CIRCLE('',#18600,9.2);
#3371=CIRCLE('',#18601,8.7);
#3372=CIRCLE('',#18603,7.7);
#3373=CIRCLE('',#18605,9.2);
#3374=CIRCLE('',#18608,8.5);
#3375=CIRCLE('',#18609,8.);
#3376=CIRCLE('',#18611,33.);
#3377=CIRCLE('',#18612,32.5);
#3378=CIRCLE('',#18614,33.);
#3379=CIRCLE('',#18615,33.);
#3380=CIRCLE('',#18616,33.);
#3381=CIRCLE('',#18619,8.);
#3382=CIRCLE('',#18620,8.5);
#3383=CIRCLE('',#18623,33.);
#3384=CIRCLE('',#18624,32.5);
#3385=CIRCLE('',#18626,33.);
#3386=CIRCLE('',#18627,33.);
#3387=CIRCLE('',#18628,33.);
#3388=CIRCLE('',#18631,8.);
#3389=CIRCLE('',#18632,8.5);
#3390=CIRCLE('',#18635,33.);
#3391=CIRCLE('',#18636,32.5);
#3392=CIRCLE('',#18638,33.);
#3393=CIRCLE('',#18639,33.);
#3394=CIRCLE('',#18640,33.);
#3395=CIRCLE('',#18643,8.);
#3396=CIRCLE('',#18644,8.5);
#3397=CIRCLE('',#18647,33.);
#3398=CIRCLE('',#18648,32.5);
#3399=CIRCLE('',#18650,33.);
#3400=CIRCLE('',#18651,33.);
#3401=CIRCLE('',#18652,33.);
#3402=CIRCLE('',#18655,8.);
#3403=CIRCLE('',#18656,8.5);
#3404=CIRCLE('',#18659,33.);
#3405=CIRCLE('',#18660,32.5);
#3406=CIRCLE('',#18662,33.);
#3407=CIRCLE('',#18663,33.);
#3408=CIRCLE('',#18664,33.);
#3409=CIRCLE('',#18667,8.);
#3410=CIRCLE('',#18668,8.5);
#3411=CIRCLE('',#18670,32.5);
#3412=CIRCLE('',#18671,8.5);
#3413=CIRCLE('',#18672,32.5);
#3414=CIRCLE('',#18673,8.5);
#3415=CIRCLE('',#18674,32.5);
#3416=CIRCLE('',#18675,8.5);
#3417=CIRCLE('',#18676,32.5);
#3418=CIRCLE('',#18677,8.5);
#3419=CIRCLE('',#18678,32.5);
#3420=CIRCLE('',#18679,8.5);
#3421=CIRCLE('',#18680,32.5);
#3422=CIRCLE('',#18681,8.5);
#3423=CIRCLE('',#18682,32.5);
#3424=CIRCLE('',#18683,14.);
#3425=CIRCLE('',#18685,33.);
#3426=CIRCLE('',#18688,8.);
#3427=CIRCLE('',#18690,8.);
#3428=CIRCLE('',#18693,33.);
#3429=CIRCLE('',#18694,33.);
#3430=CIRCLE('',#18695,33.);
#3431=CIRCLE('',#18698,8.);
#3432=CIRCLE('',#18700,33.);
#3433=CIRCLE('',#18703,33.);
#3434=CIRCLE('',#18704,33.);
#3435=CIRCLE('',#18705,33.);
#3436=CIRCLE('',#18708,8.);
#3437=CIRCLE('',#18710,33.);
#3438=CIRCLE('',#18713,33.);
#3439=CIRCLE('',#18714,33.);
#3440=CIRCLE('',#18715,33.);
#3441=CIRCLE('',#18718,8.);
#3442=CIRCLE('',#18720,33.);
#3443=CIRCLE('',#18723,33.);
#3444=CIRCLE('',#18724,33.);
#3445=CIRCLE('',#18725,33.);
#3446=CIRCLE('',#18728,8.);
#3447=CIRCLE('',#18730,33.);
#3448=CIRCLE('',#18733,33.);
#3449=CIRCLE('',#18734,33.);
#3450=CIRCLE('',#18735,33.);
#3451=CIRCLE('',#18738,8.);
#3452=CIRCLE('',#18740,33.);
#3453=CIRCLE('',#18743,33.);
#3454=CIRCLE('',#18744,33.);
#3455=CIRCLE('',#18745,33.);
#3456=CIRCLE('',#18746,33.);
#3457=CIRCLE('',#18749,33.);
#3458=CIRCLE('',#18750,33.);
#3459=CIRCLE('',#18751,33.);
#3460=CIRCLE('',#18754,8.);
#3461=CIRCLE('',#18757,32.4);
#3462=CIRCLE('',#18759,8.);
#3463=CIRCLE('',#18761,3.442);
#3464=CIRCLE('',#18762,3.442);
#3465=CIRCLE('',#18764,3.442);
#3466=CIRCLE('',#18765,3.442);
#3467=CIRCLE('',#18766,2.872);
#3468=CIRCLE('',#18769,32.4);
#3469=CIRCLE('',#18772,8.);
#3470=CIRCLE('',#18777,8.);
#3471=CIRCLE('',#18782,8.);
#3472=CIRCLE('',#18787,8.);
#3473=CIRCLE('',#18792,8.);
#3474=CIRCLE('',#18797,8.);
#3475=CIRCLE('',#18802,8.);
#3476=CIRCLE('',#18807,8.);
#3477=CIRCLE('',#18812,8.);
#3478=CIRCLE('',#18823,8.5);
#3479=CIRCLE('',#18824,8.5);
#3480=CIRCLE('',#18827,9.2);
#3481=CIRCLE('',#18829,9.2);
#3482=CIRCLE('',#18832,30.);
#3483=CIRCLE('',#18835,30.);
#3484=CIRCLE('',#18838,30.);
#3485=CIRCLE('',#18841,30.);
#3486=CIRCLE('',#18844,30.);
#3487=CIRCLE('',#18847,30.);
#3488=CIRCLE('',#18850,30.);
#3489=CIRCLE('',#18853,30.);
#3490=CIRCLE('',#18856,30.);
#3491=CIRCLE('',#18859,30.);
#3492=CIRCLE('',#18862,30.);
#3493=CIRCLE('',#18865,30.);
#3494=CIRCLE('',#18883,12.);
#3495=CIRCLE('',#18887,8.8);
#3496=CIRCLE('',#18889,7.2);
#3497=CIRCLE('',#18891,6.2);
#3498=CIRCLE('',#18893,5.5);
#3499=CIRCLE('',#18895,5.5);
#3500=CIRCLE('',#18897,5.2);
#3501=CIRCLE('',#18899,3.3);
#3502=CIRCLE('',#18901,3.3);
#3503=CIRCLE('',#18903,3.5);
#3504=CIRCLE('',#18905,3.5);
#3505=CIRCLE('',#18907,2.9);
#3506=CIRCLE('',#18909,2.9);
#3507=CIRCLE('',#18912,3.442);
#3508=CIRCLE('',#18914,3.);
#3509=CIRCLE('',#18923,8.5);
#3510=CIRCLE('',#18924,8.3);
#3511=CIRCLE('',#18926,8.5);
#3512=CIRCLE('',#18928,8.2);
#3513=CIRCLE('',#18930,3.81);
#3514=CIRCLE('',#18932,3.505);
#3515=CIRCLE('',#18934,3.505);
#3516=CIRCLE('',#18936,3.81);
#3517=CIRCLE('',#18941,1.2);
#3518=CIRCLE('',#18944,16.8);
#3519=CIRCLE('',#18945,2.85);
#3520=CIRCLE('',#18946,2.85);
#3521=CIRCLE('',#18947,5.85);
#3522=CIRCLE('',#18948,2.85);
#3523=CIRCLE('',#18950,17.);
#3524=CIRCLE('',#18953,17.);
#3525=CIRCLE('',#18954,16.8);
#3526=CIRCLE('',#18958,2.85);
#3527=CIRCLE('',#18959,2.85);
#3528=CIRCLE('',#18960,5.85);
#3529=CIRCLE('',#18961,2.85);
#3530=CIRCLE('',#18964,2.65);
#3531=CIRCLE('',#18966,2.65);
#3532=CIRCLE('',#18969,2.65);
#3533=CIRCLE('',#18971,2.65);
#3534=CIRCLE('',#18974,2.65);
#3535=CIRCLE('',#18976,2.65);
#3536=CIRCLE('',#18979,1.);
#3537=CIRCLE('',#19165,0.600000000000001);
#3538=CIRCLE('',#19166,0.600000000000001);
#3539=CIRCLE('',#19169,0.6);
#3540=CIRCLE('',#19170,0.6);
#3541=CIRCLE('',#19173,0.600000000000001);
#3542=CIRCLE('',#19174,0.600000000000001);
#3543=CIRCLE('',#19177,0.600000000000001);
#3544=CIRCLE('',#19178,0.600000000000001);
#3545=CIRCLE('',#19181,0.6);
#3546=CIRCLE('',#19182,0.6);
#3547=CIRCLE('',#19185,0.600000000000001);
#3548=CIRCLE('',#19186,0.600000000000001);
#3549=CIRCLE('',#19189,6.6);
#3550=CIRCLE('',#19190,6.6);
#3551=CIRCLE('',#19192,7.6);
#3552=CIRCLE('',#19194,7.6);
#3553=CIRCLE('',#19196,7.6);
#3554=CIRCLE('',#19198,5.75);
#3555=CIRCLE('',#19199,5.55);
#3556=CIRCLE('',#19201,5.75);
#3557=CIRCLE('',#19203,8.3);
#3558=CIRCLE('',#19205,8.5);
#3559=CIRCLE('',#19207,8.5);
#3560=CIRCLE('',#19209,8.3);
#3561=CIRCLE('',#19211,7.8);
#3562=CIRCLE('',#19213,7.6);
#3563=CIRCLE('',#19216,7.3);
#3564=CIRCLE('',#19218,3.81);
#3565=CIRCLE('',#19220,3.505);
#3566=CIRCLE('',#19222,3.505);
#3567=CIRCLE('',#19224,3.81);
#3568=CIRCLE('',#19232,37.6);
#3569=CIRCLE('',#19233,37.6);
#3570=CIRCLE('',#19235,39.);
#3571=CIRCLE('',#19236,38.540427484991);
#3572=CIRCLE('',#19238,39.);
#3573=CIRCLE('',#19239,39.);
#3574=CIRCLE('',#19240,39.);
#3575=CIRCLE('',#19241,39.);
#3576=CIRCLE('',#19242,39.);
#3577=CIRCLE('',#19243,39.);
#3578=CIRCLE('',#19244,39.);
#3579=CIRCLE('',#19245,39.);
#3580=CIRCLE('',#19246,39.);
#3581=CIRCLE('',#19247,39.);
#3582=CIRCLE('',#19248,39.);
#3583=CIRCLE('',#19249,39.);
#3584=CIRCLE('',#19250,39.);
#3585=CIRCLE('',#19251,39.);
#3586=CIRCLE('',#19252,39.);
#3587=CIRCLE('',#19253,39.);
#3588=CIRCLE('',#19254,39.);
#3589=CIRCLE('',#19255,39.);
#3590=CIRCLE('',#19256,39.);
#3591=CIRCLE('',#19257,39.);
#3592=CIRCLE('',#19258,39.);
#3593=CIRCLE('',#19259,39.);
#3594=CIRCLE('',#19260,39.);
#3595=CIRCLE('',#19261,39.);
#3596=CIRCLE('',#19262,39.);
#3597=CIRCLE('',#19263,39.);
#3598=CIRCLE('',#19264,39.);
#3599=CIRCLE('',#19265,39.);
#3600=CIRCLE('',#19266,39.);
#3601=CIRCLE('',#19268,38.540427484991);
#3602=CIRCLE('',#19270,38.540427484991);
#3603=CIRCLE('',#19272,38.540427484991);
#3604=CIRCLE('',#19274,38.540427484991);
#3605=CIRCLE('',#19276,38.540427484991);
#3606=CIRCLE('',#19278,38.540427484991);
#3607=CIRCLE('',#19280,38.540427484991);
#3608=CIRCLE('',#19282,38.540427484991);
#3609=CIRCLE('',#19284,38.540427484991);
#3610=CIRCLE('',#19286,38.540427484991);
#3611=CIRCLE('',#19288,38.540427484991);
#3612=CIRCLE('',#19290,38.540427484991);
#3613=CIRCLE('',#19292,38.540427484991);
#3614=CIRCLE('',#19294,3.825);
#3615=CIRCLE('',#19295,3.525);
#3616=CIRCLE('',#19296,3.525);
#3617=CIRCLE('',#19298,3.525);
#3618=CIRCLE('',#19299,3.525);
#3619=CIRCLE('',#19301,38.5);
#3620=CIRCLE('',#19303,3.825);
#3621=CIRCLE('',#19305,8.1);
#3622=CIRCLE('',#19307,30.6);
#3623=CIRCLE('',#19309,37.6);
#3624=CIRCLE('',#19311,30.6);
#3625=CIRCLE('',#19313,37.6);
#3626=CIRCLE('',#19315,30.6);
#3627=CIRCLE('',#19317,37.6);
#3628=CIRCLE('',#19319,30.6);
#3629=CIRCLE('',#19321,37.6);
#3630=CIRCLE('',#19323,30.6);
#3631=CIRCLE('',#19325,37.6);
#3632=CIRCLE('',#19327,30.6);
#3633=CIRCLE('',#19329,37.6);
#3634=CIRCLE('',#19331,30.6);
#3635=CIRCLE('',#19334,27.);
#3636=CIRCLE('',#19336,37.6);
#3637=CIRCLE('',#19338,27.);
#3638=CIRCLE('',#19340,37.6);
#3639=CIRCLE('',#19342,27.);
#3640=CIRCLE('',#19344,37.6);
#3641=CIRCLE('',#19346,27.);
#3642=CIRCLE('',#19348,37.6);
#3643=CIRCLE('',#19350,27.);
#3644=CIRCLE('',#19352,37.6);
#3645=CIRCLE('',#19354,27.);
#3646=CIRCLE('',#19356,9.2);
#3647=CIRCLE('',#19357,9.2);
#3648=CIRCLE('',#19358,37.6);
#3649=CIRCLE('',#19360,27.);
#3650=CIRCLE('',#19364,8.7);
#3651=CIRCLE('',#19366,8.7);
#3652=CIRCLE('',#19378,4.6);
#3653=CIRCLE('',#19400,4.6);
#3654=CIRCLE('',#19401,4.6);
#3655=CIRCLE('',#19402,4.6);
#3656=CIRCLE('',#19403,4.6);
#3657=CIRCLE('',#19404,4.6);
#3658=CIRCLE('',#19405,4.6);
#3659=CIRCLE('',#19406,4.6);
#3660=CIRCLE('',#19407,4.6);
#3661=CIRCLE('',#19408,3.95);
#3662=CIRCLE('',#19418,3.55);
#3663=CIRCLE('',#19420,3.95);
#3664=CIRCLE('',#19421,3.55);
#3665=CIRCLE('',#19432,6.2);
#3666=CIRCLE('',#19434,6.5);
#3667=CIRCLE('',#19436,6.5);
#3668=CIRCLE('',#19438,6.);
#3669=CIRCLE('',#19442,5.52);
#3670=CIRCLE('',#19443,0.6);
#3671=CIRCLE('',#19445,0.6);
#3672=CIRCLE('',#19447,5.52);
#3673=CIRCLE('',#19449,5.52);
#3674=CIRCLE('',#19450,0.6);
#3675=CIRCLE('',#19452,0.6);
#3676=CIRCLE('',#19454,5.52);
#3677=CIRCLE('',#19456,5.52);
#3678=CIRCLE('',#19457,0.6);
#3679=CIRCLE('',#19459,0.6);
#3680=CIRCLE('',#19461,5.52);
#3681=CIRCLE('',#19463,5.52);
#3682=CIRCLE('',#19464,0.6);
#3683=CIRCLE('',#19466,0.6);
#3684=CIRCLE('',#19468,5.52);
#3685=CIRCLE('',#19474,8.45);
#3686=CIRCLE('',#19475,8.45);
#3687=CIRCLE('',#19477,8.8);
#3688=CIRCLE('',#19479,8.8);
#3689=CIRCLE('',#19481,8.8);
#3690=CIRCLE('',#19483,8.8);
#3691=CIRCLE('',#19484,8.4);
#3692=CIRCLE('',#19487,8.4);
#3693=CIRCLE('',#19489,5.82);
#3694=CIRCLE('',#19491,5.52);
#3695=CIRCLE('',#19493,5.52);
#3696=CIRCLE('',#19495,5.82);
#3697=CIRCLE('',#19499,0.750000000000001);
#3698=CIRCLE('',#19500,0.55);
#3699=CIRCLE('',#19502,0.55);
#3700=CIRCLE('',#19504,0.750000000000001);
#3701=CIRCLE('',#19506,0.750000000000001);
#3702=CIRCLE('',#19508,0.750000000000001);
#3703=CIRCLE('',#19510,0.55);
#3704=CIRCLE('',#19512,0.55);
#3705=B_SPLINE_CURVE_WITH_KNOTS('',3,(#23617,#23618,#23619,#23620,#23621,
#23622,#23623,#23624,#23625,#23626),.UNSPECIFIED.,.F.,.F.,(4,3,3,4),(-4.0929304201303,
-3.96712820430096,-2.97534615322572,-2.06773127522693),.UNSPECIFIED.);
#3706=B_SPLINE_CURVE_WITH_KNOTS('',3,(#23629,#23630,#23631,#23632,#23633,
#23634,#23635),.UNSPECIFIED.,.F.,.F.,(4,3,4),(0.,0.991782051075235,1.1163935086858),
 .UNSPECIFIED.);
#3707=B_SPLINE_CURVE_WITH_KNOTS('',3,(#23640,#23641,#23642,#23643,#23644,
#23645,#23646,#23647,#23648,#23649,#23650,#23651,#23652,#23653,#23654,#23655,
#23656,#23657,#23658,#23659,#23660,#23661),.UNSPECIFIED.,.F.,.F.,(4,3,3,
3,3,3,3,4),(-10.37611572731,-9.9178205107524,-8.92603845967716,-7.93425640860193,
-6.94247435752668,-5.95069230645144,-4.9589102553762,-4.0929304201303),
 .UNSPECIFIED.);
#3708=B_SPLINE_CURVE_WITH_KNOTS('',3,(#23662,#23663,#23664,#23665,#23666,
#23667,#23668,#23669,#23670,#23671,#23672,#23673,#23674,#23675,#23676,#23677,
#23678,#23679,#23680,#23681,#23682,#23683),.UNSPECIFIED.,.F.,.F.,(4,3,3,
3,3,3,3,4),(1.1163935086858,1.98356410215048,2.97534615322572,3.96712820430096,
4.9589102553762,5.95069230645144,6.94247435752668,7.39957881586548),
 .UNSPECIFIED.);
#3709=B_SPLINE_CURVE_WITH_KNOTS('',3,(#23688,#23689,#23690,#23691,#23692,
#23693,#23694,#23695,#23696,#23697,#23698,#23699,#23700,#23701,#23702,#23703,
#23704,#23705,#23706,#23707,#23708,#23709),.UNSPECIFIED.,.F.,.F.,(4,3,3,
3,3,3,3,4),(-16.6593010344895,-15.8685128172038,-14.8767307661286,-13.8849487150534,
-12.8931666639781,-11.9013846129029,-10.9096025618276,-10.37611572731),
 .UNSPECIFIED.);
#3710=B_SPLINE_CURVE_WITH_KNOTS('',3,(#23710,#23711,#23712,#23713,#23714,
#23715,#23716,#23717,#23718,#23719,#23720,#23721,#23722,#23723,#23724,#23725,
#23726,#23727,#23728,#23729,#23730,#23731),.UNSPECIFIED.,.F.,.F.,(4,3,3,
3,3,3,3,4),(7.39957881586548,7.93425640860192,8.92603845967716,9.9178205107524,
10.9096025618276,11.9013846129029,12.8931666639781,13.682764123045),
 .UNSPECIFIED.);
#3711=B_SPLINE_CURVE_WITH_KNOTS('',3,(#23736,#23737,#23738,#23739,#23740,
#23741,#23742,#23743,#23744,#23745,#23746,#23747,#23748,#23749,#23750,#23751,
#23752,#23753,#23754,#23755,#23756,#23757,#23758,#23759,#23760),
 .UNSPECIFIED.,.F.,.F.,(4,3,3,3,3,3,3,3,4),(-22.9424863416691,-22.8109871747305,
-21.8192051236553,-20.8274230725801,-19.8356410215048,-18.8438589704296,
-17.8520769193543,-16.8602948682791,-16.6593010344895),.UNSPECIFIED.);
#3712=B_SPLINE_CURVE_WITH_KNOTS('',3,(#23761,#23762,#23763,#23764,#23765,
#23766,#23767,#23768,#23769,#23770,#23771,#23772,#23773,#23774,#23775,#23776,
#23777,#23778,#23779,#23780,#23781,#23782,#23783,#23784,#23785),
 .UNSPECIFIED.,.F.,.F.,(4,3,3,3,3,3,3,3,4),(13.682764123045,13.8849487150534,
14.8767307661286,15.8685128172039,16.8602948682791,17.8520769193543,18.8438589704296,
19.8356410215048,19.9659494302246),.UNSPECIFIED.);
#3713=B_SPLINE_CURVE_WITH_KNOTS('',3,(#23790,#23791,#23792,#23793,#23794,
#23795,#23796,#23797,#23798,#23799,#23800,#23801,#23802,#23803,#23804,#23805,
#23806,#23807,#23808,#23809,#23810,#23811),.UNSPECIFIED.,.F.,.F.,(4,3,3,
3,3,3,3,4),(-29.2256716488488,-28.761679481182,-27.7698974301067,-26.7781153790315,
-25.7863333279563,-24.794551276881,-23.8027692258058,-22.9424863416691),
 .UNSPECIFIED.);
#3714=B_SPLINE_CURVE_WITH_KNOTS('',3,(#23812,#23813,#23814,#23815,#23816,
#23817,#23818,#23819,#23820,#23821,#23822,#23823,#23824,#23825,#23826,#23827,
#23828,#23829,#23830,#23831,#23832,#23833),.UNSPECIFIED.,.F.,.F.,(4,3,3,
3,3,3,3,4),(19.9659494302246,20.8274230725801,21.8192051236553,22.8109871747305,
23.8027692258058,24.794551276881,25.7863333279562,26.2491347374043),
 .UNSPECIFIED.);
#3715=B_SPLINE_CURVE_WITH_KNOTS('',3,(#23838,#23839,#23840,#23841,#23842,
#23843,#23844,#23845,#23846,#23847,#23848,#23849,#23850,#23851,#23852,#23853,
#23854,#23855,#23856,#23857,#23858,#23859),.UNSPECIFIED.,.F.,.F.,(4,3,3,
3,3,3,3,4),(-35.5088569560282,-34.7123717876334,-33.7205897365582,-32.7288076854829,
-31.7370256344077,-30.7452435833325,-29.7534615322572,-29.2256716488488),
 .UNSPECIFIED.);
#3716=B_SPLINE_CURVE_WITH_KNOTS('',3,(#23860,#23861,#23862,#23863,#23864,
#23865,#23866,#23867,#23868,#23869,#23870,#23871,#23872,#23873,#23874,#23875,
#23876,#23877,#23878,#23879,#23880,#23881),.UNSPECIFIED.,.F.,.F.,(4,3,3,
3,3,3,3,4),(26.2491347374043,26.7781153790315,27.7698974301067,28.761679481182,
29.7534615322572,30.7452435833325,31.7370256344077,32.5323200445837),
 .UNSPECIFIED.);
#3717=B_SPLINE_CURVE_WITH_KNOTS('',3,(#23886,#23887,#23888,#23889,#23890,
#23891,#23892,#23893,#23894,#23895,#23896,#23897,#23898,#23899,#23900,#23901,
#23902,#23903,#23904,#23905,#23906,#23907,#23908,#23909,#23910),
 .UNSPECIFIED.,.F.,.F.,(4,3,3,3,3,3,3,3,4),(-41.7920422632079,-41.6548461451601,
-40.6630640940849,-39.6712820430096,-38.6794999919344,-37.6877179408591,
-36.6959358897839,-35.7041538387087,-35.5088569560282),.UNSPECIFIED.);
#3718=B_SPLINE_CURVE_WITH_KNOTS('',3,(#23911,#23912,#23913,#23914,#23915,
#23916,#23917,#23918,#23919,#23920,#23921,#23922,#23923,#23924,#23925,#23926,
#23927,#23928,#23929,#23930,#23931,#23932,#23933,#23934,#23935),
 .UNSPECIFIED.,.F.,.F.,(4,3,3,3,3,3,3,3,4),(32.5323200445837,32.7288076854829,
33.7205897365582,34.7123717876334,35.7041538387086,36.6959358897839,37.6877179408591,
38.6794999919344,38.8155053517634),.UNSPECIFIED.);
#3719=B_SPLINE_CURVE_WITH_KNOTS('',3,(#23940,#23941,#23942,#23943,#23944,
#23945,#23946,#23947,#23948,#23949,#23950,#23951,#23952,#23953,#23954,#23955,
#23956,#23957,#23958,#23959,#23960,#23961),.UNSPECIFIED.,.F.,.F.,(4,3,3,
3,3,3,3,4),(-48.0752275703874,-47.6055384516115,-46.6137564005363,-45.6219743494611,
-44.6301922983858,-43.6384102473106,-42.6466281962353,-41.7920422632079),
 .UNSPECIFIED.);
#3720=B_SPLINE_CURVE_WITH_KNOTS('',3,(#23962,#23963,#23964,#23965,#23966,
#23967,#23968,#23969,#23970,#23971,#23972,#23973,#23974,#23975,#23976,#23977,
#23978,#23979,#23980,#23981,#23982,#23983),.UNSPECIFIED.,.F.,.F.,(4,3,3,
3,3,3,3,4),(38.8155053517634,39.6712820430096,40.6630640940849,41.6548461451601,
42.6466281962353,43.6384102473106,44.6301922983858,45.0986906589429),
 .UNSPECIFIED.);
#3721=B_SPLINE_CURVE_WITH_KNOTS('',3,(#23988,#23989,#23990,#23991,#23992,
#23993,#23994,#23995,#23996,#23997,#23998,#23999,#24000,#24001,#24002,#24003,
#24004,#24005,#24006,#24007,#24008,#24009),.UNSPECIFIED.,.F.,.F.,(4,3,3,
3,3,3,3,4),(-54.358412877567,-53.556230758063,-52.5644487069877,-51.5726666559125,
-50.5808846048373,-49.589102553762,-48.5973205026868,-48.0752275703874),
 .UNSPECIFIED.);
#3722=B_SPLINE_CURVE_WITH_KNOTS('',3,(#24010,#24011,#24012,#24013,#24014,
#24015,#24016,#24017,#24018,#24019,#24020,#24021,#24022,#24023,#24024,#24025,
#24026,#24027,#24028,#24029,#24030,#24031),.UNSPECIFIED.,.F.,.F.,(4,3,3,
3,3,3,3,4),(45.0986906589429,45.6219743494611,46.6137564005363,47.6055384516115,
48.5973205026868,49.589102553762,50.5808846048373,51.3818759661225),
 .UNSPECIFIED.);
#3723=B_SPLINE_CURVE_WITH_KNOTS('',3,(#24036,#24037,#24038,#24039,#24040,
#24041,#24042,#24043,#24044,#24045,#24046,#24047,#24048,#24049,#24050,#24051,
#24052,#24053,#24054,#24055,#24056,#24057,#24058,#24059,#24060),
 .UNSPECIFIED.,.F.,.F.,(4,3,3,3,3,3,3,3,4),(-60.6415981847467,-60.4987051155897,
-59.5069230645144,-58.5151410134392,-57.5233589623639,-56.5315769112887,
-55.5397948602135,-54.5480128091382,-54.358412877567),.UNSPECIFIED.);
#3724=B_SPLINE_CURVE_WITH_KNOTS('',3,(#24061,#24062,#24063,#24064,#24065,
#24066,#24067,#24068,#24069,#24070,#24071,#24072,#24073,#24074,#24075,#24076,
#24077,#24078,#24079,#24080,#24081,#24082,#24083,#24084,#24085),
 .UNSPECIFIED.,.F.,.F.,(4,3,3,3,3,3,3,3,4),(51.3818759661225,51.5726666559125,
52.5644487069878,53.556230758063,54.5480128091382,55.5397948602135,56.5315769112887,
57.523358962364,57.6650612733022),.UNSPECIFIED.);
#3725=B_SPLINE_CURVE_WITH_KNOTS('',3,(#24090,#24091,#24092,#24093,#24094,
#24095,#24096,#24097,#24098,#24099,#24100,#24101,#24102,#24103,#24104,#24105,
#24106,#24107,#24108,#24109,#24110,#24111),.UNSPECIFIED.,.F.,.F.,(4,3,3,
3,3,3,3,4),(-66.9247834919262,-66.4493974220411,-65.4576153709659,-64.4658333198906,
-63.4740512688154,-62.4822692177402,-61.4904871666649,-60.6415981847467),
 .UNSPECIFIED.);
#3726=B_SPLINE_CURVE_WITH_KNOTS('',3,(#24112,#24113,#24114,#24115,#24116,
#24117,#24118,#24119,#24120,#24121,#24122,#24123,#24124,#24125,#24126,#24127,
#24128,#24129,#24130,#24131,#24132,#24133),.UNSPECIFIED.,.F.,.F.,(4,3,3,
3,3,3,3,4),(57.6650612733022,58.5151410134392,59.5069230645144,60.4987051155897,
61.4904871666649,62.4822692177402,63.4740512688154,63.9482465804817),
 .UNSPECIFIED.);
#3727=B_SPLINE_CURVE_WITH_KNOTS('',3,(#24138,#24139,#24140,#24141,#24142,
#24143,#24144,#24145,#24146,#24147,#24148,#24149,#24150,#24151,#24152,#24153,
#24154,#24155,#24156,#24157,#24158,#24159),.UNSPECIFIED.,.F.,.F.,(4,3,3,
3,3,3,3,4),(-73.2079687991058,-72.4000897284926,-71.4083076774173,-70.4165256263421,
-69.4247435752668,-68.4329615241916,-67.4411794731163,-66.9247834919262),
 .UNSPECIFIED.);
#3728=B_SPLINE_CURVE_WITH_KNOTS('',3,(#24160,#24161,#24162,#24163,#24164,
#24165,#24166,#24167,#24168,#24169,#24170,#24171,#24172,#24173,#24174,#24175,
#24176,#24177,#24178,#24179,#24180,#24181),.UNSPECIFIED.,.F.,.F.,(4,3,3,
3,3,3,3,4),(63.9482465804817,64.4658333198906,65.4576153709659,66.4493974220411,
67.4411794731163,68.4329615241916,69.4247435752668,70.2314318876613),
 .UNSPECIFIED.);
#3729=B_SPLINE_CURVE_WITH_KNOTS('',3,(#24186,#24187,#24188,#24189,#24190,
#24191,#24192,#24193,#24194,#24195,#24196,#24197,#24198,#24199,#24200,#24201,
#24202,#24203,#24204,#24205,#24206,#24207,#24208,#24209,#24210),
 .UNSPECIFIED.,.F.,.F.,(4,3,3,3,3,3,3,3,4),(-79.4911541062855,-79.3425640860193,
-78.350782034944,-77.3589999838688,-76.3672179327935,-75.3754358817183,
-74.383653830643,-73.3918717795678,-73.2079687991058),.UNSPECIFIED.);
#3730=B_SPLINE_CURVE_WITH_KNOTS('',3,(#24211,#24212,#24213,#24214,#24215,
#24216,#24217,#24218,#24219,#24220,#24221,#24222,#24223,#24224,#24225,#24226,
#24227,#24228,#24229,#24230,#24231,#24232,#24233,#24234,#24235),
 .UNSPECIFIED.,.F.,.F.,(4,3,3,3,3,3,3,3,4),(70.2314318876613,70.4165256263421,
71.4083076774173,72.4000897284925,73.3918717795678,74.383653830643,75.3754358817183,
76.3672179327935,76.514617194841),.UNSPECIFIED.);
#3731=B_SPLINE_CURVE_WITH_KNOTS('',3,(#24240,#24241,#24242,#24243,#24244,
#24245,#24246,#24247,#24248,#24249,#24250,#24251,#24252,#24253,#24254,#24255,
#24256,#24257,#24258,#24259,#24260,#24261),.UNSPECIFIED.,.F.,.F.,(4,3,3,
3,3,3,3,4),(-85.774339413465,-85.2932563924707,-84.3014743413955,-83.3096922903202,
-82.317910239245,-81.3261281881697,-80.3343461370945,-79.4911541062855),
 .UNSPECIFIED.);
#3732=B_SPLINE_CURVE_WITH_KNOTS('',3,(#24262,#24263,#24264,#24265,#24266,
#24267,#24268,#24269,#24270,#24271,#24272,#24273,#24274,#24275,#24276,#24277,
#24278,#24279,#24280,#24281,#24282,#24283),.UNSPECIFIED.,.F.,.F.,(4,3,3,
3,3,3,3,4),(76.514617194841,77.3589999838687,78.350782034944,79.3425640860192,
80.3343461370945,81.3261281881697,82.317910239245,82.7978025020205),
 .UNSPECIFIED.);
#3733=B_SPLINE_CURVE_WITH_KNOTS('',3,(#24288,#24289,#24290,#24291,#24292,
#24293,#24294,#24295,#24296,#24297,#24298,#24299,#24300,#24301,#24302,#24303,
#24304,#24305,#24306,#24307,#24308,#24309),.UNSPECIFIED.,.F.,.F.,(4,3,3,
3,3,3,3,4),(-92.0575247206446,-91.2439486989222,-90.2521666478469,-89.2603845967717,
-88.2686025456964,-87.2768204946212,-86.2850384435459,-85.774339413465),
 .UNSPECIFIED.);
#3734=B_SPLINE_CURVE_WITH_KNOTS('',3,(#24310,#24311,#24312,#24313,#24314,
#24315,#24316,#24317,#24318,#24319,#24320,#24321,#24322,#24323,#24324,#24325,
#24326,#24327,#24328,#24329,#24330,#24331),.UNSPECIFIED.,.F.,.F.,(4,3,3,
3,3,3,3,4),(82.7978025020205,83.3096922903202,84.3014743413955,85.2932563924707,
86.2850384435459,87.2768204946212,88.2686025456964,89.0809878092001),
 .UNSPECIFIED.);
#3735=B_SPLINE_CURVE_WITH_KNOTS('',3,(#24336,#24337,#24338,#24339,#24340,
#24341,#24342,#24343,#24344,#24345,#24346,#24347,#24348,#24349,#24350,#24351,
#24352,#24353,#24354,#24355,#24356,#24357,#24358,#24359,#24360),
 .UNSPECIFIED.,.F.,.F.,(4,3,3,3,3,3,3,3,4),(-98.3407100278241,-98.1864230564488,
-97.1946410053736,-96.2028589542983,-95.2110769032231,-94.2192948521479,
-93.2275128010726,-92.2357307499974,-92.0575247206446),.UNSPECIFIED.);
#3736=B_SPLINE_CURVE_WITH_KNOTS('',3,(#24361,#24362,#24363,#24364,#24365,
#24366,#24367,#24368,#24369,#24370,#24371,#24372,#24373,#24374,#24375,#24376,
#24377,#24378,#24379,#24380,#24381,#24382,#24383,#24384,#24385),
 .UNSPECIFIED.,.F.,.F.,(4,3,3,3,3,3,3,3,4),(89.0809878092001,89.2603845967717,
90.2521666478469,91.2439486989221,92.2357307499974,93.2275128010726,94.2192948521479,
95.2110769032231,95.3641731163798),.UNSPECIFIED.);
#3737=B_SPLINE_CURVE_WITH_KNOTS('',3,(#24670,#24671,#24672,#24673,#24674,
#24675,#24676,#24677,#24678,#24679,#24680,#24681,#24682),.UNSPECIFIED.,
 .F.,.F.,(4,3,3,3,4),(-0.621212683296683,-0.547442578207368,-0.286906424613279,
-0.13635260812343,-0.0501381164492948),.UNSPECIFIED.);
#3738=B_SPLINE_CURVE_WITH_KNOTS('',3,(#24684,#24685,#24686,#24687,#24688,
#24689),.UNSPECIFIED.,.F.,.F.,(4,2,4),(-0.59625459278609,-0.430840814871636,
-0.228304293786418),.UNSPECIFIED.);
#3739=B_SPLINE_CURVE_WITH_KNOTS('',3,(#24691,#24692,#24693,#24694),
 .UNSPECIFIED.,.F.,.F.,(4,4),(-7.28045043043161,-7.11297879609542),
 .UNSPECIFIED.);
#3740=B_SPLINE_CURVE_WITH_KNOTS('',3,(#24704,#24705,#24706,#24707,#24708,
#24709,#24710,#24711,#24712,#24713,#24714,#24715,#24716,#24717,#24718,#24719,
#24720,#24721,#24722,#24723,#24724,#24725,#24726,#24727,#24728,#24729,#24730,
#24731,#24732,#24733,#24734,#24735,#24736,#24737,#24738,#24739,#24740,#24741,
#24742,#24743,#24744,#24745,#24746,#24747,#24748,#24749,#24750,#24751,#24752,
#24753,#24754,#24755,#24756,#24757,#24758,#24759,#24760,#24761,#24762,#24763,
#24764,#24765,#24766,#24767,#24768,#24769,#24770),.UNSPECIFIED.,.F.,.F.,
(4,3,3,3,3,3,3,3,3,3,3,3,3,3,3,3,3,3,3,3,3,3,4),(-7.11297879609542,-7.10146924893286,
-5.58665127018164,-5.35053694579391,-5.18292437028481,-4.93518995665546,
-4.59847254575879,-4.20592684575953,-3.66025783498759,-3.16635853426091,
-2.76138423965328,-2.31987517722514,-2.01229466828823,-1.72292721736197,
-1.60295645902473,-1.18526991652666,-0.932600063372656,-0.806265136795657,
-0.720980394300845,-0.679930210218657,-0.615963294349632,-0.164312231354017,
0.),.UNSPECIFIED.);
#3741=B_SPLINE_CURVE_WITH_KNOTS('',3,(#24774,#24775,#24776,#24777),
 .UNSPECIFIED.,.F.,.F.,(4,4),(-0.123320533354435,0.),.UNSPECIFIED.);
#3742=B_SPLINE_CURVE_WITH_KNOTS('',3,(#24779,#24780,#24781,#24782,#24783,
#24784),.UNSPECIFIED.,.F.,.F.,(4,2,4),(-1.20932024771483,-0.985380063173393,
-0.454839283541959),.UNSPECIFIED.);
#3743=B_SPLINE_CURVE_WITH_KNOTS('',3,(#24786,#24787,#24788,#24789),
 .UNSPECIFIED.,.F.,.F.,(4,4),(-0.123345114071721,0.),.UNSPECIFIED.);
#3744=B_SPLINE_CURVE_WITH_KNOTS('',3,(#24793,#24794,#24795,#24796,#24797,
#24798,#24799,#24800,#24801,#24802,#24803,#24804,#24805,#24806,#24807,#24808,
#24809,#24810,#24811,#24812,#24813,#24814,#24815,#24816,#24817,#24818,#24819,
#24820,#24821,#24822,#24823,#24824,#24825,#24826,#24827,#24828,#24829,#24830,
#24831,#24832,#24833,#24834,#24835,#24836,#24837,#24838,#24839,#24840,#24841,
#24842,#24843,#24844,#24845,#24846,#24847,#24848,#24849,#24850,#24851,#24852,
#24853,#24854,#24855,#24856,#24857,#24858,#24859,#24860,#24861,#24862,#24863,
#24864,#24865),.UNSPECIFIED.,.F.,.F.,(4,3,3,3,3,3,3,3,3,3,3,3,3,3,3,3,3,
3,3,3,3,3,3,3,4),(-12.8459374903622,-11.4794095596864,-10.7961455943485,
-10.3238102702983,-10.1128816290106,-9.79002513500549,-7.17546445018599,
-5.86818410777624,-5.21454393657137,-4.88772385096893,-4.68535987608564,
-4.56090376536649,-4.42075803997013,-3.48474489263661,-2.76035534392185,
-2.17493233268881,-1.74712655326283,-1.70292711374468,-1.28137423833938,
-0.996111179634618,-0.765912925480064,-0.547442578207694,-0.286906424613352,
-0.136326843594367,-0.0501381164492894),.UNSPECIFIED.);
#3745=B_SPLINE_CURVE_WITH_KNOTS('',3,(#24867,#24868,#24869,#24870,#24871,
#24872),.UNSPECIFIED.,.F.,.F.,(4,2,4),(-0.993618385713602,-0.861681629743272,
-0.62552951637108),.UNSPECIFIED.);
#3746=B_SPLINE_CURVE_WITH_KNOTS('',3,(#24874,#24875,#24876,#24877,#24878,
#24879,#24880,#24881,#24882,#24883,#24884,#24885,#24886,#24887,#24888,#24889,
#24890,#24891,#24892,#24893,#24894,#24895,#24896,#24897,#24898,#24899,#24900,
#24901,#24902,#24903,#24904,#24905,#24906,#24907,#24908,#24909,#24910,#24911,
#24912,#24913,#24914,#24915,#24916,#24917,#24918,#24919,#24920,#24921,#24922,
#24923,#24924,#24925,#24926,#24927,#24928,#24929,#24930,#24931,#24932,#24933,
#24934,#24935,#24936,#24937,#24938,#24939,#24940),.UNSPECIFIED.,.F.,.F.,
(4,3,3,3,3,3,3,3,3,3,3,3,3,3,3,3,3,3,3,3,3,3,4),(-7.28045043097461,-7.10146924951175,
-5.58665127099474,-5.3505385242668,-5.18292571362766,-4.93518995738714,
-4.59847254647905,-4.20592684649596,-3.66025783571592,-3.16635853508255,
-2.76138424004969,-2.31987517755785,-2.01230406739047,-1.72292916443561,
-1.60295645915655,-1.18526991660116,-0.932600063410003,-0.806265136814425,
-0.720980394325866,-0.679930210218847,-0.615963294364446,-0.164312231361294,
0.),.UNSPECIFIED.);
#3747=B_SPLINE_CURVE_WITH_KNOTS('',3,(#24944,#24945,#24946,#24947),
 .UNSPECIFIED.,.F.,.F.,(4,4),(-0.123320533354439,0.),.UNSPECIFIED.);
#3748=B_SPLINE_CURVE_WITH_KNOTS('',3,(#24949,#24950,#24951,#24952),
 .UNSPECIFIED.,.F.,.F.,(4,4),(-1.0626156692464,-0.306410932880036),
 .UNSPECIFIED.);
#3749=B_SPLINE_CURVE_WITH_KNOTS('',3,(#24954,#24955,#24956,#24957),
 .UNSPECIFIED.,.F.,.F.,(4,4),(-0.12334511407167,0.),.UNSPECIFIED.);
#3750=B_SPLINE_CURVE_WITH_KNOTS('',3,(#24961,#24962,#24963,#24964,#24965,
#24966,#24967,#24968,#24969,#24970,#24971,#24972,#24973,#24974,#24975,#24976,
#24977,#24978,#24979,#24980,#24981,#24982,#24983,#24984,#24985,#24986,#24987,
#24988,#24989,#24990,#24991,#24992,#24993,#24994,#24995,#24996,#24997,#24998,
#24999,#25000,#25001,#25002,#25003,#25004,#25005,#25006,#25007,#25008,#25009,
#25010,#25011,#25012,#25013,#25014,#25015,#25016,#25017,#25018,#25019,#25020,
#25021,#25022,#25023,#25024,#25025,#25026,#25027,#25028,#25029,#25030,#25031,
#25032,#25033),.UNSPECIFIED.,.F.,.F.,(4,3,3,3,3,3,3,3,3,3,3,3,3,3,3,3,3,
3,3,3,3,3,3,3,4),(-12.8459374829188,-11.4794095553317,-10.7961455915381,
-10.3238102685133,-10.1128816277446,-9.79002513405492,-7.17546444972407,
-5.86818410755865,-5.21454393647594,-4.88772385093459,-4.68535987595121,
-4.56090376539323,-4.4207580397955,-3.48474489237297,-2.76035534392132,
-2.17493233268991,-1.74712655325337,-1.70292711374332,-1.28137423833823,
-0.996111179633743,-0.765912925479433,-0.547442578207301,-0.286906424613261,
-0.136326843593883,-0.0501381164492951),.UNSPECIFIED.);
#3751=B_SPLINE_CURVE_WITH_KNOTS('',3,(#25035,#25036,#25037,#25038,#25039,
#25040),.UNSPECIFIED.,.F.,.F.,(4,2,4),(-0.562962425256162,-0.401675631762058,
-0.194993927866297),.UNSPECIFIED.);
#3752=B_SPLINE_CURVE_WITH_KNOTS('',3,(#25042,#25043,#25044,#25045,#25046,
#25047,#25048,#25049,#25050,#25051,#25052,#25053,#25054,#25055,#25056,#25057,
#25058,#25059,#25060,#25061,#25062,#25063,#25064,#25065,#25066,#25067,#25068,
#25069,#25070,#25071,#25072,#25073,#25074,#25075,#25076,#25077,#25078,#25079,
#25080,#25081,#25082,#25083,#25084,#25085,#25086,#25087,#25088,#25089,#25090,
#25091,#25092,#25093,#25094,#25095,#25096,#25097,#25098,#25099,#25100,#25101,
#25102,#25103,#25104,#25105,#25106,#25107,#25108),.UNSPECIFIED.,.F.,.F.,
(4,3,3,3,3,3,3,3,3,3,3,3,3,3,3,3,3,3,3,3,3,3,4),(-7.28045043032899,-7.10146924891762,
-5.58665127078463,-5.3505385241117,-5.18292571340915,-4.93518995720784,
-4.59847254633886,-4.20592684642313,-3.6602578357137,-3.16635853522375,
-2.761384239933,-2.31987517752994,-2.01230406745978,-1.72292916434363,-1.60295645905542,
-1.18526991655219,-0.932600063385415,-0.806265136802025,-0.720980394296157,
-0.679930210218636,-0.615963294341316,-0.16431223136616,0.),
 .UNSPECIFIED.);
#3753=B_SPLINE_CURVE_WITH_KNOTS('',3,(#25112,#25113,#25114,#25115),
 .UNSPECIFIED.,.F.,.F.,(4,4),(-0.123320533354441,0.),.UNSPECIFIED.);
#3754=B_SPLINE_CURVE_WITH_KNOTS('',3,(#25117,#25118,#25119,#25120,#25121,
#25122),.UNSPECIFIED.,.F.,.F.,(4,2,4),(-1.35394250197628,-0.852961572903344,
-0.599740178024191),.UNSPECIFIED.);
#3755=B_SPLINE_CURVE_WITH_KNOTS('',3,(#25124,#25125,#25126,#25127),
 .UNSPECIFIED.,.F.,.F.,(4,4),(-0.12334511407174,0.),.UNSPECIFIED.);
#3756=B_SPLINE_CURVE_WITH_KNOTS('',3,(#25131,#25132,#25133,#25134,#25135,
#25136,#25137,#25138,#25139,#25140,#25141,#25142,#25143,#25144,#25145,#25146,
#25147,#25148,#25149,#25150,#25151,#25152,#25153,#25154,#25155,#25156,#25157,
#25158,#25159,#25160,#25161,#25162,#25163,#25164,#25165,#25166,#25167,#25168,
#25169,#25170,#25171,#25172,#25173,#25174,#25175,#25176,#25177,#25178,#25179,
#25180,#25181,#25182,#25183,#25184,#25185,#25186,#25187,#25188,#25189,#25190,
#25191,#25192,#25193,#25194,#25195,#25196,#25197,#25198,#25199,#25200,#25201,
#25202,#25203),.UNSPECIFIED.,.F.,.F.,(4,3,3,3,3,3,3,3,3,3,3,3,3,3,3,3,3,
3,3,3,3,3,3,3,4),(-12.8459375038567,-11.4794095705419,-10.7961456038845,
-10.3238102789195,-10.112881637227,-9.79002514266153,-7.1754644540322,-5.86818410971753,
-5.2145439375602,-4.88772385148153,-4.68535987651687,-4.56090376540287,
-4.42075804010368,-3.4847448928061,-2.76035534392402,-2.17493233269109,
-1.74712655325811,-1.70292711374465,-1.28137423833928,-0.996111179634543,
-0.765912925480012,-0.547442578207666,-0.286906424613349,-0.136326843594312,
-0.0501381164492891),.UNSPECIFIED.);
#3757=B_SPLINE_CURVE_WITH_KNOTS('',3,(#25205,#25206,#25207,#25208,#25209,
#25210),.UNSPECIFIED.,.F.,.F.,(4,2,4),(-0.59625459278609,-0.430840814871637,
-0.228304293786418),.UNSPECIFIED.);
#3758=B_SPLINE_CURVE_WITH_KNOTS('',3,(#25212,#25213,#25214,#25215,#25216,
#25217,#25218,#25219,#25220,#25221,#25222,#25223,#25224,#25225,#25226,#25227,
#25228,#25229,#25230,#25231,#25232,#25233,#25234,#25235,#25236,#25237,#25238,
#25239,#25240,#25241,#25242,#25243,#25244,#25245,#25246,#25247,#25248,#25249,
#25250,#25251,#25252,#25253,#25254,#25255,#25256,#25257,#25258,#25259,#25260,
#25261,#25262,#25263,#25264,#25265,#25266,#25267,#25268,#25269,#25270,#25271,
#25272,#25273,#25274,#25275,#25276,#25277,#25278),.UNSPECIFIED.,.F.,.F.,
(4,3,3,3,3,3,3,3,3,3,3,3,3,3,3,3,3,3,3,3,3,3,4),(-7.28045043166272,-7.10146925011317,
-5.58665127095826,-5.35053852414499,-5.18292571362894,-4.93518995732684,
-4.59847254636421,-4.2059268462769,-3.66025783539328,-3.16635853453117,
-2.76138423998915,-2.31987517746889,-2.01230406724825,-1.72292916446406,
-1.60295645919639,-1.18526991661974,-0.932600063420101,-0.806265136820283,
-0.72098039431399,-0.679930210220465,-0.615963294353296,-0.164312231344775,
0.),.UNSPECIFIED.);
#3759=B_SPLINE_CURVE_WITH_KNOTS('',3,(#25282,#25283,#25284,#25285),
 .UNSPECIFIED.,.F.,.F.,(4,4),(-0.123320533354419,0.),.UNSPECIFIED.);
#3760=B_SPLINE_CURVE_WITH_KNOTS('',3,(#25287,#25288,#25289,#25290,#25291,
#25292),.UNSPECIFIED.,.F.,.F.,(4,2,4),(-1.20932024771483,-0.985380063173395,
-0.454839283541961),.UNSPECIFIED.);
#3761=B_SPLINE_CURVE_WITH_KNOTS('',3,(#25294,#25295,#25296,#25297),
 .UNSPECIFIED.,.F.,.F.,(4,4),(-0.123345114071717,0.),.UNSPECIFIED.);
#3762=B_SPLINE_CURVE_WITH_KNOTS('',3,(#25301,#25302,#25303,#25304,#25305,
#25306,#25307,#25308,#25309,#25310,#25311,#25312,#25313,#25314,#25315,#25316,
#25317,#25318,#25319,#25320,#25321,#25322,#25323,#25324,#25325,#25326,#25327,
#25328,#25329,#25330,#25331,#25332,#25333,#25334,#25335,#25336,#25337,#25338,
#25339,#25340,#25341,#25342,#25343,#25344,#25345,#25346,#25347,#25348,#25349,
#25350,#25351,#25352,#25353,#25354,#25355,#25356,#25357,#25358,#25359,#25360,
#25361,#25362,#25363,#25364,#25365,#25366,#25367,#25368,#25369,#25370,#25371,
#25372,#25373),.UNSPECIFIED.,.F.,.F.,(4,3,3,3,3,3,3,3,3,3,3,3,3,3,3,3,3,
3,3,3,3,3,3,3,4),(-12.845937481397,-11.4794095526284,-10.7961455882441,
-10.3238102648368,-10.1128816238599,-9.79002513019444,-7.1754644477685,
-5.86818410655552,-5.21454393594904,-4.88772385064579,-4.68535987568061,
-4.56090376534255,-4.42075803979776,-3.48474489238989,-2.76035534391794,
-2.17493233268459,-1.7471265532667,-1.7029271137431,-1.28137423833835,-0.996111179633872,
-0.765912925479539,-0.547442578207378,-0.286906424613282,-0.136326843594111,
-0.0501381164492929),.UNSPECIFIED.);
#3763=B_SPLINE_CURVE_WITH_KNOTS('',3,(#25375,#25376,#25377,#25378,#25379,
#25380),.UNSPECIFIED.,.F.,.F.,(4,2,4),(-0.993618385713604,-0.861681629743274,
-0.625529516371081),.UNSPECIFIED.);
#3764=B_SPLINE_CURVE_WITH_KNOTS('',3,(#25382,#25383,#25384,#25385,#25386,
#25387,#25388,#25389,#25390,#25391,#25392,#25393,#25394,#25395,#25396,#25397,
#25398,#25399,#25400,#25401,#25402,#25403,#25404,#25405,#25406,#25407,#25408,
#25409,#25410,#25411,#25412,#25413,#25414,#25415,#25416,#25417,#25418,#25419,
#25420,#25421,#25422,#25423,#25424,#25425,#25426,#25427,#25428,#25429,#25430,
#25431,#25432,#25433,#25434,#25435,#25436,#25437,#25438,#25439,#25440,#25441,
#25442,#25443,#25444,#25445,#25446,#25447,#25448),.UNSPECIFIED.,.F.,.F.,
(4,3,3,3,3,3,3,3,3,3,3,3,3,3,3,3,3,3,3,3,3,3,4),(-7.28045042893884,-7.10146924747538,
-5.58665126903134,-5.35053852232403,-5.18292571185153,-4.93518995565818,
-4.59847254483662,-4.2059268449215,-3.66025783426991,-3.16635853364197,
-2.76138423916958,-2.31987517683752,-2.01230406676,-1.7229291640395,-1.60295645881592,
-1.18526991641048,-0.932600063313362,-0.806265136764801,-0.720980394288129,
-0.67993021021624,-0.615963294347702,-0.164312231346664,0.),
 .UNSPECIFIED.);
#3765=B_SPLINE_CURVE_WITH_KNOTS('',3,(#25452,#25453,#25454,#25455),
 .UNSPECIFIED.,.F.,.F.,(4,4),(-0.123320533354399,0.),.UNSPECIFIED.);
#3766=B_SPLINE_CURVE_WITH_KNOTS('',3,(#25457,#25458,#25459,#25460),
 .UNSPECIFIED.,.F.,.F.,(4,4),(-1.0626156692464,-0.306410932880038),
 .UNSPECIFIED.);
#3767=B_SPLINE_CURVE_WITH_KNOTS('',3,(#25462,#25463,#25464,#25465),
 .UNSPECIFIED.,.F.,.F.,(4,4),(-0.123345114071698,0.),.UNSPECIFIED.);
#3768=B_SPLINE_CURVE_WITH_KNOTS('',3,(#25469,#25470,#25471,#25472,#25473,
#25474,#25475,#25476,#25477,#25478,#25479,#25480,#25481,#25482,#25483,#25484,
#25485,#25486,#25487,#25488,#25489,#25490,#25491,#25492,#25493,#25494,#25495,
#25496,#25497,#25498,#25499,#25500,#25501,#25502,#25503,#25504,#25505,#25506,
#25507,#25508,#25509,#25510,#25511,#25512,#25513,#25514,#25515,#25516,#25517,
#25518,#25519,#25520,#25521,#25522,#25523,#25524,#25525,#25526,#25527,#25528,
#25529,#25530,#25531,#25532,#25533,#25534,#25535,#25536,#25537,#25538,#25539,
#25540,#25541),.UNSPECIFIED.,.F.,.F.,(4,3,3,3,3,3,3,3,3,3,3,3,3,3,3,3,3,
3,3,3,3,3,3,3,4),(-12.8459374966351,-11.47940956567,-10.7961456001875,-10.3238102760087,
-10.112881634705,-9.79002514042822,-7.17546445291215,-5.86818410915412,
-5.2145439372751,-4.88772385133559,-4.68535987628659,-4.56090376539608,
-4.42075803990238,-3.48474489262088,-2.76035534392035,-2.17493233268499,
-1.74712655327526,-1.70292711374321,-1.28137423833862,-0.996111179634085,
-0.765912925479667,-0.547442578207445,-0.286906424613299,-0.136326843594094,
-0.0501381164492935),.UNSPECIFIED.);
#3769=B_SPLINE_CURVE_WITH_KNOTS('',3,(#25543,#25544,#25545,#25546,#25547,
#25548),.UNSPECIFIED.,.F.,.F.,(4,2,4),(-0.562962425256162,-0.401675631762059,
-0.194993927866297),.UNSPECIFIED.);
#3770=B_SPLINE_CURVE_WITH_KNOTS('',3,(#25550,#25551,#25552,#25553,#25554,
#25555,#25556,#25557,#25558,#25559,#25560,#25561,#25562,#25563,#25564,#25565,
#25566,#25567,#25568,#25569,#25570,#25571,#25572,#25573,#25574,#25575,#25576,
#25577,#25578,#25579,#25580,#25581,#25582,#25583,#25584,#25585,#25586,#25587,
#25588,#25589,#25590,#25591,#25592,#25593,#25594,#25595,#25596,#25597,#25598,
#25599,#25600,#25601,#25602,#25603,#25604,#25605,#25606,#25607,#25608,#25609,
#25610,#25611,#25612,#25613,#25614,#25615,#25616),.UNSPECIFIED.,.F.,.F.,
(4,3,3,3,3,3,3,3,3,3,3,3,3,3,3,3,3,3,3,3,3,3,4),(-7.28045043082453,-7.10146924927971,
-5.58665127018918,-5.35053852339042,-5.18292571293016,-4.93518995664928,
-4.59847254572338,-4.20592684566866,-3.6602578348416,-3.16635853399249,
-2.76138423964393,-2.31987517718532,-2.01230406700153,-1.72292916430381,
-1.60295645905806,-1.18526991654249,-0.932600063380627,-0.806265136799696,
-0.720980394307554,-0.679930210218765,-0.615963294354504,-0.164312231365093,
0.),.UNSPECIFIED.);
#3771=B_SPLINE_CURVE_WITH_KNOTS('',3,(#25620,#25621,#25622,#25623),
 .UNSPECIFIED.,.F.,.F.,(4,4),(-0.123320533354414,0.),.UNSPECIFIED.);
#3772=B_SPLINE_CURVE_WITH_KNOTS('',3,(#25625,#25626,#25627,#25628,#25629,
#25630),.UNSPECIFIED.,.F.,.F.,(4,2,4),(-1.35394250197628,-0.852961572903346,
-0.59974017802419),.UNSPECIFIED.);
#3773=B_SPLINE_CURVE_WITH_KNOTS('',3,(#25632,#25633,#25634,#25635),
 .UNSPECIFIED.,.F.,.F.,(4,4),(-0.123345114071673,0.),.UNSPECIFIED.);
#3774=B_SPLINE_CURVE_WITH_KNOTS('',3,(#25639,#25640,#25641,#25642,#25643,
#25644,#25645,#25646,#25647,#25648,#25649,#25650,#25651,#25652,#25653,#25654,
#25655,#25656,#25657,#25658,#25659,#25660,#25661,#25662,#25663,#25664,#25665,
#25666,#25667,#25668,#25669,#25670,#25671,#25672,#25673,#25674,#25675,#25676,
#25677,#25678,#25679,#25680,#25681,#25682,#25683,#25684,#25685,#25686,#25687,
#25688,#25689,#25690,#25691,#25692,#25693,#25694,#25695,#25696,#25697,#25698,
#25699,#25700,#25701,#25702,#25703,#25704,#25705,#25706,#25707,#25708,#25709,
#25710,#25711),.UNSPECIFIED.,.F.,.F.,(4,3,3,3,3,3,3,3,3,3,3,3,3,3,3,3,3,
3,3,3,3,3,3,3,4),(-12.8459374941425,-11.4794095636326,-10.7961455983776,
-10.3238102743478,-10.1128816331227,-9.79002513892905,-7.17546445215169,
-5.86818410876301,-5.21454393706867,-4.8877238512215,-4.68535987616866,
-4.56090376537433,-4.42075803987497,-3.48474489239197,-2.76035534391279,
-2.17493233267342,-1.74712655332313,-1.70292711374052,-1.28137423833797,
-0.996111179633762,-0.765912925479437,-0.5474425782073,-0.286906424613261,
-0.136326843593853,-0.0501381164492956),.UNSPECIFIED.);
#3775=B_SPLINE_CURVE_WITH_KNOTS('',3,(#25713,#25714,#25715,#25716,#25717,
#25718),.UNSPECIFIED.,.F.,.F.,(4,2,4),(-0.59625459278609,-0.430840814871637,
-0.228304293786418),.UNSPECIFIED.);
#3776=B_SPLINE_CURVE_WITH_KNOTS('',3,(#25720,#25721,#25722,#25723,#25724,
#25725,#25726,#25727,#25728,#25729,#25730,#25731,#25732,#25733,#25734,#25735,
#25736,#25737,#25738,#25739,#25740,#25741,#25742,#25743,#25744,#25745,#25746,
#25747,#25748,#25749,#25750,#25751,#25752,#25753,#25754,#25755,#25756,#25757,
#25758,#25759,#25760,#25761,#25762,#25763,#25764,#25765,#25766,#25767,#25768,
#25769,#25770,#25771,#25772,#25773,#25774,#25775,#25776,#25777,#25778,#25779,
#25780,#25781,#25782,#25783,#25784,#25785,#25786),.UNSPECIFIED.,.F.,.F.,
(4,3,3,3,3,3,3,3,3,3,3,3,3,3,3,3,3,3,3,3,3,3,4),(-7.28045043046879,-7.10146924897955,
-5.5866512702956,-5.35053852355109,-5.18292571300685,-4.93518995676392,
-4.59847254587039,-4.20592684588041,-3.66025783511541,-3.16635853441469,
-2.7613842397294,-2.31987517727554,-2.01230406711462,-1.72292916430658,
-1.6029564590523,-1.18526991653489,-0.932600063375318,-0.806265136795533,
-0.72098039430825,-0.679930210215748,-0.615963294352945,-0.164312231215415,
0.),.UNSPECIFIED.);
#3777=B_SPLINE_CURVE_WITH_KNOTS('',3,(#25790,#25791,#25792,#25793),
 .UNSPECIFIED.,.F.,.F.,(4,4),(-0.123320533354419,0.),.UNSPECIFIED.);
#3778=B_SPLINE_CURVE_WITH_KNOTS('',3,(#25795,#25796,#25797,#25798,#25799,
#25800),.UNSPECIFIED.,.F.,.F.,(4,2,4),(-1.20932024771483,-0.985380063173395,
-0.454839283541961),.UNSPECIFIED.);
#3779=B_SPLINE_CURVE_WITH_KNOTS('',3,(#25802,#25803,#25804,#25805),
 .UNSPECIFIED.,.F.,.F.,(4,4),(-0.123345114071701,0.),.UNSPECIFIED.);
#3780=B_SPLINE_CURVE_WITH_KNOTS('',3,(#25809,#25810,#25811,#25812,#25813,
#25814,#25815,#25816,#25817,#25818,#25819,#25820,#25821,#25822,#25823,#25824,
#25825,#25826,#25827,#25828,#25829,#25830,#25831,#25832,#25833,#25834,#25835,
#25836,#25837,#25838,#25839,#25840,#25841,#25842,#25843,#25844,#25845,#25846,
#25847,#25848,#25849,#25850,#25851,#25852,#25853,#25854,#25855,#25856,#25857,
#25858,#25859,#25860,#25861,#25862,#25863,#25864,#25865,#25866,#25867,#25868,
#25869,#25870,#25871,#25872,#25873,#25874,#25875,#25876,#25877,#25878,#25879,
#25880,#25881),.UNSPECIFIED.,.F.,.F.,(4,3,3,3,3,3,3,3,3,3,3,3,3,3,3,3,3,
3,3,3,3,3,3,3,4),(-12.8459374808793,-11.4794095526363,-10.7961455885147,
-10.3238102652891,-10.1128816243932,-9.79002513076713,-7.17546444805649,
-5.86818410670117,-5.21454393602351,-4.88772385068468,-4.68535987570999,
-4.56090376534585,-4.42075803974874,-3.48474489224273,-2.7603553439125,
-2.1749323326753,-1.74712655331056,-1.70292711374082,-1.28137423833786,
-0.996111179633715,-0.765912925479485,-0.547442578207348,-0.286906424613266,
-0.136326843594045,-0.0501381164492935),.UNSPECIFIED.);
#3781=B_SPLINE_CURVE_WITH_KNOTS('',3,(#25883,#25884,#25885,#25886,#25887,
#25888),.UNSPECIFIED.,.F.,.F.,(4,2,4),(-0.993618385713603,-0.861681629743274,
-0.625529516371081),.UNSPECIFIED.);
#3782=B_SPLINE_CURVE_WITH_KNOTS('',3,(#25890,#25891,#25892,#25893,#25894,
#25895,#25896,#25897,#25898,#25899,#25900,#25901,#25902,#25903,#25904,#25905,
#25906,#25907,#25908,#25909,#25910,#25911,#25912,#25913,#25914,#25915,#25916,
#25917,#25918,#25919,#25920,#25921,#25922,#25923,#25924,#25925,#25926,#25927,
#25928,#25929,#25930,#25931,#25932,#25933,#25934,#25935,#25936,#25937,#25938,
#25939,#25940,#25941,#25942,#25943,#25944,#25945,#25946,#25947,#25948,#25949,
#25950,#25951,#25952,#25953,#25954,#25955,#25956),.UNSPECIFIED.,.F.,.F.,
(4,3,3,3,3,3,3,3,3,3,3,3,3,3,3,3,3,3,3,3,3,3,4),(-7.28045043064328,-7.10146924914703,
-5.58665127040606,-5.35053852365389,-5.18292571310771,-4.93518995685649,
-4.59847254595278,-4.20592684595026,-3.66025783517109,-3.16635853444291,
-2.76138423978034,-2.31987517731217,-2.01230406713492,-1.72292916433732,
-1.60295645908227,-1.18526991655821,-0.932600063388904,-0.806265136804252,
-0.72098039430321,-0.679930210219599,-0.615963294348663,-0.16431223133682,
0.),.UNSPECIFIED.);
#3783=B_SPLINE_CURVE_WITH_KNOTS('',3,(#25960,#25961,#25962,#25963),
 .UNSPECIFIED.,.F.,.F.,(4,4),(-0.123320533354419,0.),.UNSPECIFIED.);
#3784=B_SPLINE_CURVE_WITH_KNOTS('',3,(#25965,#25966,#25967,#25968),
 .UNSPECIFIED.,.F.,.F.,(4,4),(-1.0626156692464,-0.306410932880038),
 .UNSPECIFIED.);
#3785=B_SPLINE_CURVE_WITH_KNOTS('',3,(#25970,#25971,#25972,#25973),
 .UNSPECIFIED.,.F.,.F.,(4,4),(-0.123345114071741,0.),.UNSPECIFIED.);
#3786=B_SPLINE_CURVE_WITH_KNOTS('',3,(#25977,#25978,#25979,#25980,#25981,
#25982,#25983,#25984,#25985,#25986,#25987,#25988,#25989,#25990,#25991,#25992,
#25993,#25994,#25995,#25996,#25997,#25998,#25999,#26000,#26001,#26002,#26003,
#26004,#26005,#26006,#26007,#26008,#26009,#26010,#26011,#26012,#26013,#26014,
#26015,#26016,#26017,#26018,#26019,#26020,#26021,#26022,#26023,#26024,#26025,
#26026,#26027,#26028,#26029,#26030,#26031,#26032,#26033,#26034,#26035,#26036,
#26037,#26038,#26039,#26040,#26041,#26042,#26043,#26044,#26045,#26046,#26047,
#26048,#26049),.UNSPECIFIED.,.F.,.F.,(4,3,3,3,3,3,3,3,3,3,3,3,3,3,3,3,3,
3,3,3,3,3,3,3,4),(-12.8459374931962,-11.4794095622303,-10.7961455967474,
-10.3238102725535,-10.1128816312645,-9.79002513704445,-7.17546445119587,
-5.86818410827158,-5.21454393680944,-4.88772385107836,-4.68535987603764,
-4.56090376534729,-4.42075803988792,-3.4847448924849,-2.76035534391094,
-2.17493233266957,-1.74712655334424,-1.70292711374143,-1.28137423833914,
-0.996111179634701,-0.765912925480124,-0.54744257820773,-0.286906424613362,
-0.136326843594467,-0.0501381164492885),.UNSPECIFIED.);
#3787=B_SPLINE_CURVE_WITH_KNOTS('',3,(#26051,#26052,#26053,#26054,#26055,
#26056),.UNSPECIFIED.,.F.,.F.,(4,2,4),(-0.562962425256162,-0.401675631762059,
-0.194993927866297),.UNSPECIFIED.);
#3788=B_SPLINE_CURVE_WITH_KNOTS('',3,(#26058,#26059,#26060,#26061,#26062,
#26063,#26064,#26065,#26066,#26067,#26068,#26069,#26070,#26071,#26072,#26073,
#26074,#26075,#26076,#26077,#26078,#26079,#26080,#26081,#26082,#26083,#26084,
#26085,#26086,#26087,#26088,#26089,#26090,#26091,#26092,#26093,#26094,#26095,
#26096,#26097,#26098,#26099,#26100,#26101,#26102,#26103,#26104,#26105,#26106,
#26107,#26108,#26109,#26110,#26111,#26112,#26113,#26114,#26115,#26116,#26117,
#26118,#26119,#26120,#26121,#26122,#26123,#26124),.UNSPECIFIED.,.F.,.F.,
(4,3,3,3,3,3,3,3,3,3,3,3,3,3,3,3,3,3,3,3,3,3,4),(-7.28045043029337,-7.10146924879316,
-5.58665127003706,-5.35053852328322,-5.18292571277321,-4.93518995652797,
-4.59847254563688,-4.20592684564096,-3.66025783487647,-3.16635853414848,
-2.76138423958633,-2.31987517717087,-2.01230406703615,-1.72292916424559,
-1.60295645899705,-1.18526991650819,-0.932600063361394,-0.806265136787995,
-0.720980394298989,-0.679930210214595,-0.615963294349437,-0.164312231356818,
0.),.UNSPECIFIED.);
#3789=B_SPLINE_CURVE_WITH_KNOTS('',3,(#26128,#26129,#26130,#26131),
 .UNSPECIFIED.,.F.,.F.,(4,4),(-0.123320533354417,0.),.UNSPECIFIED.);
#3790=B_SPLINE_CURVE_WITH_KNOTS('',3,(#26133,#26134,#26135,#26136,#26137,
#26138),.UNSPECIFIED.,.F.,.F.,(4,2,4),(-1.35394250197628,-0.852961572903345,
-0.599740178024189),.UNSPECIFIED.);
#3791=B_SPLINE_CURVE_WITH_KNOTS('',3,(#26140,#26141,#26142,#26143),
 .UNSPECIFIED.,.F.,.F.,(4,4),(-0.123345114071735,0.),.UNSPECIFIED.);
#3792=B_SPLINE_CURVE_WITH_KNOTS('',3,(#26147,#26148,#26149,#26150,#26151,
#26152,#26153,#26154,#26155,#26156,#26157,#26158,#26159,#26160,#26161,#26162,
#26163,#26164,#26165,#26166,#26167,#26168,#26169,#26170,#26171,#26172,#26173,
#26174,#26175,#26176,#26177,#26178,#26179,#26180,#26181,#26182,#26183,#26184,
#26185,#26186,#26187,#26188,#26189,#26190,#26191,#26192,#26193,#26194,#26195,
#26196,#26197,#26198,#26199,#26200,#26201,#26202,#26203,#26204,#26205,#26206,
#26207,#26208,#26209,#26210,#26211,#26212,#26213,#26214,#26215,#26216,#26217,
#26218,#26219),.UNSPECIFIED.,.F.,.F.,(4,3,3,3,3,3,3,3,3,3,3,3,3,3,3,3,3,
3,3,3,3,3,3,3,4),(-12.8459375085894,-11.4794095748003,-10.7961456079058,
-10.3238102827373,-10.1128816410112,-9.79002514616695,-7.17546445577377,
-5.86818411057718,-5.21454393797889,-4.88772385167974,-4.68535987651592,
-4.56090376538059,-4.42075803995975,-3.4847448925491,-2.76035534390967,
-2.17493233266947,-1.7471265533345,-1.70292711373975,-1.28137423833773,
-0.996111179633625,-0.765912925479341,-0.547442578207242,-0.286906424613248,
-0.13632684359387,-0.0501381164492966),.UNSPECIFIED.);
#3793=B_SPLINE_CURVE_WITH_KNOTS('',3,(#26221,#26222,#26223,#26224,#26225,
#26226),.UNSPECIFIED.,.F.,.F.,(4,2,4),(-0.59625459278609,-0.430840814871637,
-0.228304293786418),.UNSPECIFIED.);
#3794=B_SPLINE_CURVE_WITH_KNOTS('',3,(#26228,#26229,#26230,#26231,#26232,
#26233,#26234,#26235,#26236,#26237,#26238,#26239,#26240,#26241,#26242,#26243,
#26244,#26245,#26246,#26247,#26248,#26249,#26250,#26251,#26252,#26253,#26254,
#26255,#26256,#26257,#26258,#26259,#26260,#26261,#26262,#26263,#26264,#26265,
#26266,#26267,#26268,#26269,#26270,#26271,#26272,#26273,#26274,#26275,#26276,
#26277,#26278,#26279,#26280,#26281,#26282,#26283,#26284,#26285,#26286,#26287,
#26288,#26289,#26290,#26291,#26292,#26293,#26294),.UNSPECIFIED.,.F.,.F.,
(4,3,3,3,3,3,3,3,3,3,3,3,3,3,3,3,3,3,3,3,3,3,4),(-7.2804504305595,-7.10146924906192,
-5.58665127031306,-5.35053852355854,-5.18292571301866,-4.93518995676791,
-4.59847254586487,-4.20592684586167,-3.6602578350825,-3.16635853435267,
-2.76138423970751,-2.31987517726742,-2.01229466833062,-1.72292721738687,
-1.60295645904427,-1.18526991653728,-0.932600063377868,-0.806265136798164,
-0.720980394308923,-0.679930210218459,-0.615963294355597,-0.164312231353533,
0.),.UNSPECIFIED.);
#3795=B_SPLINE_CURVE_WITH_KNOTS('',3,(#26298,#26299,#26300,#26301),
 .UNSPECIFIED.,.F.,.F.,(4,4),(-0.123320533354386,0.),.UNSPECIFIED.);
#3796=B_SPLINE_CURVE_WITH_KNOTS('',3,(#26303,#26304,#26305,#26306,#26307,
#26308),.UNSPECIFIED.,.F.,.F.,(4,2,4),(-1.20932024771483,-0.985380063173395,
-0.454839283541961),.UNSPECIFIED.);
#3797=B_SPLINE_CURVE_WITH_KNOTS('',3,(#26310,#26311,#26312,#26313),
 .UNSPECIFIED.,.F.,.F.,(4,4),(-0.12334511407169,0.),.UNSPECIFIED.);
#3798=B_SPLINE_CURVE_WITH_KNOTS('',3,(#26317,#26318,#26319,#26320,#26321,
#26322,#26323,#26324,#26325,#26326,#26327,#26328,#26329,#26330,#26331,#26332,
#26333,#26334,#26335,#26336,#26337,#26338,#26339,#26340,#26341,#26342,#26343,
#26344,#26345,#26346,#26347,#26348,#26349,#26350,#26351,#26352,#26353,#26354,
#26355,#26356,#26357,#26358,#26359,#26360,#26361,#26362,#26363,#26364,#26365,
#26366,#26367,#26368,#26369,#26370,#26371,#26372,#26373,#26374,#26375,#26376,
#26377,#26378,#26379,#26380,#26381,#26382,#26383,#26384,#26385,#26386,#26387,
#26388,#26389),.UNSPECIFIED.,.F.,.F.,(4,3,3,3,3,3,3,3,3,3,3,3,3,3,3,3,3,
3,3,3,3,3,3,3,4),(-12.8459374789857,-11.4794095507986,-10.796145586705,
-10.3238102635133,-10.1128816226115,-9.79002512908185,-7.17546444721137,
-5.86818410627612,-5.2145439358085,-4.88772385057469,-4.68535987579906,
-4.56090376534088,-4.42075803995232,-3.48474489272658,-2.76035534392023,
-2.17493233268704,-1.74712655326145,-1.70292711374347,-1.28137423833848,
-0.996111179633947,-0.765912925479577,-0.547442578207388,-0.286906424613283,
-0.136326843593936,-0.0501381164492949),.UNSPECIFIED.);
#3799=B_SPLINE_CURVE_WITH_KNOTS('',3,(#26391,#26392,#26393,#26394,#26395,
#26396),.UNSPECIFIED.,.F.,.F.,(4,2,4),(-0.993618385713603,-0.861681629743273,
-0.625529516371081),.UNSPECIFIED.);
#3800=B_SPLINE_CURVE_WITH_KNOTS('',3,(#26398,#26399,#26400,#26401,#26402,
#26403,#26404,#26405,#26406,#26407,#26408,#26409,#26410,#26411,#26412,#26413,
#26414,#26415,#26416,#26417,#26418,#26419,#26420,#26421,#26422,#26423,#26424,
#26425,#26426,#26427,#26428,#26429,#26430,#26431,#26432,#26433,#26434,#26435,
#26436,#26437,#26438,#26439,#26440,#26441,#26442,#26443,#26444,#26445,#26446,
#26447,#26448,#26449,#26450,#26451,#26452,#26453,#26454,#26455,#26456,#26457,
#26458,#26459,#26460,#26461,#26462,#26463,#26464),.UNSPECIFIED.,.F.,.F.,
(4,3,3,3,3,3,3,3,3,3,3,3,3,3,3,3,3,3,3,3,3,3,4),(-7.28045043097374,-7.10146924946984,
-5.58665127066262,-5.3505385238982,-5.18292571334222,-4.9351899570797,-4.5984725461592,
-4.20592684613719,-3.66025783532649,-3.1663585345898,-2.76138423986509,
-2.3198751773955,-2.01230406722963,-1.72292916437289,-1.60295645910747,
-1.18526991657213,-0.932600063393711,-0.806265136804503,-0.720980394315423,
-0.679930210215295,-0.615963294358323,-0.164312231362043,0.),
 .UNSPECIFIED.);
#3801=B_SPLINE_CURVE_WITH_KNOTS('',3,(#26468,#26469,#26470,#26471),
 .UNSPECIFIED.,.F.,.F.,(4,4),(-0.123320533354413,0.),.UNSPECIFIED.);
#3802=B_SPLINE_CURVE_WITH_KNOTS('',3,(#26473,#26474,#26475,#26476),
 .UNSPECIFIED.,.F.,.F.,(4,4),(-1.0626156692464,-0.306410932880038),
 .UNSPECIFIED.);
#3803=B_SPLINE_CURVE_WITH_KNOTS('',3,(#26478,#26479,#26480,#26481),
 .UNSPECIFIED.,.F.,.F.,(4,4),(-0.123345114071708,0.),.UNSPECIFIED.);
#3804=B_SPLINE_CURVE_WITH_KNOTS('',3,(#26485,#26486,#26487,#26488,#26489,
#26490,#26491,#26492,#26493,#26494,#26495,#26496,#26497,#26498,#26499,#26500,
#26501,#26502,#26503,#26504,#26505,#26506,#26507,#26508,#26509,#26510,#26511,
#26512,#26513,#26514,#26515,#26516,#26517,#26518,#26519,#26520,#26521,#26522,
#26523,#26524,#26525,#26526,#26527,#26528,#26529,#26530,#26531,#26532,#26533,
#26534,#26535,#26536,#26537,#26538,#26539,#26540,#26541,#26542,#26543,#26544,
#26545,#26546,#26547,#26548,#26549,#26550,#26551,#26552,#26553,#26554,#26555,
#26556,#26557),.UNSPECIFIED.,.F.,.F.,(4,3,3,3,3,3,3,3,3,3,3,3,3,3,3,3,3,
3,3,3,3,3,3,3,4),(-12.8459374978601,-11.4794095665157,-10.7961456008435,
-10.3238102765321,-10.1128816351713,-9.79002514084029,-7.17546445308554,
-5.86818410920817,-5.21454393726949,-4.88772385130015,-4.68535987641399,
-4.5609037653308,-4.42075804013772,-3.48474489292319,-2.76035534391119,
-2.1749323326717,-1.74712655332877,-1.70292711374094,-1.28137423833841,
-0.996111179634097,-0.765912925479675,-0.547442578207446,-0.286906424613297,
-0.13632684359409,-0.050138116449294),.UNSPECIFIED.);
#3805=B_SPLINE_CURVE_WITH_KNOTS('',3,(#26559,#26560,#26561,#26562,#26563,
#26564),.UNSPECIFIED.,.F.,.F.,(4,2,4),(-0.562962425256162,-0.401675631762059,
-0.194993927866297),.UNSPECIFIED.);
#3806=B_SPLINE_CURVE_WITH_KNOTS('',3,(#26565,#26566,#26567,#26568,#26569,
#26570,#26571,#26572,#26573,#26574,#26575,#26576,#26577,#26578,#26579,#26580,
#26581,#26582,#26583,#26584,#26585,#26586,#26587,#26588,#26589),
 .UNSPECIFIED.,.F.,.F.,(4,3,3,3,3,3,3,3,4),(-7.28045042871898,-7.10146924723026,
-5.58665126861639,-5.35053852188943,-5.18292571148688,-4.93518995528529,
-4.59847254446614,-4.20592684453517,-4.02394626436512),.UNSPECIFIED.);
#3807=B_SPLINE_CURVE_WITH_KNOTS('',3,(#26595,#26596,#26597,#26598,#26599,
#26600),.UNSPECIFIED.,.F.,.F.,(4,1,1,4),(109.955742875643,110.793237955343,
111.785020006418,112.692634884417),.UNSPECIFIED.);
#3808=B_SPLINE_CURVE_WITH_KNOTS('',3,(#26603,#26604,#26605,#26606,#26607),
 .UNSPECIFIED.,.F.,.F.,(4,1,4),(109.955742875643,110.461935712833,111.453717763908),
 .UNSPECIFIED.);
#3809=B_SPLINE_CURVE_WITH_KNOTS('',3,(#26612,#26613,#26614,#26615,#26616,
#26617,#26618,#26619,#26620,#26621,#26622),.UNSPECIFIED.,.F.,.F.,(4,1,1,
1,1,1,1,1,4),(103.672557568463,103.850763597816,104.842545648891,105.834327699966,
106.826109751042,107.817891802117,108.809673853192,109.801455904267,109.955742875643),
 .UNSPECIFIED.);
#3810=B_SPLINE_CURVE_WITH_KNOTS('',3,(#26623,#26624,#26625,#26626,#26627,
#26628,#26629,#26630,#26631,#26632),.UNSPECIFIED.,.F.,.F.,(4,1,1,1,1,1,
1,4),(103.672557568463,104.511243406382,105.503025457457,106.494807508532,
107.486589559607,108.478371610683,109.470153661758,109.955742875643),
 .UNSPECIFIED.);
#3811=B_SPLINE_CURVE_WITH_KNOTS('',3,(#26637,#26638,#26639,#26640,#26641,
#26642,#26643,#26644,#26645,#26646),.UNSPECIFIED.,.F.,.F.,(4,1,1,1,1,1,
1,4),(97.3893722612835,97.9000712913645,98.8918533424397,99.883635393515,
100.87541744459,101.867199495665,102.858981546741,103.672557568463),
 .UNSPECIFIED.);
#3812=B_SPLINE_CURVE_WITH_KNOTS('',3,(#26647,#26648,#26649,#26650,#26651,
#26652,#26653,#26654,#26655,#26656,#26657),.UNSPECIFIED.,.F.,.F.,(4,1,1,
1,1,1,1,1,4),(97.3893722612835,97.568769048855,98.5605510999303,99.5523331510055,
100.544115202081,101.535897253156,102.527679304231,103.519461355306,103.672557568463),
 .UNSPECIFIED.);
#3813=B_SPLINE_CURVE_WITH_KNOTS('',3,(#26662,#26663,#26664,#26665,#26666,
#26667,#26668,#26669,#26670,#26671),.UNSPECIFIED.,.F.,.F.,(4,1,1,1,1,1,
1,4),(91.106186954104,91.949378984913,92.9411610359883,93.9329430870635,
94.9247251381387,95.916507189214,96.9082892402892,97.3893722612835),
 .UNSPECIFIED.);
#3814=B_SPLINE_CURVE_WITH_KNOTS('',3,(#26672,#26673,#26674,#26675,#26676,
#26677,#26678,#26679,#26680,#26681),.UNSPECIFIED.,.F.,.F.,(4,1,1,1,1,1,
1,4),(91.106186954104,91.6180767424036,92.6098587934788,93.601640844554,
94.5934228956293,95.5852049467045,96.5769869977798,97.3893722612835),
 .UNSPECIFIED.);
#3815=B_SPLINE_CURVE_WITH_KNOTS('',3,(#26686,#26687,#26688,#26689,#26690,
#26691,#26692,#26693,#26694,#26695,#26696),.UNSPECIFIED.,.F.,.F.,(4,1,1,
1,1,1,1,1,4),(84.8230016469244,85.0069046273863,85.9986866784616,86.9904687295368,
87.9822507806121,88.9740328316873,89.9658148827625,90.9575969338378,91.106186954104),
 .UNSPECIFIED.);
#3816=B_SPLINE_CURVE_WITH_KNOTS('',3,(#26697,#26698,#26699,#26700,#26701,
#26702,#26703,#26704,#26705,#26706),.UNSPECIFIED.,.F.,.F.,(4,1,1,1,1,1,
1,4),(84.8230016469244,85.6673844359521,86.6591664870274,87.6509485381026,
88.6427305891778,89.6345126402531,90.6262946913283,91.106186954104),
 .UNSPECIFIED.);
#3817=B_SPLINE_CURVE_WITH_KNOTS('',3,(#26711,#26712,#26713,#26714,#26715,
#26716,#26717,#26718,#26719,#26720),.UNSPECIFIED.,.F.,.F.,(4,1,1,1,1,1,
1,4),(78.5398163397447,79.0562123209349,80.0479943720101,81.0397764230854,
82.0315584741606,83.0233405252359,84.0151225763111,84.8230016469244),
 .UNSPECIFIED.);
#3818=B_SPLINE_CURVE_WITH_KNOTS('',3,(#26721,#26722,#26723,#26724,#26725,
#26726,#26727,#26728,#26729,#26730,#26731),.UNSPECIFIED.,.F.,.F.,(4,1,1,
1,1,1,1,1,4),(78.5398163397447,78.7249100784254,79.7166921295007,80.7084741805759,
81.7002562316512,82.6920382827264,83.6838203338016,84.6756023848769,84.8230016469244),
 .UNSPECIFIED.);
#3819=B_SPLINE_CURVE_WITH_KNOTS('',3,(#26736,#26737,#26738,#26739,#26740,
#26741,#26742,#26743,#26744,#26745),.UNSPECIFIED.,.F.,.F.,(4,1,1,1,1,1,
1,4),(72.2566310325653,73.1055200144834,74.0973020655587,75.0890841166339,
76.0808661677092,77.0726482187844,78.0644302698597,78.5398163397447),
 .UNSPECIFIED.);
#3820=B_SPLINE_CURVE_WITH_KNOTS('',3,(#26746,#26747,#26748,#26749,#26750,
#26751,#26752,#26753,#26754,#26755),.UNSPECIFIED.,.F.,.F.,(4,1,1,1,1,1,
1,4),(72.2566310325653,72.774217771974,73.7659998230492,74.7577818741245,
75.7495639251997,76.741345976275,77.7331280273502,78.5398163397447),
 .UNSPECIFIED.);
#3821=B_SPLINE_CURVE_WITH_KNOTS('',3,(#26760,#26761,#26762,#26763,#26764,
#26765,#26766,#26767,#26768,#26769,#26770),.UNSPECIFIED.,.F.,.F.,(4,1,1,
1,1,1,1,1,4),(65.9734457253856,66.1630456569568,67.154827708032,68.1466097591072,
69.1383918101825,70.1301738612577,71.121955912333,72.1137379634082,72.2566310325653),
 .UNSPECIFIED.);
#3822=B_SPLINE_CURVE_WITH_KNOTS('',3,(#26771,#26772,#26773,#26774,#26775,
#26776,#26777,#26778,#26779,#26780),.UNSPECIFIED.,.F.,.F.,(4,1,1,1,1,1,
1,4),(65.9734457253856,66.8235254655226,67.8153075165978,68.807089567673,
69.7988716187483,70.7906536698235,71.7824357208987,72.2566310325653),
 .UNSPECIFIED.);
#3823=B_SPLINE_CURVE_WITH_KNOTS('',3,(#26785,#26786,#26787,#26788,#26789,
#26790,#26791,#26792,#26793,#26794),.UNSPECIFIED.,.F.,.F.,(4,1,1,1,1,1,
1,4),(59.6902604182061,60.2123533505053,61.2041354015806,62.1959174526558,
63.187699503731,64.1794815548063,65.1712636058815,65.9734457253856),
 .UNSPECIFIED.);
#3824=B_SPLINE_CURVE_WITH_KNOTS('',3,(#26795,#26796,#26797,#26798,#26799,
#26800,#26801,#26802,#26803,#26804,#26805),.UNSPECIFIED.,.F.,.F.,(4,1,1,
1,1,1,1,1,4),(59.6902604182059,59.8810511079959,60.8728331590711,61.8646152101463,
62.8563972612216,63.8481793122968,64.8399613633721,65.8317434144473,65.9734457253856),
 .UNSPECIFIED.);
#3825=B_SPLINE_CURVE_WITH_KNOTS('',3,(#26810,#26811,#26812,#26813,#26814,
#26815,#26816,#26817,#26818,#26819),.UNSPECIFIED.,.F.,.F.,(4,1,1,1,1,1,
1,4),(53.4070751110265,54.2616610440539,55.2534430951291,56.2452251462044,
57.2370071972796,58.2287892483548,59.2205712994301,59.6902604182061),
 .UNSPECIFIED.);
#3826=B_SPLINE_CURVE_WITH_KNOTS('',3,(#26820,#26821,#26822,#26823,#26824,
#26825,#26826,#26827,#26828,#26829),.UNSPECIFIED.,.F.,.F.,(4,1,1,1,1,1,
1,4),(53.4070751110265,53.9303588015444,54.9221408526197,55.9139229036949,
56.9057049547701,57.8974870058454,58.8892690569206,59.6902604182059),
 .UNSPECIFIED.);
#3827=B_SPLINE_CURVE_WITH_KNOTS('',3,(#26834,#26835,#26836,#26837,#26838,
#26839,#26840,#26841,#26842,#26843,#26844),.UNSPECIFIED.,.F.,.F.,(4,1,1,
1,1,1,1,1,4),(47.1238898038468,47.3191866865272,48.3109687376024,49.3027507886777,
50.2945328397529,51.2863148908282,52.2780969419034,53.2698789929786,53.4070751110265),
 .UNSPECIFIED.);
#3828=B_SPLINE_CURVE_WITH_KNOTS('',3,(#26845,#26846,#26847,#26848,#26849,
#26850,#26851,#26852,#26853,#26854),.UNSPECIFIED.,.F.,.F.,(4,1,1,1,1,1,
1,4),(47.1238898038468,47.979666495093,48.9714485461682,49.9632305972435,
50.9550126483187,51.9467946993939,52.9385767504692,53.4070751110265),
 .UNSPECIFIED.);
#3829=B_SPLINE_CURVE_WITH_KNOTS('',3,(#26859,#26860,#26861,#26862,#26863,
#26864,#26865,#26866,#26867,#26868),.UNSPECIFIED.,.F.,.F.,(4,1,1,1,1,1,
1,4),(40.8407044966673,41.3684943800758,42.360276431151,43.3520584822262,
44.3438405333015,45.3356225843767,46.327404635452,47.1238898038468),
 .UNSPECIFIED.);
#3830=B_SPLINE_CURVE_WITH_KNOTS('',3,(#26869,#26870,#26871,#26872,#26873,
#26874,#26875,#26876,#26877,#26878,#26879),.UNSPECIFIED.,.F.,.F.,(4,1,1,
1,1,1,1,1,4),(40.8407044966673,41.0371921375663,42.0289741886415,43.0207562397168,
44.012538290792,45.0043203418673,45.9961023929425,46.9878844440177,47.1238898038468),
 .UNSPECIFIED.);
#3831=B_SPLINE_CURVE_WITH_KNOTS('',3,(#26884,#26885,#26886,#26887,#26888,
#26889,#26890,#26891,#26892,#26893),.UNSPECIFIED.,.F.,.F.,(4,1,1,1,1,1,
1,4),(34.5575191894877,35.4178020736243,36.4095841246995,37.4013661757748,
38.39314822685,39.3849302779253,40.3767123290005,40.8407044966673),
 .UNSPECIFIED.);
#3832=B_SPLINE_CURVE_WITH_KNOTS('',3,(#26894,#26895,#26896,#26897,#26898,
#26899,#26900,#26901,#26902,#26903),.UNSPECIFIED.,.F.,.F.,(4,1,1,1,1,1,
1,4),(34.5575191894877,35.0864998311148,36.0782818821901,37.0700639332653,
38.0618459843406,39.0536280354158,40.0454100864911,40.8407044966673),
 .UNSPECIFIED.);
#3833=B_SPLINE_CURVE_WITH_KNOTS('',3,(#26908,#26909,#26910,#26911,#26912,
#26913,#26914,#26915,#26916,#26917,#26918),.UNSPECIFIED.,.F.,.F.,(4,1,1,
1,1,1,1,1,4),(28.2743338823081,28.4753277160976,29.4671097671729,30.4588918182481,
31.4506738693233,32.4424559203986,33.4342379714738,34.4260200225491,34.5575191894877),
 .UNSPECIFIED.);
#3834=B_SPLINE_CURVE_WITH_KNOTS('',3,(#26919,#26920,#26921,#26922,#26923,
#26924,#26925,#26926,#26927,#26928),.UNSPECIFIED.,.F.,.F.,(4,1,1,1,1,1,
1,4),(28.2743338823081,29.1358075246634,30.1275895757386,31.1193716268139,
32.1111536778891,33.1029357289644,34.0947177800396,34.5575191894877),
 .UNSPECIFIED.);
#3835=B_SPLINE_CURVE_WITH_KNOTS('',3,(#26933,#26934,#26935,#26936,#26937,
#26938,#26939,#26940,#26941,#26942),.UNSPECIFIED.,.F.,.F.,(4,1,1,1,1,1,
1,4),(21.9911485751285,22.5246354096462,23.5164174607214,24.5081995117967,
25.4999815628719,26.4917636139471,27.4835456650224,28.2743338823081),
 .UNSPECIFIED.);
#3836=B_SPLINE_CURVE_WITH_KNOTS('',3,(#26943,#26944,#26945,#26946,#26947,
#26948,#26949,#26950,#26951,#26952,#26953),.UNSPECIFIED.,.F.,.F.,(4,1,1,
1,1,1,1,1,4),(21.9911485751284,22.1933331671367,23.185115218212,24.1768972692872,
25.1686793203624,26.1604613714377,27.1522434225129,28.1440254735882,28.2743338823081),
 .UNSPECIFIED.);
#3837=B_SPLINE_CURVE_WITH_KNOTS('',3,(#26958,#26959,#26960,#26961,#26962,
#26963,#26964,#26965,#26966,#26967),.UNSPECIFIED.,.F.,.F.,(4,1,1,1,1,1,
1,4),(15.7079632679489,16.5739431031947,17.56572515427,18.5575072053452,
19.5492892564205,20.5410713074957,21.5328533585709,21.9911485751285),
 .UNSPECIFIED.);
#3838=B_SPLINE_CURVE_WITH_KNOTS('',3,(#26968,#26969,#26970,#26971,#26972,
#26973,#26974,#26975,#26976,#26977),.UNSPECIFIED.,.F.,.F.,(4,1,1,1,1,1,
1,4),(15.7079632679489,16.2426408606853,17.2344229117605,18.2262049628358,
19.217987013911,20.2097690649862,21.2015511160615,21.9911485751284),
 .UNSPECIFIED.);
#3839=B_SPLINE_CURVE_WITH_KNOTS('',3,(#27305,#27306,#27307,#27308),
 .UNSPECIFIED.,.F.,.F.,(4,4),(-0.0707400283740946,0.),.UNSPECIFIED.);
#3840=B_SPLINE_CURVE_WITH_KNOTS('',3,(#27312,#27313,#27314,#27315),
 .UNSPECIFIED.,.F.,.F.,(4,4),(-0.070743295445964,-3.34525766250426E-6),
 .UNSPECIFIED.);
#3841=B_SPLINE_CURVE_WITH_KNOTS('',3,(#27319,#27320,#27321,#27322,#27323,
#27324,#27325,#27326,#27327,#27328,#27329,#27330,#27331,#27332,#27333,#27334,
#27335,#27336,#27337,#27338,#27339,#27340,#27341,#27342,#27343,#27344,#27345,
#27346,#27347,#27348,#27349,#27350,#27351,#27352,#27353,#27354,#27355,#27356,
#27357,#27358,#27359,#27360,#27361,#27362,#27363,#27364,#27365,#27366,#27367,
#27368,#27369,#27370,#27371,#27372,#27373,#27374,#27375,#27376,#27377,#27378,
#27379,#27380,#27381,#27382,#27383,#27384,#27385,#27386,#27387,#27388,#27389,
#27390,#27391,#27392,#27393,#27394,#27395,#27396,#27397,#27398,#27399,#27400,
#27401,#27402,#27403,#27404,#27405,#27406,#27407,#27408,#27409,#27410,#27411,
#27412,#27413,#27414,#27415),.UNSPECIFIED.,.F.,.F.,(4,3,3,3,3,3,3,3,3,3,
3,3,3,3,3,3,3,3,3,3,3,3,3,3,3,3,3,3,3,3,3,3,4),(-0.461463988274541,-0.386087506167661,
-0.375299929924104,-0.372903671306323,-0.356077696752448,-0.352040116130794,
-0.339920267375323,-0.338448280177947,-0.326632246672126,-0.313204943761465,
-0.304885949019545,-0.29982124014814,-0.293952204614803,-0.287658393406508,
-0.282882239837598,-0.277507204165034,-0.271689255077659,-0.265572046854325,
-0.25886897335232,-0.254459737762025,-0.241918019250842,-0.227822266677633,
-0.212603244487136,-0.196183063900822,-0.178197554741815,-0.159751102176233,
-0.141758270371077,-0.134249918117004,-0.101233605562941,-0.0682193757072185,
-0.0525746845214139,-0.0245175806023845,0.),.UNSPECIFIED.);
#3842=B_SPLINE_CURVE_WITH_KNOTS('',3,(#27418,#27419,#27420,#27421,#27422,
#27423,#27424,#27425,#27426,#27427,#27428,#27429,#27430,#27431,#27432,#27433,
#27434,#27435,#27436,#27437,#27438,#27439,#27440,#27441,#27442,#27443,#27444,
#27445,#27446,#27447,#27448,#27449,#27450,#27451,#27452,#27453,#27454,#27455,
#27456,#27457,#27458,#27459,#27460,#27461,#27462,#27463,#27464,#27465,#27466,
#27467,#27468,#27469,#27470,#27471,#27472,#27473,#27474,#27475,#27476,#27477,
#27478,#27479,#27480,#27481),.UNSPECIFIED.,.F.,.F.,(4,3,3,3,3,3,3,3,3,3,
3,3,3,3,3,3,3,3,3,3,3,4),(-0.976443208995993,-0.95964177146371,-0.949661288965092,
-0.932500795758735,-0.914975318862148,-0.904644103415597,-0.893689140152817,
-0.881835075865292,-0.868593367676957,-0.854447019507673,-0.839440732702782,
-0.82369847533003,-0.808085046250858,-0.793464970995011,-0.790720555879271,
-0.779060485592236,-0.740625,-0.691250000000001,-0.5925,-0.543125,-0.395,
-0.049999999999998),.UNSPECIFIED.);
#3843=B_SPLINE_CURVE_WITH_KNOTS('',3,(#27693,#27694,#27695,#27696),
 .UNSPECIFIED.,.F.,.F.,(4,4),(-0.253410853624616,-0.103262412077185),
 .UNSPECIFIED.);
#3844=B_SPLINE_CURVE_WITH_KNOTS('',3,(#27698,#27699,#27700,#27701),
 .UNSPECIFIED.,.F.,.F.,(4,4),(0.,0.29),.UNSPECIFIED.);
#3845=B_SPLINE_CURVE_WITH_KNOTS('',3,(#27703,#27704,#27705,#27706),
 .UNSPECIFIED.,.F.,.F.,(4,4),(3.28350553677514,3.37607250270485),
 .UNSPECIFIED.);
#3846=B_SPLINE_CURVE_WITH_KNOTS('',3,(#27707,#27708,#27709,#27710,#27711,
#27712,#27713,#27714,#27715,#27716,#27717,#27718,#27719,#27720,#27721,#27722,
#27723,#27724,#27725,#27726,#27727,#27728,#27729,#27730,#27731,#27732,#27733,
#27734,#27735,#27736,#27737,#27738,#27739,#27740,#27741,#27742,#27743,#27744,
#27745,#27746,#27747,#27748,#27749,#27750,#27751,#27752),.UNSPECIFIED.,
 .F.,.F.,(4,3,3,3,3,3,3,3,3,3,3,3,3,3,3,4),(-4.02394626436512,-3.66025783388072,
-3.16634870316095,-2.76138423897494,-2.31987517666077,-2.01230406657675,
-1.72292916396621,-1.60295645875968,-1.18526991637693,-0.932600063295131,
-0.806265136754233,-0.720980394265897,-0.679930210213335,-0.615963294332911,
-0.164312231367537,0.),.UNSPECIFIED.);
#3847=B_SPLINE_CURVE_WITH_KNOTS('',3,(#27754,#27755,#27756,#27757,#27758,
#27759),.UNSPECIFIED.,.F.,.F.,(4,2,4),(-2.17700203273975,-1.38478587807843,
-0.288632999074765),.UNSPECIFIED.);
#3848=B_SPLINE_CURVE_WITH_KNOTS('',3,(#27761,#27762,#27763,#27764,#27765,
#27766,#27767,#27768,#27769,#27770,#27771,#27772,#27773,#27774,#27775,#27776,
#27777,#27778,#27779,#27780,#27781,#27782,#27783,#27784,#27785,#27786,#27787,
#27788,#27789,#27790,#27791),.UNSPECIFIED.,.F.,.F.,(4,3,3,3,3,3,3,3,3,3,
4),(0.664704897780732,0.688351938092992,0.78031723869645,0.810486879810963,
0.862717972416633,0.955520663501275,1.01466394039964,1.06038302616807,1.10529572457683,
1.13272802062135,1.20216888729732),.UNSPECIFIED.);
#3849=B_SPLINE_CURVE_WITH_KNOTS('',3,(#27792,#27793,#27794,#27795,#27796,
#27797,#27798,#27799,#27800,#27801,#27802,#27803,#27804,#27805,#27806,#27807,
#27808,#27809,#27810),.UNSPECIFIED.,.F.,.F.,(4,3,3,3,3,3,4),(0.,0.178790961538472,
0.350742859481108,0.449205432353047,0.513879914408645,0.522694757423744,
0.664704897780732),.UNSPECIFIED.);
#3850=B_SPLINE_CURVE_WITH_KNOTS('',3,(#27814,#27815,#27816,#27817),
 .UNSPECIFIED.,.F.,.F.,(4,4),(-0.0707400282910659,0.),.UNSPECIFIED.);
#3851=B_SPLINE_CURVE_WITH_KNOTS('',3,(#27821,#27822,#27823,#27824),
 .UNSPECIFIED.,.F.,.F.,(4,4),(-0.0707432948545235,-3.34525766380878E-6),
 .UNSPECIFIED.);
#3852=B_SPLINE_CURVE_WITH_KNOTS('',3,(#27828,#27829,#27830,#27831,#27832,
#27833,#27834,#27835,#27836,#27837,#27838,#27839,#27840,#27841,#27842,#27843,
#27844,#27845,#27846,#27847,#27848,#27849,#27850,#27851,#27852,#27853,#27854,
#27855,#27856,#27857,#27858,#27859,#27860,#27861,#27862,#27863,#27864,#27865,
#27866,#27867,#27868,#27869,#27870,#27871,#27872,#27873,#27874,#27875,#27876,
#27877,#27878,#27879,#27880,#27881,#27882,#27883,#27884,#27885,#27886,#27887,
#27888,#27889,#27890,#27891,#27892,#27893,#27894,#27895,#27896,#27897,#27898,
#27899,#27900,#27901,#27902,#27903,#27904,#27905,#27906,#27907,#27908,#27909,
#27910,#27911,#27912,#27913,#27914,#27915,#27916,#27917,#27918),
 .UNSPECIFIED.,.F.,.F.,(4,3,3,3,3,3,3,3,3,3,3,3,3,3,3,3,3,3,3,3,3,3,3,3,
3,3,3,3,3,3,4),(-0.461463988274541,-0.386087506167661,-0.372903671306323,
-0.36421409612757,-0.352528758081246,-0.339636892136157,-0.338448280177947,
-0.328074919236012,-0.316383789572668,-0.304885949019545,-0.297243973048271,
-0.288858567477107,-0.282882239837598,-0.277347677282806,-0.271340988166504,
-0.265007390818464,-0.258044852490757,-0.254459737762025,-0.242044020405013,
-0.228141105146501,-0.213185106576004,-0.197120884701682,-0.179636878474788,
-0.161760929349414,-0.144350238406641,-0.134249918117004,-0.102125955921634,
-0.0702664487997089,-0.0525746845214139,-0.02166066501539,0.),
 .UNSPECIFIED.);
#3853=B_SPLINE_CURVE_WITH_KNOTS('',3,(#27921,#27922,#27923,#27924,#27925,
#27926,#27927,#27928,#27929,#27930,#27931,#27932,#27933,#27934,#27935,#27936,
#27937,#27938,#27939,#27940,#27941,#27942,#27943,#27944,#27945,#27946,#27947,
#27948,#27949,#27950,#27951,#27952,#27953,#27954,#27955,#27956,#27957,#27958,
#27959,#27960,#27961,#27962,#27963,#27964,#27965,#27966,#27967,#27968,#27969,
#27970,#27971,#27972,#27973,#27974,#27975,#27976,#27977,#27978,#27979,#27980,
#27981,#27982,#27983,#27984),.UNSPECIFIED.,.F.,.F.,(4,3,3,3,3,3,3,3,3,3,
3,3,3,3,3,3,3,3,3,3,3,4),(-0.976443208995993,-0.960629666524146,-0.949661288965092,
-0.931972270488235,-0.914398186943459,-0.904644103415597,-0.893317754842137,
-0.880493104971779,-0.866940956882255,-0.85260546798694,-0.837134239960023,
-0.82157385570265,-0.80614720579096,-0.79187466047125,-0.790720555879271,
-0.779060485592236,-0.740625,-0.691250000000001,-0.5925,-0.49375,-0.394999999999999,
-0.0499999999999998),.UNSPECIFIED.);
#3854=B_SPLINE_CURVE_WITH_KNOTS('',3,(#28176,#28177,#28178,#28179),
 .UNSPECIFIED.,.F.,.F.,(4,4),(-0.253410853624616,-0.103262412077185),
 .UNSPECIFIED.);
#3855=B_SPLINE_CURVE_WITH_KNOTS('',3,(#28181,#28182,#28183,#28184),
 .UNSPECIFIED.,.F.,.F.,(4,4),(0.,0.29),.UNSPECIFIED.);
#3856=B_SPLINE_CURVE_WITH_KNOTS('',3,(#28185,#28186,#28187,#28188),
 .UNSPECIFIED.,.F.,.F.,(4,4),(3.28350553660553,3.37607250252489),
 .UNSPECIFIED.);
#3857=B_SPLINE_CURVE_WITH_KNOTS('',3,(#28190,#28191,#28192,#28193,#28194,
#28195),.UNSPECIFIED.,.F.,.F.,(4,2,4),(-2.17700203273975,-1.38478587807843,
-0.288632999074765),.UNSPECIFIED.);
#3858=B_SPLINE_CURVE_WITH_KNOTS('',3,(#28197,#28198,#28199,#28200,#28201,
#28202,#28203,#28204,#28205,#28206,#28207,#28208,#28209,#28210,#28211,#28212,
#28213,#28214,#28215,#28216,#28217,#28218,#28219,#28220,#28221,#28222,#28223,
#28224,#28225,#28226,#28227),.UNSPECIFIED.,.F.,.F.,(4,3,3,3,3,3,3,3,3,3,
4),(0.664704897780732,0.688351938092992,0.780317238696425,0.810486879810963,
0.862717972416611,0.955520663501275,1.01466394039954,1.06038302616807,1.10529572457683,
1.13272802062135,1.20216888729732),.UNSPECIFIED.);
#3859=B_SPLINE_CURVE_WITH_KNOTS('',3,(#28228,#28229,#28230,#28231,#28232,
#28233,#28234,#28235,#28236,#28237,#28238,#28239,#28240,#28241,#28242,#28243,
#28244,#28245,#28246),.UNSPECIFIED.,.F.,.F.,(4,3,3,3,3,3,4),(0.,0.178790961538472,
0.350742859481108,0.449205432353048,0.513879914408647,0.522694757423744,
0.664704897780732),.UNSPECIFIED.);
#3860=B_SPLINE_CURVE_WITH_KNOTS('',3,(#28250,#28251,#28252,#28253),
 .UNSPECIFIED.,.F.,.F.,(4,4),(-0.0707400285408625,0.),.UNSPECIFIED.);
#3861=B_SPLINE_CURVE_WITH_KNOTS('',3,(#28257,#28258,#28259,#28260),
 .UNSPECIFIED.,.F.,.F.,(4,4),(-0.0707432954689054,-3.34525766178262E-6),
 .UNSPECIFIED.);
#3862=B_SPLINE_CURVE_WITH_KNOTS('',3,(#28264,#28265,#28266,#28267,#28268,
#28269,#28270,#28271,#28272,#28273,#28274,#28275,#28276,#28277,#28278,#28279,
#28280,#28281,#28282,#28283,#28284,#28285,#28286,#28287,#28288,#28289,#28290,
#28291,#28292,#28293,#28294,#28295,#28296,#28297,#28298,#28299,#28300,#28301,
#28302,#28303,#28304,#28305,#28306,#28307,#28308,#28309,#28310,#28311,#28312,
#28313,#28314,#28315,#28316,#28317,#28318,#28319,#28320,#28321,#28322,#28323,
#28324,#28325,#28326,#28327,#28328,#28329,#28330,#28331,#28332,#28333,#28334,
#28335,#28336,#28337,#28338,#28339,#28340,#28341,#28342,#28343,#28344,#28345,
#28346,#28347,#28348,#28349,#28350,#28351,#28352,#28353,#28354,#28355,#28356,
#28357,#28358,#28359,#28360),.UNSPECIFIED.,.F.,.F.,(4,3,3,3,3,3,3,3,3,3,
3,3,3,3,3,3,3,3,3,3,3,3,3,3,3,3,3,3,3,3,3,3,4),(-0.461463988274541,-0.386087506167661,
-0.372903671306323,-0.36421409612757,-0.349922618618476,-0.338448280177947,
-0.328550793223587,-0.322977024945215,-0.314822638010309,-0.306007155782235,
-0.304885949019545,-0.297658439870379,-0.289754515056109,-0.282882239837598,
-0.277393071545031,-0.271439067306372,-0.265165133454002,-0.258272116803473,
-0.254459737762025,-0.242193625916565,-0.2284734588626,-0.213717473130501,
-0.197852099811634,-0.180468088683695,-0.162567602548416,-0.144906258984996,
-0.134249918117004,-0.102205018832853,-0.0696974934620852,-0.0525746845214139,
-0.0222228841287548,-0.000827460244363642,0.),.UNSPECIFIED.);
#3863=B_SPLINE_CURVE_WITH_KNOTS('',3,(#28363,#28364,#28365,#28366,#28367,
#28368,#28369,#28370,#28371,#28372,#28373,#28374,#28375,#28376,#28377,#28378,
#28379,#28380,#28381,#28382,#28383,#28384,#28385,#28386,#28387,#28388,#28389,
#28390,#28391,#28392,#28393,#28394,#28395,#28396,#28397,#28398,#28399,#28400,
#28401,#28402,#28403,#28404,#28405,#28406,#28407,#28408,#28409,#28410,#28411,
#28412,#28413,#28414,#28415,#28416,#28417,#28418,#28419,#28420,#28421,#28422,
#28423,#28424,#28425,#28426),.UNSPECIFIED.,.F.,.F.,(4,3,3,3,3,3,3,3,3,3,
3,3,3,3,3,3,3,3,3,3,3,4),(-0.976443208995993,-0.960628704721015,-0.949661288965092,
-0.931975105549615,-0.914400310860217,-0.904644103415597,-0.893320015681317,
-0.880495083206061,-0.866943636882904,-0.852607981525575,-0.837136125113999,
-0.821574066138986,-0.806147311009128,-0.791872999074624,-0.790720555879271,
-0.779060485592236,-0.740625,-0.691250000000001,-0.5925,-0.49375,-0.394999999999999,
-0.0499999999999998),.UNSPECIFIED.);
#3864=B_SPLINE_CURVE_WITH_KNOTS('',3,(#28648,#28649,#28650,#28651),
 .UNSPECIFIED.,.F.,.F.,(4,4),(-0.253410853624616,-0.103262412077186),
 .UNSPECIFIED.);
#3865=B_SPLINE_CURVE_WITH_KNOTS('',3,(#28653,#28654,#28655,#28656),
 .UNSPECIFIED.,.F.,.F.,(4,4),(0.,0.29),.UNSPECIFIED.);
#3866=B_SPLINE_CURVE_WITH_KNOTS('',3,(#28657,#28658,#28659,#28660),
 .UNSPECIFIED.,.F.,.F.,(4,4),(3.28350553660308,3.37607250251481),
 .UNSPECIFIED.);
#3867=B_SPLINE_CURVE_WITH_KNOTS('',3,(#28662,#28663,#28664,#28665,#28666,
#28667),.UNSPECIFIED.,.F.,.F.,(4,2,4),(-2.17700203273975,-1.38478587807843,
-0.288632999074765),.UNSPECIFIED.);
#3868=B_SPLINE_CURVE_WITH_KNOTS('',3,(#28669,#28670,#28671,#28672,#28673,
#28674,#28675,#28676,#28677,#28678,#28679,#28680,#28681,#28682,#28683,#28684,
#28685,#28686,#28687,#28688,#28689,#28690,#28691,#28692,#28693,#28694,#28695,
#28696,#28697,#28698,#28699),.UNSPECIFIED.,.F.,.F.,(4,3,3,3,3,3,3,3,3,3,
4),(0.664704897780732,0.688351938092992,0.780317238696443,0.810486879810963,
0.862717972416633,0.955520663501275,1.0146639403997,1.06038302616807,1.10529572457683,
1.13272802062135,1.20216888729732),.UNSPECIFIED.);
#3869=B_SPLINE_CURVE_WITH_KNOTS('',3,(#28700,#28701,#28702,#28703,#28704,
#28705,#28706,#28707,#28708,#28709,#28710,#28711,#28712,#28713,#28714,#28715,
#28716,#28717,#28718),.UNSPECIFIED.,.F.,.F.,(4,3,3,3,3,3,4),(0.,0.178790961538472,
0.350742859481108,0.449205432353048,0.513879914408647,0.522694757423744,
0.664704897780732),.UNSPECIFIED.);
#3870=B_SPLINE_CURVE_WITH_KNOTS('',3,(#28722,#28723,#28724,#28725),
 .UNSPECIFIED.,.F.,.F.,(4,4),(-0.0707400283740959,0.),.UNSPECIFIED.);
#3871=B_SPLINE_CURVE_WITH_KNOTS('',3,(#28729,#28730,#28731,#28732),
 .UNSPECIFIED.,.F.,.F.,(4,4),(-0.0707432954466584,-3.34525766253202E-6),
 .UNSPECIFIED.);
#3872=B_SPLINE_CURVE_WITH_KNOTS('',3,(#28736,#28737,#28738,#28739,#28740,
#28741,#28742,#28743,#28744,#28745,#28746,#28747,#28748,#28749,#28750,#28751,
#28752,#28753,#28754,#28755,#28756,#28757,#28758,#28759,#28760,#28761,#28762,
#28763,#28764,#28765,#28766,#28767,#28768,#28769,#28770,#28771,#28772,#28773,
#28774,#28775,#28776,#28777,#28778,#28779,#28780,#28781,#28782,#28783,#28784,
#28785,#28786,#28787,#28788,#28789,#28790,#28791,#28792,#28793,#28794,#28795,
#28796,#28797,#28798,#28799,#28800,#28801,#28802,#28803,#28804,#28805,#28806,
#28807,#28808,#28809,#28810,#28811,#28812,#28813,#28814,#28815,#28816,#28817,
#28818,#28819,#28820,#28821,#28822,#28823,#28824,#28825,#28826,#28827,#28828,
#28829,#28830,#28831,#28832),.UNSPECIFIED.,.F.,.F.,(4,3,3,3,3,3,3,3,3,3,
3,3,3,3,3,3,3,3,3,3,3,3,3,3,3,3,3,3,3,3,3,3,4),(-0.461463988274541,-0.386087506167661,
-0.375299929924104,-0.372903671306323,-0.356077696752448,-0.352040116130794,
-0.339920267375323,-0.338448280177947,-0.326632246672124,-0.313204943761436,
-0.304885949019545,-0.29982124014814,-0.293952204614803,-0.287658393406508,
-0.282882239837598,-0.277507204165034,-0.271689255077659,-0.265572046854325,
-0.258868973352318,-0.254459737762025,-0.241918019250842,-0.227822266677611,
-0.212603244487091,-0.196183063900774,-0.178197554741625,-0.159751102176005,
-0.141758270370875,-0.134249918117004,-0.10123360556295,-0.068219375707454,
-0.0525746845214139,-0.0245175806023862,0.),.UNSPECIFIED.);
#3873=B_SPLINE_CURVE_WITH_KNOTS('',3,(#28835,#28836,#28837,#28838,#28839,
#28840,#28841,#28842,#28843,#28844,#28845,#28846,#28847,#28848,#28849,#28850,
#28851,#28852,#28853,#28854,#28855,#28856,#28857,#28858,#28859,#28860,#28861,
#28862,#28863,#28864,#28865,#28866,#28867,#28868,#28869,#28870,#28871,#28872,
#28873,#28874,#28875,#28876,#28877,#28878,#28879,#28880,#28881,#28882,#28883,
#28884,#28885,#28886,#28887,#28888,#28889,#28890,#28891,#28892,#28893,#28894,
#28895,#28896,#28897,#28898),.UNSPECIFIED.,.F.,.F.,(4,3,3,3,3,3,3,3,3,3,
3,3,3,3,3,3,3,3,3,3,3,4),(-0.976443208995993,-0.959642323211355,-0.949661288965092,
-0.932497758133295,-0.914973156724424,-0.904644103415597,-0.893686857853989,
-0.881830566008639,-0.868587665962165,-0.854441220699773,-0.839436072992889,
-0.823696621722087,-0.808086574213453,-0.793469897333356,-0.790720555879271,
-0.779060485592236,-0.740625,-0.691250000000001,-0.5925,-0.543125,-0.394999999999999,
-0.0499999999999998),.UNSPECIFIED.);
#3874=B_SPLINE_CURVE_WITH_KNOTS('',3,(#29110,#29111,#29112,#29113),
 .UNSPECIFIED.,.F.,.F.,(4,4),(-0.253410853624616,-0.103262412077185),
 .UNSPECIFIED.);
#3875=B_SPLINE_CURVE_WITH_KNOTS('',3,(#29115,#29116,#29117,#29118),
 .UNSPECIFIED.,.F.,.F.,(4,4),(0.,0.29),.UNSPECIFIED.);
#3876=B_SPLINE_CURVE_WITH_KNOTS('',3,(#29119,#29120,#29121,#29122),
 .UNSPECIFIED.,.F.,.F.,(4,4),(3.28350553697936,3.37607250293456),
 .UNSPECIFIED.);
#3877=B_SPLINE_CURVE_WITH_KNOTS('',3,(#29124,#29125,#29126,#29127,#29128,
#29129),.UNSPECIFIED.,.F.,.F.,(4,2,4),(-2.17700203273975,-1.38478587807843,
-0.288632999074766),.UNSPECIFIED.);
#3878=B_SPLINE_CURVE_WITH_KNOTS('',3,(#29131,#29132,#29133,#29134,#29135,
#29136,#29137,#29138,#29139,#29140,#29141,#29142,#29143,#29144,#29145,#29146,
#29147,#29148,#29149,#29150,#29151,#29152,#29153,#29154,#29155,#29156,#29157,
#29158,#29159,#29160,#29161),.UNSPECIFIED.,.F.,.F.,(4,3,3,3,3,3,3,3,3,3,
4),(0.664704897780732,0.688351938092992,0.780317238696442,0.810486879810963,
0.862717972416637,0.955520663501275,1.01466394039962,1.06038302616807,1.10529572457683,
1.13272802062135,1.20216888729732),.UNSPECIFIED.);
#3879=B_SPLINE_CURVE_WITH_KNOTS('',3,(#29162,#29163,#29164,#29165,#29166,
#29167,#29168,#29169,#29170,#29171,#29172,#29173,#29174,#29175,#29176,#29177,
#29178,#29179,#29180),.UNSPECIFIED.,.F.,.F.,(4,3,3,3,3,3,4),(0.,0.178790961538472,
0.350742859481108,0.449205432353047,0.513879914408646,0.522694757423744,
0.664704897780732),.UNSPECIFIED.);
#3880=B_SPLINE_CURVE_WITH_KNOTS('',3,(#29184,#29185,#29186,#29187),
 .UNSPECIFIED.,.F.,.F.,(4,4),(-0.070740028353927,0.),.UNSPECIFIED.);
#3881=B_SPLINE_CURVE_WITH_KNOTS('',3,(#29191,#29192,#29193,#29194),
 .UNSPECIFIED.,.F.,.F.,(4,4),(-0.0707432948167915,-3.34525766403082E-6),
 .UNSPECIFIED.);
#3882=B_SPLINE_CURVE_WITH_KNOTS('',3,(#29198,#29199,#29200,#29201,#29202,
#29203,#29204,#29205,#29206,#29207,#29208,#29209,#29210,#29211,#29212,#29213,
#29214,#29215,#29216,#29217,#29218,#29219,#29220,#29221,#29222,#29223,#29224,
#29225,#29226,#29227,#29228,#29229,#29230,#29231,#29232,#29233,#29234,#29235,
#29236,#29237,#29238,#29239,#29240,#29241,#29242,#29243,#29244,#29245,#29246,
#29247,#29248,#29249,#29250,#29251,#29252,#29253,#29254,#29255,#29256,#29257,
#29258,#29259,#29260,#29261,#29262,#29263,#29264,#29265,#29266,#29267,#29268,
#29269,#29270,#29271,#29272,#29273,#29274,#29275,#29276,#29277,#29278,#29279,
#29280,#29281,#29282,#29283,#29284,#29285,#29286,#29287,#29288),
 .UNSPECIFIED.,.F.,.F.,(4,3,3,3,3,3,3,3,3,3,3,3,3,3,3,3,3,3,3,3,3,3,3,3,
3,3,3,3,3,3,4),(-0.461463988274541,-0.386087506167661,-0.372903671306323,
-0.36421409612757,-0.352528758081253,-0.339636892136,-0.338448280177947,
-0.328074919236012,-0.316383789572691,-0.304885949019545,-0.297243973048271,
-0.288858567477107,-0.282882239837598,-0.277347677282806,-0.271340988166504,
-0.265007390818464,-0.258044852490787,-0.254459737762025,-0.242044020405011,
-0.228141105146502,-0.213185106575989,-0.1971208847016,-0.179636878474718,
-0.161760929349413,-0.144350238406588,-0.134249918117004,-0.102125955921634,
-0.070266448799884,-0.0525746845214139,-0.0216606650153916,0.),
 .UNSPECIFIED.);
#3883=B_SPLINE_CURVE_WITH_KNOTS('',3,(#29291,#29292,#29293,#29294,#29295,
#29296,#29297,#29298,#29299,#29300,#29301,#29302,#29303,#29304,#29305,#29306,
#29307,#29308,#29309,#29310,#29311,#29312,#29313,#29314,#29315,#29316,#29317,
#29318,#29319,#29320,#29321,#29322,#29323,#29324,#29325,#29326,#29327,#29328,
#29329,#29330,#29331,#29332,#29333,#29334,#29335,#29336,#29337,#29338,#29339,
#29340,#29341,#29342,#29343,#29344,#29345,#29346,#29347,#29348,#29349,#29350,
#29351,#29352,#29353,#29354),.UNSPECIFIED.,.F.,.F.,(4,3,3,3,3,3,3,3,3,3,
3,3,3,3,3,3,3,3,3,3,3,4),(-0.976443208995993,-0.960629666524142,-0.949661288965092,
-0.931972270488239,-0.91439818694324,-0.904644103415597,-0.893317754842134,
-0.880493104971777,-0.866940956882277,-0.852605467987382,-0.837134239960354,
-0.821573855703088,-0.806147205791179,-0.791874660471442,-0.790720555879271,
-0.779060485592236,-0.740625,-0.691250000000001,-0.5925,-0.49375,-0.394999999999999,
-0.0499999999999998),.UNSPECIFIED.);
#3884=B_SPLINE_CURVE_WITH_KNOTS('',3,(#29546,#29547,#29548,#29549),
 .UNSPECIFIED.,.F.,.F.,(4,4),(-0.253410853624616,-0.103262412077186),
 .UNSPECIFIED.);
#3885=B_SPLINE_CURVE_WITH_KNOTS('',3,(#29551,#29552,#29553,#29554),
 .UNSPECIFIED.,.F.,.F.,(4,4),(0.,0.29),.UNSPECIFIED.);
#3886=B_SPLINE_CURVE_WITH_KNOTS('',3,(#29555,#29556,#29557,#29558),
 .UNSPECIFIED.,.F.,.F.,(4,4),(3.28350553753493,3.3760725035161),
 .UNSPECIFIED.);
#3887=B_SPLINE_CURVE_WITH_KNOTS('',3,(#29560,#29561,#29562,#29563,#29564,
#29565),.UNSPECIFIED.,.F.,.F.,(4,2,4),(-2.17700203273975,-1.38478587807843,
-0.288632999074765),.UNSPECIFIED.);
#3888=B_SPLINE_CURVE_WITH_KNOTS('',3,(#29567,#29568,#29569,#29570,#29571,
#29572,#29573,#29574,#29575,#29576,#29577,#29578,#29579,#29580,#29581,#29582,
#29583,#29584,#29585,#29586,#29587,#29588,#29589,#29590,#29591,#29592,#29593,
#29594,#29595,#29596,#29597),.UNSPECIFIED.,.F.,.F.,(4,3,3,3,3,3,3,3,3,3,
4),(0.664704897780732,0.688351938092992,0.780317238696427,0.810486879810963,
0.862717972416633,0.955520663501275,1.01466394039958,1.06038302616807,1.10529572457683,
1.13272802062135,1.20216888729732),.UNSPECIFIED.);
#3889=B_SPLINE_CURVE_WITH_KNOTS('',3,(#29598,#29599,#29600,#29601,#29602,
#29603,#29604,#29605,#29606,#29607,#29608,#29609,#29610,#29611,#29612,#29613,
#29614,#29615,#29616),.UNSPECIFIED.,.F.,.F.,(4,3,3,3,3,3,4),(0.,0.178790961538472,
0.350742859481108,0.449205432353047,0.513879914408645,0.522694757423744,
0.664704897780732),.UNSPECIFIED.);
#3890=B_SPLINE_CURVE_WITH_KNOTS('',3,(#29620,#29621,#29622,#29623),
 .UNSPECIFIED.,.F.,.F.,(4,4),(-0.0707400285050858,0.),.UNSPECIFIED.);
#3891=B_SPLINE_CURVE_WITH_KNOTS('',3,(#29627,#29628,#29629,#29630),
 .UNSPECIFIED.,.F.,.F.,(4,4),(-0.0707432949753092,-3.34525766367E-6),
 .UNSPECIFIED.);
#3892=B_SPLINE_CURVE_WITH_KNOTS('',3,(#29634,#29635,#29636,#29637,#29638,
#29639,#29640,#29641,#29642,#29643,#29644,#29645,#29646,#29647,#29648,#29649,
#29650,#29651,#29652,#29653,#29654,#29655,#29656,#29657,#29658,#29659,#29660,
#29661,#29662,#29663,#29664,#29665,#29666,#29667,#29668,#29669,#29670,#29671,
#29672,#29673,#29674,#29675,#29676,#29677,#29678,#29679,#29680,#29681,#29682,
#29683,#29684,#29685,#29686,#29687,#29688,#29689,#29690,#29691,#29692,#29693,
#29694,#29695,#29696,#29697,#29698,#29699,#29700,#29701,#29702,#29703,#29704,
#29705,#29706,#29707,#29708,#29709,#29710,#29711,#29712,#29713,#29714,#29715,
#29716,#29717,#29718,#29719,#29720,#29721,#29722,#29723,#29724,#29725,#29726,
#29727,#29728,#29729,#29730),.UNSPECIFIED.,.F.,.F.,(4,3,3,3,3,3,3,3,3,3,
3,3,3,3,3,3,3,3,3,3,3,3,3,3,3,3,3,3,3,3,3,3,4),(-0.461463988274541,-0.386087506167661,
-0.372903671306323,-0.36421409612757,-0.349922618627789,-0.338448280177947,
-0.328550793223787,-0.322977024945215,-0.314822638010135,-0.306007155781963,
-0.304885949019545,-0.297658439870205,-0.289754515055765,-0.282882239837598,
-0.277393071544922,-0.271439067306183,-0.265165133453763,-0.25827211680326,
-0.254459737762025,-0.242193625915918,-0.228473458861481,-0.213717473129083,
-0.197852099810681,-0.180468088688272,-0.162567602565291,-0.144906259020414,
-0.134249918117004,-0.102205019200819,-0.0696974945135463,-0.0525746845214139,
-0.0222228838221726,-0.000827460244363642,0.),.UNSPECIFIED.);
#3893=B_SPLINE_CURVE_WITH_KNOTS('',3,(#29733,#29734,#29735,#29736,#29737,
#29738,#29739,#29740,#29741,#29742,#29743,#29744,#29745,#29746,#29747,#29748,
#29749,#29750,#29751,#29752,#29753,#29754,#29755,#29756,#29757,#29758,#29759,
#29760,#29761,#29762,#29763,#29764,#29765,#29766,#29767,#29768,#29769,#29770,
#29771,#29772,#29773,#29774,#29775,#29776,#29777,#29778,#29779,#29780,#29781,
#29782,#29783,#29784,#29785,#29786,#29787,#29788,#29789,#29790,#29791,#29792,
#29793,#29794,#29795,#29796),.UNSPECIFIED.,.F.,.F.,(4,3,3,3,3,3,3,3,3,3,
3,3,3,3,3,3,3,3,3,3,3,4),(-0.976443208995993,-0.96062870472102,-0.949661288965092,
-0.931975105549613,-0.91440031086007,-0.904644103415597,-0.893320015681315,
-0.880495083206059,-0.866943636882815,-0.852607981525168,-0.837136125113694,
-0.821574066138705,-0.806147311008988,-0.791872999074437,-0.790720555879271,
-0.779060485592236,-0.740625,-0.691250000000001,-0.5925,-0.49375,-0.394999999999999,
-0.0499999999999998),.UNSPECIFIED.);
#3894=B_SPLINE_CURVE_WITH_KNOTS('',3,(#30018,#30019,#30020,#30021),
 .UNSPECIFIED.,.F.,.F.,(4,4),(-0.253410853624616,-0.103262412077185),
 .UNSPECIFIED.);
#3895=B_SPLINE_CURVE_WITH_KNOTS('',3,(#30023,#30024,#30025,#30026),
 .UNSPECIFIED.,.F.,.F.,(4,4),(0.,0.29),.UNSPECIFIED.);
#3896=B_SPLINE_CURVE_WITH_KNOTS('',3,(#30027,#30028,#30029,#30030),
 .UNSPECIFIED.,.F.,.F.,(4,4),(3.28350553820744,3.37607250422172),
 .UNSPECIFIED.);
#3897=B_SPLINE_CURVE_WITH_KNOTS('',3,(#30032,#30033,#30034,#30035,#30036,
#30037),.UNSPECIFIED.,.F.,.F.,(4,2,4),(-2.17700203273975,-1.38478587807843,
-0.288632999074765),.UNSPECIFIED.);
#3898=B_SPLINE_CURVE_WITH_KNOTS('',3,(#30039,#30040,#30041,#30042,#30043,
#30044,#30045,#30046,#30047,#30048,#30049,#30050,#30051,#30052,#30053,#30054,
#30055,#30056,#30057,#30058,#30059,#30060,#30061,#30062,#30063,#30064,#30065,
#30066,#30067,#30068,#30069),.UNSPECIFIED.,.F.,.F.,(4,3,3,3,3,3,3,3,3,3,
4),(0.664704897780732,0.688351938092992,0.780317238696421,0.810486879810963,
0.862717972416634,0.955520663501275,1.01466394039958,1.06038302616807,1.10529572457683,
1.13272802062135,1.20216888729732),.UNSPECIFIED.);
#3899=B_SPLINE_CURVE_WITH_KNOTS('',3,(#30070,#30071,#30072,#30073,#30074,
#30075,#30076,#30077,#30078,#30079,#30080,#30081,#30082,#30083,#30084,#30085,
#30086,#30087,#30088),.UNSPECIFIED.,.F.,.F.,(4,3,3,3,3,3,4),(0.,0.178790961538472,
0.350742859481108,0.449205432353047,0.513879914408646,0.522694757423744,
0.664704897780732),.UNSPECIFIED.);
#3900=B_SPLINE_CURVE_WITH_KNOTS('',3,(#30092,#30093,#30094,#30095),
 .UNSPECIFIED.,.F.,.F.,(4,4),(-0.0707400282391991,0.),.UNSPECIFIED.);
#3901=B_SPLINE_CURVE_WITH_KNOTS('',3,(#30099,#30100,#30101,#30102),
 .UNSPECIFIED.,.F.,.F.,(4,4),(-0.0707432951646884,-3.34525766250426E-6),
 .UNSPECIFIED.);
#3902=B_SPLINE_CURVE_WITH_KNOTS('',3,(#30106,#30107,#30108,#30109,#30110,
#30111,#30112,#30113,#30114,#30115,#30116,#30117,#30118,#30119,#30120,#30121,
#30122,#30123,#30124,#30125,#30126,#30127,#30128,#30129,#30130,#30131,#30132,
#30133,#30134,#30135,#30136,#30137,#30138,#30139,#30140,#30141,#30142,#30143,
#30144,#30145,#30146,#30147,#30148,#30149,#30150,#30151,#30152,#30153,#30154,
#30155,#30156,#30157,#30158,#30159,#30160,#30161,#30162,#30163,#30164,#30165,
#30166,#30167,#30168,#30169,#30170,#30171,#30172,#30173,#30174,#30175,#30176,
#30177,#30178,#30179,#30180,#30181,#30182,#30183,#30184,#30185,#30186,#30187,
#30188,#30189,#30190,#30191,#30192,#30193,#30194,#30195,#30196,#30197,#30198,
#30199,#30200,#30201,#30202),.UNSPECIFIED.,.F.,.F.,(4,3,3,3,3,3,3,3,3,3,
3,3,3,3,3,3,3,3,3,3,3,3,3,3,3,3,3,3,3,3,3,3,4),(-0.461463988274541,-0.386087506167661,
-0.375299929924104,-0.372903671306323,-0.356077696752447,-0.352040116130794,
-0.339920267375323,-0.338448280177947,-0.326632246672126,-0.313204943761465,
-0.304885949019545,-0.29982124014814,-0.293952204614803,-0.287658393406508,
-0.282882239837598,-0.277507204165034,-0.271689255077659,-0.265572046854315,
-0.25886897335229,-0.254459737762025,-0.241918019250842,-0.227822266677592,
-0.212603244487111,-0.196183063900843,-0.178197554741787,-0.159751102176188,
-0.141758270371022,-0.134249918117004,-0.10123360556295,-0.0682193757076537,
-0.0525746845214139,-0.0245175806023846,0.),.UNSPECIFIED.);
#3903=B_SPLINE_CURVE_WITH_KNOTS('',3,(#30205,#30206,#30207,#30208,#30209,
#30210,#30211,#30212,#30213,#30214,#30215,#30216,#30217,#30218,#30219,#30220,
#30221,#30222,#30223,#30224,#30225,#30226,#30227,#30228,#30229,#30230,#30231,
#30232,#30233,#30234,#30235,#30236,#30237,#30238,#30239,#30240,#30241,#30242,
#30243,#30244,#30245,#30246,#30247,#30248,#30249,#30250,#30251,#30252,#30253,
#30254,#30255,#30256,#30257,#30258,#30259,#30260,#30261,#30262,#30263,#30264,
#30265,#30266,#30267,#30268),.UNSPECIFIED.,.F.,.F.,(4,3,3,3,3,3,3,3,3,3,
3,3,3,3,3,3,3,3,3,3,3,4),(-0.976443208995993,-0.959641771463709,-0.949661288965092,
-0.932500795758733,-0.914975318861591,-0.904644103415597,-0.893689140152815,
-0.881835075865074,-0.86859336767674,-0.854447019507201,-0.83944073270216,
-0.82369847532938,-0.808085046249769,-0.793464970994094,-0.790720555879271,
-0.779060485592236,-0.740625,-0.691250000000001,-0.5925,-0.543125,-0.394999999999999,
-0.0499999999999998),.UNSPECIFIED.);
#3904=B_SPLINE_CURVE_WITH_KNOTS('',3,(#30480,#30481,#30482,#30483),
 .UNSPECIFIED.,.F.,.F.,(4,4),(-0.253410853624616,-0.103262412077185),
 .UNSPECIFIED.);
#3905=B_SPLINE_CURVE_WITH_KNOTS('',3,(#30485,#30486,#30487,#30488),
 .UNSPECIFIED.,.F.,.F.,(4,4),(0.,0.29),.UNSPECIFIED.);
#3906=B_SPLINE_CURVE_WITH_KNOTS('',3,(#30489,#30490,#30491,#30492),
 .UNSPECIFIED.,.F.,.F.,(4,4),(3.28350553686237,3.37607250280011),
 .UNSPECIFIED.);
#3907=B_SPLINE_CURVE_WITH_KNOTS('',3,(#30494,#30495,#30496,#30497,#30498,
#30499),.UNSPECIFIED.,.F.,.F.,(4,2,4),(-2.17700203273975,-1.38478587807843,
-0.288632999074765),.UNSPECIFIED.);
#3908=B_SPLINE_CURVE_WITH_KNOTS('',3,(#30501,#30502,#30503,#30504,#30505,
#30506,#30507,#30508,#30509,#30510,#30511,#30512,#30513,#30514,#30515,#30516,
#30517,#30518,#30519,#30520,#30521,#30522,#30523,#30524,#30525,#30526,#30527,
#30528,#30529,#30530,#30531),.UNSPECIFIED.,.F.,.F.,(4,3,3,3,3,3,3,3,3,3,
4),(0.664704897780732,0.688351938092992,0.78031723869643,0.810486879810963,
0.862717972416625,0.955520663501275,1.01466394039959,1.06038302616807,1.10529572457683,
1.13272802062135,1.20216888729732),.UNSPECIFIED.);
#3909=B_SPLINE_CURVE_WITH_KNOTS('',3,(#30532,#30533,#30534,#30535,#30536,
#30537,#30538,#30539,#30540,#30541,#30542,#30543,#30544,#30545,#30546,#30547,
#30548,#30549,#30550),.UNSPECIFIED.,.F.,.F.,(4,3,3,3,3,3,4),(0.,0.178790961538472,
0.350742859481108,0.449205432353047,0.513879914408646,0.522694757423744,
0.664704897780732),.UNSPECIFIED.);
#3910=B_SPLINE_CURVE_WITH_KNOTS('',3,(#30554,#30555,#30556,#30557),
 .UNSPECIFIED.,.F.,.F.,(4,4),(-0.0707400284125705,0.),.UNSPECIFIED.);
#3911=B_SPLINE_CURVE_WITH_KNOTS('',3,(#30561,#30562,#30563,#30564),
 .UNSPECIFIED.,.F.,.F.,(4,4),(-0.0707432947474667,-3.34525766357285E-6),
 .UNSPECIFIED.);
#3912=B_SPLINE_CURVE_WITH_KNOTS('',3,(#30568,#30569,#30570,#30571,#30572,
#30573,#30574,#30575,#30576,#30577,#30578,#30579,#30580,#30581,#30582,#30583,
#30584,#30585,#30586,#30587,#30588,#30589,#30590,#30591,#30592,#30593,#30594,
#30595,#30596,#30597,#30598,#30599,#30600,#30601,#30602,#30603,#30604,#30605,
#30606,#30607,#30608,#30609,#30610,#30611,#30612,#30613,#30614,#30615,#30616,
#30617,#30618,#30619,#30620,#30621,#30622,#30623,#30624,#30625,#30626,#30627,
#30628,#30629,#30630,#30631,#30632,#30633,#30634,#30635,#30636,#30637,#30638,
#30639,#30640,#30641,#30642,#30643,#30644,#30645,#30646,#30647,#30648,#30649,
#30650,#30651,#30652,#30653,#30654,#30655,#30656,#30657,#30658),
 .UNSPECIFIED.,.F.,.F.,(4,3,3,3,3,3,3,3,3,3,3,3,3,3,3,3,3,3,3,3,3,3,3,3,
3,3,3,3,3,3,4),(-0.461463988274541,-0.386087506167661,-0.372903671306323,
-0.36421409612757,-0.35252875808128,-0.339636892136031,-0.338448280177947,
-0.328074919236012,-0.316383789572668,-0.304885949019545,-0.297243973048271,
-0.288858567477107,-0.282882239837598,-0.277347677282808,-0.271340988166513,
-0.265007390818488,-0.258044852490789,-0.254459737762025,-0.242044020405011,
-0.228141105146501,-0.21318510657597,-0.197120884701618,-0.179636878474804,
-0.161760929349425,-0.144350238406565,-0.134249918117004,-0.102125955921629,
-0.0702664487999561,-0.0525746845214139,-0.021660665015393,0.),
 .UNSPECIFIED.);
#3913=B_SPLINE_CURVE_WITH_KNOTS('',3,(#30661,#30662,#30663,#30664,#30665,
#30666,#30667,#30668,#30669,#30670,#30671,#30672,#30673,#30674,#30675,#30676,
#30677,#30678,#30679,#30680,#30681,#30682,#30683,#30684,#30685,#30686,#30687,
#30688,#30689,#30690,#30691,#30692,#30693,#30694,#30695,#30696,#30697,#30698,
#30699,#30700,#30701,#30702,#30703,#30704,#30705,#30706,#30707,#30708,#30709,
#30710,#30711,#30712,#30713,#30714,#30715,#30716,#30717,#30718,#30719,#30720,
#30721,#30722,#30723,#30724),.UNSPECIFIED.,.F.,.F.,(4,3,3,3,3,3,3,3,3,3,
3,3,3,3,3,3,3,3,3,3,3,4),(-0.976443208995993,-0.960629666524145,-0.949661288965092,
-0.931972270488238,-0.914398186942953,-0.904644103415597,-0.893317754842134,
-0.880493104971776,-0.86694095688213,-0.852605467987035,-0.837134239960094,
-0.82157385570267,-0.80614720579097,-0.791874660471043,-0.790720555879271,
-0.779060485592236,-0.740625,-0.691250000000001,-0.5925,-0.49375,-0.394999999999999,
-0.0499999999999998),.UNSPECIFIED.);
#3914=B_SPLINE_CURVE_WITH_KNOTS('',3,(#30916,#30917,#30918,#30919),
 .UNSPECIFIED.,.F.,.F.,(4,4),(-0.253410853624616,-0.103262412077186),
 .UNSPECIFIED.);
#3915=B_SPLINE_CURVE_WITH_KNOTS('',3,(#30921,#30922,#30923,#30924),
 .UNSPECIFIED.,.F.,.F.,(4,4),(0.,0.29),.UNSPECIFIED.);
#3916=B_SPLINE_CURVE_WITH_KNOTS('',3,(#30925,#30926,#30927,#30928),
 .UNSPECIFIED.,.F.,.F.,(4,4),(3.28350553743639,3.37607250339859),
 .UNSPECIFIED.);
#3917=B_SPLINE_CURVE_WITH_KNOTS('',3,(#30930,#30931,#30932,#30933,#30934,
#30935),.UNSPECIFIED.,.F.,.F.,(4,2,4),(-2.17700203273975,-1.38478587807843,
-0.288632999074766),.UNSPECIFIED.);
#3918=B_SPLINE_CURVE_WITH_KNOTS('',3,(#30937,#30938,#30939,#30940,#30941,
#30942,#30943,#30944,#30945,#30946,#30947,#30948,#30949,#30950,#30951,#30952,
#30953,#30954,#30955,#30956,#30957,#30958,#30959,#30960,#30961,#30962,#30963,
#30964,#30965,#30966,#30967),.UNSPECIFIED.,.F.,.F.,(4,3,3,3,3,3,3,3,3,3,
4),(0.664704897780732,0.688351938092992,0.780317238696445,0.810486879810963,
0.862717972416636,0.955520663501275,1.01466394039967,1.06038302616807,1.10529572457683,
1.13272802062135,1.20216888729732),.UNSPECIFIED.);
#3919=B_SPLINE_CURVE_WITH_KNOTS('',3,(#30968,#30969,#30970,#30971,#30972,
#30973,#30974,#30975,#30976,#30977,#30978,#30979,#30980,#30981,#30982,#30983,
#30984,#30985,#30986),.UNSPECIFIED.,.F.,.F.,(4,3,3,3,3,3,4),(0.,0.178790961538472,
0.350742859481108,0.449205432353047,0.513879914408646,0.522694757423744,
0.664704897780732),.UNSPECIFIED.);
#3920=B_SPLINE_CURVE_WITH_KNOTS('',3,(#30990,#30991,#30992,#30993),
 .UNSPECIFIED.,.F.,.F.,(4,4),(-0.0707400283123018,0.),.UNSPECIFIED.);
#3921=B_SPLINE_CURVE_WITH_KNOTS('',3,(#30997,#30998,#30999,#31000),
 .UNSPECIFIED.,.F.,.F.,(4,4),(-0.0707432952234936,-3.34525766215732E-6),
 .UNSPECIFIED.);
#3922=B_SPLINE_CURVE_WITH_KNOTS('',3,(#31004,#31005,#31006,#31007,#31008,
#31009,#31010,#31011,#31012,#31013,#31014,#31015,#31016,#31017,#31018,#31019,
#31020,#31021,#31022,#31023,#31024,#31025,#31026,#31027,#31028,#31029,#31030,
#31031,#31032,#31033,#31034,#31035,#31036,#31037,#31038,#31039,#31040,#31041,
#31042,#31043,#31044,#31045,#31046,#31047,#31048,#31049,#31050,#31051,#31052,
#31053,#31054,#31055,#31056,#31057,#31058,#31059,#31060,#31061,#31062,#31063,
#31064,#31065,#31066,#31067,#31068,#31069,#31070,#31071,#31072,#31073,#31074,
#31075,#31076,#31077,#31078,#31079,#31080,#31081,#31082,#31083,#31084,#31085,
#31086,#31087,#31088,#31089,#31090,#31091,#31092,#31093,#31094,#31095,#31096,
#31097,#31098,#31099,#31100),.UNSPECIFIED.,.F.,.F.,(4,3,3,3,3,3,3,3,3,3,
3,3,3,3,3,3,3,3,3,3,3,3,3,3,3,3,3,3,3,3,3,3,4),(-0.461463988274541,-0.386087506167661,
-0.372903671306323,-0.36421409612757,-0.349922618618653,-0.338448280177947,
-0.328550793223542,-0.322977024945215,-0.314822638010335,-0.306007155782303,
-0.304885949019545,-0.297658439870374,-0.289754515056093,-0.282882239837598,
-0.277393071545029,-0.271439067306369,-0.265165133453971,-0.258272116803451,
-0.254459737762025,-0.242193625916564,-0.228473458862565,-0.21371747313048,
-0.197852099811482,-0.180468088683521,-0.162567602548332,-0.144906258985007,
-0.134249918117004,-0.102205018832849,-0.0696974934620405,-0.0525746845214139,
-0.0222228841287436,-0.000827460244363642,0.),.UNSPECIFIED.);
#3923=B_SPLINE_CURVE_WITH_KNOTS('',3,(#31103,#31104,#31105,#31106,#31107,
#31108,#31109,#31110,#31111,#31112,#31113,#31114,#31115,#31116,#31117,#31118,
#31119,#31120,#31121,#31122,#31123,#31124,#31125,#31126,#31127,#31128,#31129,
#31130,#31131,#31132,#31133,#31134,#31135,#31136,#31137,#31138,#31139,#31140,
#31141,#31142,#31143,#31144,#31145,#31146,#31147,#31148,#31149,#31150,#31151,
#31152,#31153,#31154,#31155,#31156,#31157,#31158,#31159,#31160,#31161,#31162,
#31163,#31164,#31165,#31166),.UNSPECIFIED.,.F.,.F.,(4,3,3,3,3,3,3,3,3,3,
3,3,3,3,3,3,3,3,3,3,3,4),(-0.976443208995993,-0.960628704721019,-0.949661288965092,
-0.931975105549617,-0.914400310860108,-0.904644103415597,-0.893320015681313,
-0.880495083206057,-0.866943636882841,-0.852607981525343,-0.837136125113825,
-0.821574066139019,-0.806147311009145,-0.791872999074882,-0.790720555879271,
-0.779060485592236,-0.740625,-0.691250000000001,-0.5925,-0.49375,-0.394999999999999,
-0.0499999999999998),.UNSPECIFIED.);
#3924=B_SPLINE_CURVE_WITH_KNOTS('',3,(#31388,#31389,#31390,#31391),
 .UNSPECIFIED.,.F.,.F.,(4,4),(-0.253410853624616,-0.103262412077186),
 .UNSPECIFIED.);
#3925=B_SPLINE_CURVE_WITH_KNOTS('',3,(#31393,#31394,#31395,#31396),
 .UNSPECIFIED.,.F.,.F.,(4,4),(0.,0.29),.UNSPECIFIED.);
#3926=B_SPLINE_CURVE_WITH_KNOTS('',3,(#31397,#31398,#31399,#31400),
 .UNSPECIFIED.,.F.,.F.,(4,4),(3.2835055364322,3.37607250233925),
 .UNSPECIFIED.);
#3927=B_SPLINE_CURVE_WITH_KNOTS('',3,(#31402,#31403,#31404,#31405,#31406,
#31407),.UNSPECIFIED.,.F.,.F.,(4,2,4),(-2.17700203273975,-1.38478587807843,
-0.288632999074765),.UNSPECIFIED.);
#3928=B_SPLINE_CURVE_WITH_KNOTS('',3,(#31409,#31410,#31411,#31412,#31413,
#31414,#31415,#31416,#31417,#31418,#31419,#31420,#31421,#31422,#31423,#31424,
#31425,#31426,#31427,#31428,#31429,#31430,#31431,#31432,#31433,#31434,#31435,
#31436,#31437,#31438,#31439),.UNSPECIFIED.,.F.,.F.,(4,3,3,3,3,3,3,3,3,3,
4),(0.664704897780732,0.688351938092992,0.780317238696455,0.810486879810963,
0.86271797241663,0.955520663501275,1.0146639403996,1.06038302616807,1.10529572457683,
1.13272802062135,1.20216888729732),.UNSPECIFIED.);
#3929=B_SPLINE_CURVE_WITH_KNOTS('',3,(#31440,#31441,#31442,#31443,#31444,
#31445,#31446,#31447,#31448,#31449,#31450,#31451,#31452,#31453,#31454,#31455,
#31456,#31457,#31458),.UNSPECIFIED.,.F.,.F.,(4,3,3,3,3,3,4),(0.,0.178790961538472,
0.350742859481108,0.449205432353048,0.513879914408647,0.522694757423744,
0.664704897780732),.UNSPECIFIED.);
#3930=B_SPLINE_CURVE_WITH_KNOTS('',3,(#31462,#31463,#31464,#31465),
 .UNSPECIFIED.,.F.,.F.,(4,4),(-0.070740028238931,0.),.UNSPECIFIED.);
#3931=B_SPLINE_CURVE_WITH_KNOTS('',3,(#31469,#31470,#31471,#31472),
 .UNSPECIFIED.,.F.,.F.,(4,4),(-0.0707432954463844,-3.34525766251814E-6),
 .UNSPECIFIED.);
#3932=B_SPLINE_CURVE_WITH_KNOTS('',3,(#31476,#31477,#31478,#31479,#31480,
#31481,#31482,#31483,#31484,#31485,#31486,#31487,#31488,#31489,#31490,#31491,
#31492,#31493,#31494,#31495,#31496,#31497,#31498,#31499,#31500,#31501,#31502,
#31503,#31504,#31505,#31506,#31507,#31508,#31509,#31510,#31511,#31512,#31513,
#31514,#31515,#31516,#31517,#31518,#31519,#31520,#31521,#31522,#31523,#31524,
#31525,#31526,#31527,#31528,#31529,#31530,#31531,#31532,#31533,#31534,#31535,
#31536,#31537,#31538,#31539,#31540,#31541,#31542,#31543,#31544,#31545,#31546,
#31547,#31548,#31549,#31550,#31551,#31552,#31553,#31554,#31555,#31556,#31557,
#31558,#31559,#31560,#31561,#31562,#31563,#31564,#31565,#31566,#31567,#31568,
#31569,#31570,#31571,#31572),.UNSPECIFIED.,.F.,.F.,(4,3,3,3,3,3,3,3,3,3,
3,3,3,3,3,3,3,3,3,3,3,3,3,3,3,3,3,3,3,3,3,3,4),(-0.461463988274541,-0.386087506167661,
-0.375299929924104,-0.372903671306323,-0.356067397506652,-0.352040116130794,
-0.339910821414875,-0.338448280177947,-0.326626118627217,-0.313191280956895,
-0.304885949019545,-0.29982124014814,-0.293951934878654,-0.287657824438721,
-0.282882239837598,-0.277506987555355,-0.271688793715204,-0.265571314353823,
-0.258867937821342,-0.254459737762025,-0.241918476962302,-0.227823327163533,
-0.21260498793569,-0.196185493994907,-0.178200253731108,-0.159753497644407,
-0.141759381819153,-0.134249918117004,-0.101233746097596,-0.0682163658997657,
-0.0525746845214139,-0.024519300953322,0.),.UNSPECIFIED.);
#3933=B_SPLINE_CURVE_WITH_KNOTS('',3,(#31575,#31576,#31577,#31578,#31579,
#31580,#31581,#31582,#31583,#31584,#31585,#31586,#31587,#31588,#31589,#31590,
#31591,#31592,#31593,#31594,#31595,#31596,#31597,#31598,#31599,#31600,#31601,
#31602,#31603,#31604,#31605,#31606,#31607,#31608,#31609,#31610,#31611,#31612,
#31613,#31614,#31615,#31616,#31617,#31618,#31619,#31620,#31621,#31622,#31623,
#31624,#31625,#31626,#31627,#31628,#31629,#31630,#31631,#31632,#31633,#31634,
#31635,#31636,#31637,#31638),.UNSPECIFIED.,.F.,.F.,(4,3,3,3,3,3,3,3,3,3,
3,3,3,3,3,3,3,3,3,3,3,4),(-0.976443208995993,-0.959641771463709,-0.949661288965092,
-0.932500795758733,-0.914975318861593,-0.904644103415597,-0.893689140152816,
-0.881835075865263,-0.86859336767701,-0.854447019507575,-0.839440732702475,
-0.823698475329622,-0.808085046250136,-0.793464970994181,-0.790720555879271,
-0.779060485592236,-0.740625,-0.691250000000001,-0.5925,-0.543125,-0.394999999999999,
-0.0499999999999998),.UNSPECIFIED.);
#3934=B_SPLINE_CURVE_WITH_KNOTS('',3,(#31850,#31851,#31852,#31853),
 .UNSPECIFIED.,.F.,.F.,(4,4),(-0.253410853624616,-0.103262412077185),
 .UNSPECIFIED.);
#3935=B_SPLINE_CURVE_WITH_KNOTS('',3,(#31855,#31856,#31857,#31858),
 .UNSPECIFIED.,.F.,.F.,(4,4),(0.,0.29),.UNSPECIFIED.);
#3936=B_SPLINE_CURVE_WITH_KNOTS('',3,(#31859,#31860,#31861,#31862),
 .UNSPECIFIED.,.F.,.F.,(4,4),(3.28350553681631,3.37607250273892),
 .UNSPECIFIED.);
#3937=B_SPLINE_CURVE_WITH_KNOTS('',3,(#31864,#31865,#31866,#31867,#31868,
#31869),.UNSPECIFIED.,.F.,.F.,(4,2,4),(-2.17700203273975,-1.38478587807843,
-0.288632999074765),.UNSPECIFIED.);
#3938=B_SPLINE_CURVE_WITH_KNOTS('',3,(#31871,#31872,#31873,#31874,#31875,
#31876,#31877,#31878,#31879,#31880,#31881,#31882,#31883,#31884,#31885,#31886,
#31887,#31888,#31889,#31890,#31891,#31892,#31893,#31894,#31895,#31896,#31897,
#31898,#31899,#31900,#31901),.UNSPECIFIED.,.F.,.F.,(4,3,3,3,3,3,3,3,3,3,
4),(0.664704897780732,0.688351938092992,0.780317238696435,0.810486879810963,
0.862717972416624,0.955520663501275,1.01466394039955,1.06038302616807,1.10529572457683,
1.13272802062135,1.20216888729732),.UNSPECIFIED.);
#3939=B_SPLINE_CURVE_WITH_KNOTS('',3,(#31902,#31903,#31904,#31905,#31906,
#31907,#31908,#31909,#31910,#31911,#31912,#31913,#31914,#31915,#31916,#31917,
#31918,#31919,#31920),.UNSPECIFIED.,.F.,.F.,(4,3,3,3,3,3,4),(0.,0.178790961538472,
0.350742859481108,0.449205432353047,0.513879914408646,0.522694757423744,
0.664704897780732),.UNSPECIFIED.);
#3940=B_SPLINE_CURVE_WITH_KNOTS('',3,(#31924,#31925,#31926,#31927),
 .UNSPECIFIED.,.F.,.F.,(4,4),(-0.0707400282745222,0.),.UNSPECIFIED.);
#3941=B_SPLINE_CURVE_WITH_KNOTS('',3,(#31931,#31932,#31933,#31934),
 .UNSPECIFIED.,.F.,.F.,(4,4),(-0.0707432948552679,-3.34525766382265E-6),
 .UNSPECIFIED.);
#3942=B_SPLINE_CURVE_WITH_KNOTS('',3,(#31938,#31939,#31940,#31941,#31942,
#31943,#31944,#31945,#31946,#31947,#31948,#31949,#31950,#31951,#31952,#31953,
#31954,#31955,#31956,#31957,#31958,#31959,#31960,#31961,#31962,#31963,#31964,
#31965,#31966,#31967,#31968,#31969,#31970,#31971,#31972,#31973,#31974,#31975,
#31976,#31977,#31978,#31979,#31980,#31981,#31982,#31983,#31984,#31985,#31986,
#31987,#31988,#31989,#31990,#31991,#31992,#31993,#31994,#31995,#31996,#31997,
#31998,#31999,#32000,#32001,#32002,#32003,#32004,#32005,#32006,#32007,#32008,
#32009,#32010,#32011,#32012,#32013,#32014,#32015,#32016,#32017,#32018,#32019,
#32020,#32021,#32022,#32023,#32024,#32025,#32026,#32027,#32028),
 .UNSPECIFIED.,.F.,.F.,(4,3,3,3,3,3,3,3,3,3,3,3,3,3,3,3,3,3,3,3,3,3,3,3,
3,3,3,3,3,3,4),(-0.461463988274541,-0.386087506167661,-0.372903671306323,
-0.36421409612757,-0.352528758081246,-0.339636892135942,-0.338448280177947,
-0.328074919236012,-0.316383789572667,-0.304885949019545,-0.297243973048271,
-0.288858567477107,-0.282882239837598,-0.277347677282806,-0.271340988166504,
-0.265007390818465,-0.25804485249077,-0.254459737762025,-0.242044020405011,
-0.228141105146492,-0.213185106576009,-0.197120884701566,-0.179636878474647,
-0.161760929349303,-0.144350238406463,-0.134249918117004,-0.102125955921642,
-0.0702664487997433,-0.0525746845214139,-0.0216606650153897,0.),
 .UNSPECIFIED.);
#3943=B_SPLINE_CURVE_WITH_KNOTS('',3,(#32031,#32032,#32033,#32034,#32035,
#32036,#32037,#32038,#32039,#32040,#32041,#32042,#32043,#32044,#32045,#32046,
#32047,#32048,#32049,#32050,#32051,#32052,#32053,#32054,#32055,#32056,#32057,
#32058,#32059,#32060,#32061,#32062,#32063,#32064,#32065,#32066,#32067,#32068,
#32069,#32070,#32071,#32072,#32073,#32074,#32075,#32076,#32077,#32078,#32079,
#32080,#32081,#32082,#32083,#32084,#32085,#32086,#32087,#32088,#32089,#32090,
#32091,#32092,#32093,#32094),.UNSPECIFIED.,.F.,.F.,(4,3,3,3,3,3,3,3,3,3,
3,3,3,3,3,3,3,3,3,3,3,4),(-0.976443208995993,-0.960629666524143,-0.949661288965092,
-0.931972270488239,-0.91439818694386,-0.904644103415597,-0.893317754842135,
-0.880493104971777,-0.866940956882102,-0.852605467987185,-0.837134239960207,
-0.821573855702639,-0.806147205790955,-0.791874660471242,-0.790720555879271,
-0.779060485592236,-0.740625,-0.691250000000001,-0.5925,-0.49375,-0.394999999999999,
-0.0499999999999998),.UNSPECIFIED.);
#3944=B_SPLINE_CURVE_WITH_KNOTS('',3,(#32286,#32287,#32288,#32289),
 .UNSPECIFIED.,.F.,.F.,(4,4),(-0.253410853624616,-0.103262412077186),
 .UNSPECIFIED.);
#3945=B_SPLINE_CURVE_WITH_KNOTS('',3,(#32291,#32292,#32293,#32294),
 .UNSPECIFIED.,.F.,.F.,(4,4),(0.,0.29),.UNSPECIFIED.);
#3946=B_SPLINE_CURVE_WITH_KNOTS('',3,(#32295,#32296,#32297,#32298),
 .UNSPECIFIED.,.F.,.F.,(4,4),(3.28350553629102,3.37607250219087),
 .UNSPECIFIED.);
#3947=B_SPLINE_CURVE_WITH_KNOTS('',3,(#32300,#32301,#32302,#32303,#32304,
#32305),.UNSPECIFIED.,.F.,.F.,(4,2,4),(-2.17700203273975,-1.38478587807843,
-0.288632999074765),.UNSPECIFIED.);
#3948=B_SPLINE_CURVE_WITH_KNOTS('',3,(#32307,#32308,#32309,#32310,#32311,
#32312,#32313,#32314,#32315,#32316,#32317,#32318,#32319,#32320,#32321,#32322,
#32323,#32324,#32325,#32326,#32327,#32328,#32329,#32330,#32331,#32332,#32333,
#32334,#32335,#32336,#32337),.UNSPECIFIED.,.F.,.F.,(4,3,3,3,3,3,3,3,3,3,
4),(0.664704897780732,0.688351938092992,0.780317238696413,0.810486879810963,
0.862717972416625,0.955520663501275,1.01466394039958,1.06038302616807,1.10529572457683,
1.13272802062135,1.20216888729732),.UNSPECIFIED.);
#3949=B_SPLINE_CURVE_WITH_KNOTS('',3,(#32338,#32339,#32340,#32341,#32342,
#32343,#32344,#32345,#32346,#32347,#32348,#32349,#32350,#32351,#32352,#32353,
#32354,#32355,#32356),.UNSPECIFIED.,.F.,.F.,(4,3,3,3,3,3,4),(0.,0.178790961538472,
0.350742859481108,0.449205432353047,0.513879914408646,0.522694757423744,
0.664704897780732),.UNSPECIFIED.);
#3950=B_SPLINE_CURVE_WITH_KNOTS('',3,(#32360,#32361,#32362,#32363),
 .UNSPECIFIED.,.F.,.F.,(4,4),(-0.0707400283126209,0.),.UNSPECIFIED.);
#3951=B_SPLINE_CURVE_WITH_KNOTS('',3,(#32367,#32368,#32369,#32370),
 .UNSPECIFIED.,.F.,.F.,(4,4),(-0.0707432952233519,-3.34525766214344E-6),
 .UNSPECIFIED.);
#3952=B_SPLINE_CURVE_WITH_KNOTS('',3,(#32374,#32375,#32376,#32377,#32378,
#32379,#32380,#32381,#32382,#32383,#32384,#32385,#32386,#32387,#32388,#32389,
#32390,#32391,#32392,#32393,#32394,#32395,#32396,#32397,#32398,#32399,#32400,
#32401,#32402,#32403,#32404,#32405,#32406,#32407,#32408,#32409,#32410,#32411,
#32412,#32413,#32414,#32415,#32416,#32417,#32418,#32419,#32420,#32421,#32422,
#32423,#32424,#32425,#32426,#32427,#32428,#32429,#32430,#32431,#32432,#32433,
#32434,#32435,#32436,#32437,#32438,#32439,#32440,#32441,#32442,#32443,#32444,
#32445,#32446,#32447,#32448,#32449,#32450,#32451,#32452,#32453,#32454,#32455,
#32456,#32457,#32458,#32459,#32460,#32461,#32462,#32463,#32464,#32465,#32466,
#32467,#32468,#32469,#32470),.UNSPECIFIED.,.F.,.F.,(4,3,3,3,3,3,3,3,3,3,
3,3,3,3,3,3,3,3,3,3,3,3,3,3,3,3,3,3,3,3,3,3,4),(-0.461463988274541,-0.386087506167661,
-0.372903671306323,-0.36421409612757,-0.349922618627965,-0.338448280177947,
-0.328550793223787,-0.322977024945215,-0.314822638010135,-0.306007155781965,
-0.304885949019545,-0.297658439870209,-0.289754515055766,-0.282882239837598,
-0.277393071544918,-0.271439067306178,-0.265165133453712,-0.258272116803191,
-0.254459737762025,-0.242193625915922,-0.228473458861454,-0.213717473128992,
-0.197852099810461,-0.180468088688012,-0.162567602565365,-0.144906259020509,
-0.134249918117004,-0.102205019200821,-0.069697494513509,-0.0525746845214139,
-0.0222228838221762,-0.000827460244363642,0.),.UNSPECIFIED.);
#3953=B_SPLINE_CURVE_WITH_KNOTS('',3,(#32473,#32474,#32475,#32476,#32477,
#32478,#32479,#32480,#32481,#32482,#32483,#32484,#32485,#32486,#32487,#32488,
#32489,#32490,#32491,#32492,#32493,#32494,#32495,#32496,#32497,#32498,#32499,
#32500,#32501,#32502,#32503,#32504,#32505,#32506,#32507,#32508,#32509,#32510,
#32511,#32512,#32513,#32514,#32515,#32516,#32517,#32518,#32519,#32520,#32521,
#32522,#32523,#32524,#32525,#32526,#32527,#32528,#32529,#32530,#32531,#32532,
#32533,#32534,#32535,#32536),.UNSPECIFIED.,.F.,.F.,(4,3,3,3,3,3,3,3,3,3,
3,3,3,3,3,3,3,3,3,3,3,4),(-0.976443208995993,-0.960628704721016,-0.949661288965092,
-0.931975105549621,-0.914400310859732,-0.904644103415597,-0.893320015681319,
-0.880495083206063,-0.866943636882833,-0.852607981525122,-0.837136125113659,
-0.821574066138669,-0.80614731100897,-0.791872999074531,-0.790720555879271,
-0.779060485592236,-0.740625,-0.691250000000001,-0.5925,-0.49375,-0.394999999999999,
-0.0499999999999998),.UNSPECIFIED.);
#3954=B_SPLINE_CURVE_WITH_KNOTS('',3,(#32758,#32759,#32760,#32761),
 .UNSPECIFIED.,.F.,.F.,(4,4),(-0.253410853624616,-0.103262412077186),
 .UNSPECIFIED.);
#3955=B_SPLINE_CURVE_WITH_KNOTS('',3,(#32763,#32764,#32765,#32766),
 .UNSPECIFIED.,.F.,.F.,(4,4),(0.,0.29),.UNSPECIFIED.);
#3956=B_SPLINE_CURVE_WITH_KNOTS('',3,(#32767,#32768,#32769,#32770),
 .UNSPECIFIED.,.F.,.F.,(4,4),(3.28350553791586,3.3760725039151),
 .UNSPECIFIED.);
#3957=B_SPLINE_CURVE_WITH_KNOTS('',3,(#32772,#32773,#32774,#32775,#32776,
#32777),.UNSPECIFIED.,.F.,.F.,(4,2,4),(-2.17700203273975,-1.38478587807843,
-0.288632999074766),.UNSPECIFIED.);
#3958=B_SPLINE_CURVE_WITH_KNOTS('',3,(#32779,#32780,#32781,#32782,#32783,
#32784,#32785,#32786,#32787,#32788,#32789,#32790,#32791,#32792,#32793,#32794,
#32795,#32796,#32797,#32798,#32799,#32800,#32801,#32802,#32803,#32804,#32805,
#32806,#32807,#32808,#32809),.UNSPECIFIED.,.F.,.F.,(4,3,3,3,3,3,3,3,3,3,
4),(0.664704897780732,0.688351938092992,0.780317238696449,0.810486879810963,
0.862717972416621,0.955520663501275,1.0146639403996,1.06038302616807,1.10529572457683,
1.13272802062135,1.20216888729732),.UNSPECIFIED.);
#3959=B_SPLINE_CURVE_WITH_KNOTS('',3,(#32810,#32811,#32812,#32813,#32814,
#32815,#32816,#32817,#32818,#32819,#32820,#32821,#32822,#32823,#32824,#32825,
#32826,#32827,#32828),.UNSPECIFIED.,.F.,.F.,(4,3,3,3,3,3,4),(0.,0.178790961538472,
0.350742859481108,0.449205432353048,0.513879914408647,0.522694757423744,
0.664704897780732),.UNSPECIFIED.);
#3960=B_SPLINE_CURVE_WITH_KNOTS('',3,(#32874,#32875,#32876,#32877),
 .UNSPECIFIED.,.F.,.F.,(4,4),(3.77373852169387,3.81785134154664),
 .UNSPECIFIED.);
#3961=B_SPLINE_CURVE_WITH_KNOTS('',3,(#32881,#32882,#32883,#32884),
 .UNSPECIFIED.,.F.,.F.,(4,4),(1.38212585516677,1.42567867406759),
 .UNSPECIFIED.);
#3962=B_SPLINE_CURVE_WITH_KNOTS('',3,(#32898,#32899,#32900,#32901),
 .UNSPECIFIED.,.F.,.F.,(4,4),(1.38212585516678,1.42567867432177),
 .UNSPECIFIED.);
#3963=B_SPLINE_CURVE_WITH_KNOTS('',3,(#32908,#32909,#32910,#32911),
 .UNSPECIFIED.,.F.,.F.,(4,4),(0.,0.29),.UNSPECIFIED.);
#3964=B_SPLINE_CURVE_WITH_KNOTS('',3,(#32933,#32934,#32935,#32936),
 .UNSPECIFIED.,.F.,.F.,(4,4),(3.77373852169387,3.81785134154665),
 .UNSPECIFIED.);
#3965=B_SPLINE_CURVE_WITH_KNOTS('',3,(#32958,#32959,#32960,#32961),
 .UNSPECIFIED.,.F.,.F.,(4,4),(1.38212585516677,1.42567867432177),
 .UNSPECIFIED.);
#3966=B_SPLINE_CURVE_WITH_KNOTS('',3,(#32968,#32969,#32970,#32971),
 .UNSPECIFIED.,.F.,.F.,(4,4),(0.,0.29),.UNSPECIFIED.);
#3967=B_SPLINE_CURVE_WITH_KNOTS('',3,(#32993,#32994,#32995,#32996),
 .UNSPECIFIED.,.F.,.F.,(4,4),(3.77373852169387,3.81785134154664),
 .UNSPECIFIED.);
#3968=B_SPLINE_CURVE_WITH_KNOTS('',3,(#33018,#33019,#33020,#33021),
 .UNSPECIFIED.,.F.,.F.,(4,4),(1.38212585516678,1.42567867432177),
 .UNSPECIFIED.);
#3969=B_SPLINE_CURVE_WITH_KNOTS('',3,(#33028,#33029,#33030,#33031),
 .UNSPECIFIED.,.F.,.F.,(4,4),(0.,0.29),.UNSPECIFIED.);
#3970=B_SPLINE_CURVE_WITH_KNOTS('',3,(#33053,#33054,#33055,#33056),
 .UNSPECIFIED.,.F.,.F.,(4,4),(3.77373852169387,3.81785134154664),
 .UNSPECIFIED.);
#3971=B_SPLINE_CURVE_WITH_KNOTS('',3,(#33078,#33079,#33080,#33081),
 .UNSPECIFIED.,.F.,.F.,(4,4),(1.38212585516677,1.42567867432177),
 .UNSPECIFIED.);
#3972=B_SPLINE_CURVE_WITH_KNOTS('',3,(#33088,#33089,#33090,#33091),
 .UNSPECIFIED.,.F.,.F.,(4,4),(0.,0.29),.UNSPECIFIED.);
#3973=B_SPLINE_CURVE_WITH_KNOTS('',3,(#33113,#33114,#33115,#33116),
 .UNSPECIFIED.,.F.,.F.,(4,4),(3.77373852169387,3.81785134154665),
 .UNSPECIFIED.);
#3974=B_SPLINE_CURVE_WITH_KNOTS('',3,(#33138,#33139,#33140,#33141),
 .UNSPECIFIED.,.F.,.F.,(4,4),(1.38212585516677,1.42567867432177),
 .UNSPECIFIED.);
#3975=B_SPLINE_CURVE_WITH_KNOTS('',3,(#33148,#33149,#33150,#33151),
 .UNSPECIFIED.,.F.,.F.,(4,4),(0.,0.29),.UNSPECIFIED.);
#3976=B_SPLINE_CURVE_WITH_KNOTS('',3,(#33173,#33174,#33175,#33176),
 .UNSPECIFIED.,.F.,.F.,(4,4),(3.77373866725656,3.81785134154664),
 .UNSPECIFIED.);
#3977=B_SPLINE_CURVE_WITH_KNOTS('',3,(#33217,#33218,#33219,#33220),
 .UNSPECIFIED.,.F.,.F.,(4,4),(1.38209974812346,1.42565252910459),
 .UNSPECIFIED.);
#3978=B_SPLINE_CURVE_WITH_KNOTS('',3,(#33230,#33231,#33232,#33233,#33234,
#33235),.UNSPECIFIED.,.F.,.F.,(4,2,4),(2.73646626801627,2.7475473717049,
2.77362936601305),.UNSPECIFIED.);
#3979=B_SPLINE_CURVE_WITH_KNOTS('',3,(#33237,#33238,#33239,#33240,#33241,
#33242),.UNSPECIFIED.,.F.,.F.,(4,2,4),(1.69951603755124,1.72559803185939,
1.73667913554802),.UNSPECIFIED.);
#3980=B_SPLINE_CURVE_WITH_KNOTS('',3,(#33246,#33247,#33248,#33249,#33250,
#33251),.UNSPECIFIED.,.F.,.F.,(4,2,4),(2.73646626800866,2.74754737169729,
2.77362936600545),.UNSPECIFIED.);
#3981=B_SPLINE_CURVE_WITH_KNOTS('',3,(#33253,#33254,#33255,#33256,#33257,
#33258),.UNSPECIFIED.,.F.,.F.,(4,2,4),(1.69951603754363,1.72559803185179,
1.73667913554042),.UNSPECIFIED.);
#3982=B_SPLINE_CURVE_WITH_KNOTS('',3,(#33274,#33275,#33276,#33277),
 .UNSPECIFIED.,.F.,.F.,(4,4),(0.,0.29),.UNSPECIFIED.);
#3983=B_SPLINE_CURVE_WITH_KNOTS('',3,(#33298,#33299,#33300,#33301),
 .UNSPECIFIED.,.F.,.F.,(4,4),(3.77373866725655,3.81785134154664),
 .UNSPECIFIED.);
#3984=B_SPLINE_CURVE_WITH_KNOTS('',3,(#33313,#33314,#33315,#33316),
 .UNSPECIFIED.,.F.,.F.,(4,4),(1.38209974812346,1.42565252910459),
 .UNSPECIFIED.);
#3985=B_SPLINE_CURVE_WITH_KNOTS('',3,(#33330,#33331,#33332,#33333),
 .UNSPECIFIED.,.F.,.F.,(4,4),(0.,0.29),.UNSPECIFIED.);
#3986=B_SPLINE_CURVE_WITH_KNOTS('',3,(#33354,#33355,#33356,#33357),
 .UNSPECIFIED.,.F.,.F.,(4,4),(3.77373866725655,3.81785134154664),
 .UNSPECIFIED.);
#3987=B_SPLINE_CURVE_WITH_KNOTS('',3,(#33369,#33370,#33371,#33372),
 .UNSPECIFIED.,.F.,.F.,(4,4),(1.38209974812346,1.42565252910459),
 .UNSPECIFIED.);
#3988=B_SPLINE_CURVE_WITH_KNOTS('',3,(#33386,#33387,#33388,#33389),
 .UNSPECIFIED.,.F.,.F.,(4,4),(0.,0.29),.UNSPECIFIED.);
#3989=B_SPLINE_CURVE_WITH_KNOTS('',3,(#33410,#33411,#33412,#33413),
 .UNSPECIFIED.,.F.,.F.,(4,4),(3.77373866725655,3.81785134154664),
 .UNSPECIFIED.);
#3990=B_SPLINE_CURVE_WITH_KNOTS('',3,(#33425,#33426,#33427,#33428),
 .UNSPECIFIED.,.F.,.F.,(4,4),(1.38209974812346,1.42565252910459),
 .UNSPECIFIED.);
#3991=B_SPLINE_CURVE_WITH_KNOTS('',3,(#33442,#33443,#33444,#33445),
 .UNSPECIFIED.,.F.,.F.,(4,4),(0.,0.29),.UNSPECIFIED.);
#3992=B_SPLINE_CURVE_WITH_KNOTS('',3,(#33466,#33467,#33468,#33469),
 .UNSPECIFIED.,.F.,.F.,(4,4),(3.77373866725655,3.81785134154664),
 .UNSPECIFIED.);
#3993=B_SPLINE_CURVE_WITH_KNOTS('',3,(#33481,#33482,#33483,#33484),
 .UNSPECIFIED.,.F.,.F.,(4,4),(1.38209974812346,1.42565252910459),
 .UNSPECIFIED.);
#3994=B_SPLINE_CURVE_WITH_KNOTS('',3,(#33498,#33499,#33500,#33501),
 .UNSPECIFIED.,.F.,.F.,(4,4),(0.,0.29),.UNSPECIFIED.);
#3995=B_SPLINE_CURVE_WITH_KNOTS('',3,(#33522,#33523,#33524,#33525),
 .UNSPECIFIED.,.F.,.F.,(4,4),(3.77373866725656,3.81785134154665),
 .UNSPECIFIED.);
#3996=B_SPLINE_CURVE_WITH_KNOTS('',3,(#33537,#33538,#33539,#33540),
 .UNSPECIFIED.,.F.,.F.,(4,4),(1.38209974812346,1.42565252910459),
 .UNSPECIFIED.);
#3997=B_SPLINE_CURVE_WITH_KNOTS('',3,(#33558,#33559,#33560,#33561),
 .UNSPECIFIED.,.F.,.F.,(4,4),(0.,0.29),.UNSPECIFIED.);
#3998=B_SPLINE_CURVE_WITH_KNOTS('',3,(#33565,#33566,#33567,#33568),
 .UNSPECIFIED.,.F.,.F.,(4,4),(3.77373866725655,3.81785134154664),
 .UNSPECIFIED.);
#3999=B_SPLINE_CURVE_WITH_KNOTS('',3,(#33577,#33578,#33579,#33580),
 .UNSPECIFIED.,.F.,.F.,(4,4),(0.,0.29),.UNSPECIFIED.);
#4000=B_SPLINE_CURVE_WITH_KNOTS('',3,(#33608,#33609,#33610,#33611,#33612,
#33613),.UNSPECIFIED.,.F.,.F.,(4,2,4),(1.69951603754749,1.72559803185564,
1.73667913554427),.UNSPECIFIED.);
#4001=B_SPLINE_CURVE_WITH_KNOTS('',3,(#33617,#33618,#33619,#33620,#33621,
#33622),.UNSPECIFIED.,.F.,.F.,(4,2,4),(2.73646626801252,2.74754737170115,
2.7736293660093),.UNSPECIFIED.);
#4002=B_SPLINE_CURVE_WITH_KNOTS('',3,(#33624,#33625,#33626,#33627),
 .UNSPECIFIED.,.F.,.F.,(4,4),(-0.123345114071782,0.),.UNSPECIFIED.);
#4003=B_SPLINE_CURVE_WITH_KNOTS('',3,(#33630,#33631,#33632,#33633),
 .UNSPECIFIED.,.F.,.F.,(4,4),(-0.123320533354397,0.),.UNSPECIFIED.);
#4004=B_SPLINE_CURVE_WITH_KNOTS('',3,(#33636,#33637,#33638,#33639,#33640,
#33641,#33642,#33643,#33644,#33645,#33646,#33647,#33648,#33649,#33650,#33651,
#33652,#33653,#33654,#33655,#33656,#33657,#33658,#33659,#33660,#33661,#33662,
#33663,#33664,#33665,#33666,#33667,#33668,#33669,#33670,#33671,#33672,#33673,
#33674,#33675,#33676,#33677,#33678,#33679,#33680,#33681,#33682,#33683,#33684,
#33685,#33686,#33687,#33688,#33689,#33690,#33691,#33692,#33693,#33694,#33695,
#33696,#33697,#33698,#33699,#33700,#33701,#33702,#33703,#33704,#33705,#33706,
#33707,#33708,#33709,#33710,#33711,#33712,#33713,#33714,#33715,#33716,#33717,
#33718,#33719,#33720,#33721,#33722,#33723,#33724,#33725,#33726,#33727,#33728,
#33729),.UNSPECIFIED.,.F.,.F.,(4,3,3,3,3,3,3,3,3,3,3,3,3,3,3,3,3,3,3,3,
3,3,3,3,3,3,3,3,3,3,3,4),(-0.658260979006731,-0.633773279162244,-0.605111071598155,
-0.587935823275639,-0.58215389072593,-0.576676348727153,-0.545880192440996,
-0.518933555690609,-0.50528736116522,-0.500250745725887,-0.469731699052497,
-0.438742337954577,-0.407896515574978,-0.388499161290708,-0.383813915666766,
-0.379411229252426,-0.347601178358055,-0.330307098437898,-0.29950598700594,
-0.268122067677042,-0.260223722040077,-0.255500332123237,-0.223562790607832,
-0.191212812564609,-0.158617534984855,-0.138790343111748,-0.132403685477666,
-0.127529513558128,-0.0941940108532412,-0.0608372923199841,-0.0281712614885087,
0.),.UNSPECIFIED.);
#4005=B_SPLINE_CURVE_WITH_KNOTS('',3,(#33734,#33735,#33736,#33737,#33738,
#33739,#33740,#33741,#33742,#33743,#33744,#33745,#33746,#33747,#33748,#33749,
#33750,#33751,#33752,#33753,#33754,#33755,#33756,#33757,#33758,#33759,#33760,
#33761,#33762,#33763,#33764,#33765,#33766,#33767,#33768,#33769,#33770,#33771,
#33772,#33773,#33774,#33775,#33776,#33777,#33778,#33779,#33780,#33781,#33782,
#33783,#33784,#33785,#33786,#33787,#33788,#33789,#33790,#33791,#33792,#33793,
#33794,#33795,#33796,#33797,#33798,#33799,#33800,#33801,#33802,#33803,#33804,
#33805,#33806,#33807,#33808,#33809,#33810,#33811,#33812,#33813,#33814,#33815,
#33816,#33817,#33818,#33819,#33820,#33821,#33822,#33823,#33824,#33825,#33826,
#33827,#33828,#33829,#33830),.UNSPECIFIED.,.F.,.F.,(4,3,3,3,3,3,3,3,3,3,
3,3,3,3,3,3,3,3,3,3,3,3,3,3,3,3,3,3,3,3,3,3,4),(-0.655752415918347,-0.626851741040676,
-0.59369504602698,-0.575358814455742,-0.568230237621974,-0.56261560332179,
-0.529721437610406,-0.501045675520003,-0.488500029605451,-0.480121961098349,
-0.475419822411446,-0.443204075940068,-0.411200944373518,-0.380156597583109,
-0.360196283409126,-0.353873717113103,-0.349018195039205,-0.318315352453775,
-0.300315340887177,-0.269060639454171,-0.237672628214141,-0.231826094134014,
-0.227181047726769,-0.196613620435523,-0.166002976183476,-0.135781765031655,
-0.118809044402698,-0.114031241820972,-0.109476336553635,-0.0799052018350452,
-0.0507571470011222,-0.022522284006719,0.),.UNSPECIFIED.);
#4006=B_SPLINE_CURVE_WITH_KNOTS('',3,(#34259,#34260,#34261,#34262,#34263,
#34264,#34265,#34266,#34267,#34268,#34269,#34270,#34271,#34272,#34273,#34274,
#34275,#34276,#34277),.UNSPECIFIED.,.F.,.F.,(4,3,3,3,3,3,4),(95.3641731163798,
96.2028589542983,97.1946410053736,98.1864230564488,99.1782051075241,100.169987158599,
101.077602036598),.UNSPECIFIED.);
#4007=B_SPLINE_CURVE_WITH_KNOTS('',3,(#34279,#34280,#34281,#34282,#34283,
#34284,#34285,#34286,#34287,#34288,#34289,#34290,#34291,#34292,#34293,#34294,
#34295,#34296,#34297,#34298,#34299,#34300,#34301,#34302,#34303,#34304,#34305,
#34306,#34307,#34308,#34309,#34310,#34311,#34312,#34313,#34314,#34315,#34316,
#34317,#34318,#34319,#34320,#34321,#34322,#34323,#34324,#34325,#34326,#34327,
#34328,#34329,#34330,#34331,#34332,#34333,#34334,#34335,#34336,#34337,#34338,
#34339,#34340,#34341,#34342,#34343,#34344,#34345,#34346,#34347,#34348,#34349,
#34350,#34351,#34352,#34353,#34354,#34355,#34356,#34357,#34358,#34359,#34360,
#34361,#34362,#34363,#34364,#34365,#34366,#34367,#34368,#34369,#34370,#34371,
#34372),.UNSPECIFIED.,.F.,.F.,(4,3,3,3,3,3,3,3,3,3,3,3,3,3,3,3,3,3,3,3,
3,3,3,3,3,3,3,3,3,3,3,4),(-0.658260979006784,-0.633773279162306,-0.60511106550004,
-0.587935817558656,-0.582153877533815,-0.576676345808561,-0.545880189887229,
-0.518933553456064,-0.505287355660679,-0.500250742991463,-0.469731693480689,
-0.438742332174745,-0.407896509549881,-0.388499156771889,-0.383813916281054,
-0.37941122894066,-0.347601178541539,-0.33030709843791,-0.299505983293081,
-0.268122059993525,-0.260224018962276,-0.25550038819645,-0.223562839671894,
-0.191212858654853,-0.158617580462045,-0.13879038290429,-0.132403785254111,
-0.127529529765003,-0.0941940254338511,-0.060837309314193,-0.0281712889870458,
0.),.UNSPECIFIED.);
#4008=B_SPLINE_CURVE_WITH_KNOTS('',3,(#34373,#34374,#34375,#34376,#34377,
#34378,#34379,#34380,#34381),.UNSPECIFIED.,.F.,.F.,(4,1,1,1,1,1,4),(10.3761157273103,
11.2837306053091,12.2755126563843,13.2672947074596,14.2590767585348,15.25085880961,
15.7079632679489),.UNSPECIFIED.);
#4009=B_SPLINE_CURVE_WITH_KNOTS('',3,(#34387,#34388,#34389,#34390,#34391,
#34392,#34393,#34394,#34395,#34396,#34397,#34398,#34399,#34400,#34401,#34402,
#34403,#34404,#34405,#34406,#34407,#34408,#34409,#34410,#34411,#34412,#34413,
#34414,#34415,#34416,#34417,#34418,#34419,#34420,#34421,#34422,#34423,#34424,
#34425,#34426,#34427,#34428,#34429,#34430,#34431,#34432,#34433,#34434,#34435,
#34436,#34437,#34438,#34439,#34440,#34441,#34442,#34443,#34444,#34445,#34446,
#34447,#34448,#34449,#34450,#34451,#34452,#34453,#34454,#34455,#34456,#34457,
#34458,#34459,#34460,#34461,#34462,#34463,#34464,#34465,#34466,#34467,#34468,
#34469,#34470,#34471,#34472,#34473,#34474,#34475,#34476,#34477,#34478,#34479,
#34480,#34481,#34482,#34483),.UNSPECIFIED.,.F.,.F.,(4,3,3,3,3,3,3,3,3,3,
3,3,3,3,3,3,3,3,3,3,3,3,3,3,3,3,3,3,3,3,3,3,4),(-0.655752415918265,-0.626851741040643,
-0.593695046194504,-0.575358814612795,-0.568230240534389,-0.562615606353527,
-0.529721440557959,-0.501045678099109,-0.488500032023362,-0.480121968529048,
-0.475419837506024,-0.44320409140917,-0.411200962660038,-0.380156623791134,
-0.36019630306514,-0.353875988306761,-0.349018404483483,-0.318315565766959,
-0.300315340887157,-0.269060643749347,-0.237672631000559,-0.231826095923608,
-0.227181047488589,-0.196613622754405,-0.166002975418797,-0.135781755587927,
-0.118809036139436,-0.114031227885311,-0.109476333948085,-0.0799051921969754,
-0.0507571266588613,-0.0225222496686074,0.),.UNSPECIFIED.);
#4010=B_SPLINE_CURVE_WITH_KNOTS('',3,(#34486,#34487,#34488,#34489,#34490,
#34491,#34492,#34493),.UNSPECIFIED.,.F.,.F.,(4,1,1,1,1,4),(11.6150328478185,
12.6068148988938,13.598596949969,14.5903790010443,15.5821610521195,15.7079632679489),
 .UNSPECIFIED.);
#4011=B_SPLINE_CURVE_WITH_KNOTS('',3,(#34922,#34923,#34924,#34925,#34926,
#34927,#34928,#34929,#34930,#34931,#34932,#34933,#34934,#34935,#34936,#34937),
 .UNSPECIFIED.,.F.,.F.,(4,3,3,3,3,4),(-103.145333311825,-102.15355126075,
-101.161769209675,-100.169987158599,-99.1782051075241,-98.3407100278241),
 .UNSPECIFIED.);
#4012=B_SPLINE_CURVE_WITH_KNOTS('',3,(#34939,#34940,#34941,#34942,#34943,
#34944),.UNSPECIFIED.,.F.,.F.,(4,2,4),(-1.35394250197628,-0.852961572903344,
-0.599740178024191),.UNSPECIFIED.);
#4013=B_SPLINE_CURVE_WITH_KNOTS('',3,(#35217,#35218,#35219,#35220,#35221,
#35222,#35223,#35224,#35225,#35226,#35227,#35228,#35229,#35230,#35231,#35232,
#35233,#35234,#35235,#35236,#35237,#35238,#35239,#35240,#35241,#35242,#35243,
#35244,#35245,#35246,#35247,#35248,#35249,#35250,#35251,#35252,#35253,#35254,
#35255,#35256,#35257,#35258,#35259,#35260,#35261,#35262,#35263,#35264,#35265,
#35266,#35267,#35268,#35269,#35270,#35271,#35272,#35273,#35274,#35275,#35276,
#35277,#35278,#35279,#35280),.UNSPECIFIED.,.F.,.F.,(4,3,3,3,3,3,3,3,3,3,
3,3,3,3,3,3,3,3,3,3,3,4),(-12.8459374819259,-11.4794095531645,-10.7961455887838,
-10.3238102653841,-10.1128816244031,-9.79002513073258,-7.17546444804456,
-5.86818410670054,-5.21454393602854,-4.88772385069253,-4.68535987578927,
-4.56090376535653,-4.4207580398687,-3.48474489248014,-2.76035534391825,
-2.17493233268475,-1.74712655327371,-1.70292711374287,-1.28137423833841,
-0.996111179633922,-0.765912925479548,-0.621212683296683),.UNSPECIFIED.);
#4014=B_SPLINE_CURVE_WITH_KNOTS('',3,(#35282,#35283,#35284,#35285),
 .UNSPECIFIED.,.F.,.F.,(4,4),(0.258432097335974,0.335446700888131),
 .UNSPECIFIED.);
#4015=B_SPLINE_CURVE_WITH_KNOTS('',3,(#35289,#35290,#35291,#35292,#35293,
#35294),.UNSPECIFIED.,.F.,.F.,(4,2,4),(2.73646626800883,2.74754737169745,
2.77362936600561),.UNSPECIFIED.);
#4016=B_SPLINE_CURVE_WITH_KNOTS('',3,(#35295,#35296,#35297,#35298,#35299,
#35300),.UNSPECIFIED.,.F.,.F.,(4,2,4),(1.69951603754379,1.72559803185195,
1.73667913554058),.UNSPECIFIED.);
#4017=B_SPLINE_CURVE_WITH_KNOTS('',3,(#35302,#35303,#35304,#35305),
 .UNSPECIFIED.,.F.,.F.,(4,4),(0.258432097334697,0.335446700886078),
 .UNSPECIFIED.);
#4018=B_SPLINE_CURVE_WITH_KNOTS('',3,(#35310,#35311,#35312,#35313,#35314,
#35315),.UNSPECIFIED.,.F.,.F.,(4,2,4),(2.73646626801231,2.74754737170094,
2.77362936600909),.UNSPECIFIED.);
#4019=B_SPLINE_CURVE_WITH_KNOTS('',3,(#35316,#35317,#35318,#35319,#35320,
#35321),.UNSPECIFIED.,.F.,.F.,(4,2,4),(1.69951603754727,1.72559803185543,
1.73667913554406),.UNSPECIFIED.);
#4020=B_SPLINE_CURVE_WITH_KNOTS('',3,(#35323,#35324,#35325,#35326),
 .UNSPECIFIED.,.F.,.F.,(4,4),(0.258432097333565,0.335446700884273),
 .UNSPECIFIED.);
#4021=B_SPLINE_CURVE_WITH_KNOTS('',3,(#35331,#35332,#35333,#35334,#35335,
#35336),.UNSPECIFIED.,.F.,.F.,(4,2,4),(2.73646626800806,2.74754737169669,
2.77362936600484),.UNSPECIFIED.);
#4022=B_SPLINE_CURVE_WITH_KNOTS('',3,(#35337,#35338,#35339,#35340,#35341,
#35342),.UNSPECIFIED.,.F.,.F.,(4,2,4),(1.69951603754303,1.72559803185118,
1.73667913553981),.UNSPECIFIED.);
#4023=B_SPLINE_CURVE_WITH_KNOTS('',3,(#35344,#35345,#35346,#35347),
 .UNSPECIFIED.,.F.,.F.,(4,4),(0.258432097337429,0.335446700890448),
 .UNSPECIFIED.);
#4024=B_SPLINE_CURVE_WITH_KNOTS('',3,(#35352,#35353,#35354,#35355,#35356,
#35357),.UNSPECIFIED.,.F.,.F.,(4,2,4),(2.73646626800755,2.74754737169618,
2.77362936600433),.UNSPECIFIED.);
#4025=B_SPLINE_CURVE_WITH_KNOTS('',3,(#35358,#35359,#35360,#35361,#35362,
#35363),.UNSPECIFIED.,.F.,.F.,(4,2,4),(1.69951603754252,1.72559803185067,
1.7366791355393),.UNSPECIFIED.);
#4026=B_SPLINE_CURVE_WITH_KNOTS('',3,(#35365,#35366,#35367,#35368),
 .UNSPECIFIED.,.F.,.F.,(4,4),(0.258432097333234,0.335446700883742),
 .UNSPECIFIED.);
#4027=B_SPLINE_CURVE_WITH_KNOTS('',3,(#35373,#35374,#35375,#35376,#35377,
#35378),.UNSPECIFIED.,.F.,.F.,(4,2,4),(2.73646626801512,2.74754737170375,
2.77362936601191),.UNSPECIFIED.);
#4028=B_SPLINE_CURVE_WITH_KNOTS('',3,(#35379,#35380,#35381,#35382,#35383,
#35384),.UNSPECIFIED.,.F.,.F.,(4,2,4),(1.69951603755009,1.72559803185825,
1.73667913554687),.UNSPECIFIED.);
#4029=B_SPLINE_CURVE_WITH_KNOTS('',3,(#35386,#35387,#35388,#35389),
 .UNSPECIFIED.,.F.,.F.,(4,4),(0.258432097341974,0.335446700897715),
 .UNSPECIFIED.);
#4030=B_SPLINE_CURVE_WITH_KNOTS('',3,(#35394,#35395,#35396,#35397,#35398,
#35399),.UNSPECIFIED.,.F.,.F.,(4,2,4),(2.73646626801742,2.74754737170605,
2.7736293660142),.UNSPECIFIED.);
#4031=B_SPLINE_CURVE_WITH_KNOTS('',3,(#35400,#35401,#35402,#35403,#35404,
#35405),.UNSPECIFIED.,.F.,.F.,(4,2,4),(1.69951603755239,1.72559803186054,
1.73667913554917),.UNSPECIFIED.);
#4032=B_SPLINE_CURVE_WITH_KNOTS('',3,(#35407,#35408,#35409,#35410),
 .UNSPECIFIED.,.F.,.F.,(4,4),(0.258432097341738,0.335446700897338),
 .UNSPECIFIED.);
#4033=B_SPLINE_CURVE_WITH_KNOTS('',3,(#35415,#35416,#35417,#35418,#35419,
#35420),.UNSPECIFIED.,.F.,.F.,(4,2,4),(2.7364662680157,2.74754737170433,
2.77362936601248),.UNSPECIFIED.);
#4034=B_SPLINE_CURVE_WITH_KNOTS('',3,(#35421,#35422,#35423,#35424,#35425,
#35426),.UNSPECIFIED.,.F.,.F.,(4,2,4),(1.69951603755067,1.72559803185882,
1.73667913554745),.UNSPECIFIED.);
#4035=B_SPLINE_CURVE_WITH_KNOTS('',3,(#35428,#35429,#35430,#35431),
 .UNSPECIFIED.,.F.,.F.,(4,4),(0.258432097339649,0.335446700893994),
 .UNSPECIFIED.);
#4036=B_SPLINE_CURVE_WITH_KNOTS('',3,(#35436,#35437,#35438,#35439,#35440,
#35441),.UNSPECIFIED.,.F.,.F.,(4,2,4),(2.73646626801472,2.74754737170335,
2.7736293660115),.UNSPECIFIED.);
#4037=B_SPLINE_CURVE_WITH_KNOTS('',3,(#35442,#35443,#35444,#35445,#35446,
#35447),.UNSPECIFIED.,.F.,.F.,(4,2,4),(1.69951603754969,1.72559803185784,
1.73667913554647),.UNSPECIFIED.);
#4038=B_SPLINE_CURVE_WITH_KNOTS('',3,(#35449,#35450,#35451,#35452),
 .UNSPECIFIED.,.F.,.F.,(4,4),(0.258432097340253,0.335446700894965),
 .UNSPECIFIED.);
#4039=B_SPLINE_CURVE_WITH_KNOTS('',3,(#35457,#35458,#35459,#35460,#35461,
#35462),.UNSPECIFIED.,.F.,.F.,(4,2,4),(2.7364662680108,2.74754737169943,
2.77362936600758),.UNSPECIFIED.);
#4040=B_SPLINE_CURVE_WITH_KNOTS('',3,(#35463,#35464,#35465,#35466,#35467,
#35468),.UNSPECIFIED.,.F.,.F.,(4,2,4),(1.69951603754577,1.72559803185392,
1.73667913554255),.UNSPECIFIED.);
#4041=B_SPLINE_CURVE_WITH_KNOTS('',3,(#35470,#35471,#35472,#35473),
 .UNSPECIFIED.,.F.,.F.,(4,4),(0.258432097337265,0.33544670089019),
 .UNSPECIFIED.);
#4042=B_SPLINE_CURVE_WITH_KNOTS('',3,(#35477,#35478,#35479,#35480),
 .UNSPECIFIED.,.F.,.F.,(4,4),(0.258432097338423,0.335446700892038),
 .UNSPECIFIED.);
#4043=B_SPLINE_CURVE_WITH_KNOTS('',3,(#35484,#35485,#35486,#35487),
 .UNSPECIFIED.,.F.,.F.,(4,4),(0.258432097338034,0.335446700891419),
 .UNSPECIFIED.);
#4044=B_SPLINE_CURVE_WITH_KNOTS('',3,(#35507,#35508,#35509,#35510,#35511,
#35512),.UNSPECIFIED.,.F.,.F.,(4,2,4),(-2.32216477286167,-1.3409543646706,
-0.618253846678096),.UNSPECIFIED.);
#4045=B_SPLINE_CURVE_WITH_KNOTS('',3,(#35515,#35516,#35517,#35518),
 .UNSPECIFIED.,.F.,.F.,(4,4),(-2.64673758792282,-2.49658914637539),
 .UNSPECIFIED.);
#4046=B_SPLINE_CURVE_WITH_KNOTS('',3,(#35794,#35795,#35796,#35797,#35798,
#35799,#35800,#35801,#35802,#35803,#35804,#35805,#35806,#35807,#35808,#35809,
#35810,#35811,#35812,#35813),.UNSPECIFIED.,.F.,.F.,(4,2,2,2,2,2,2,2,2,4),
(0.,0.658822881651553,1.04966242800916,1.12777860787417,1.6152043752719,
2.27666472044823,2.65447358681698,2.96850721180304,2.98700678447604,3.25371381595271),
 .UNSPECIFIED.);
#4047=B_SPLINE_CURVE_WITH_KNOTS('',3,(#36016,#36017,#36018,#36019,#36020,
#36021),.UNSPECIFIED.,.F.,.F.,(4,2,4),(-2.32216477286167,-1.3409543646706,
-0.618253846678096),.UNSPECIFIED.);
#4048=B_SPLINE_CURVE_WITH_KNOTS('',3,(#36024,#36025,#36026,#36027),
 .UNSPECIFIED.,.F.,.F.,(4,4),(-2.64673758792282,-2.49658914637539),
 .UNSPECIFIED.);
#4049=B_SPLINE_CURVE_WITH_KNOTS('',3,(#36303,#36304,#36305,#36306,#36307,
#36308,#36309,#36310,#36311,#36312,#36313,#36314,#36315,#36316,#36317,#36318,
#36319,#36320,#36321,#36322),.UNSPECIFIED.,.F.,.F.,(4,2,2,2,2,2,2,2,2,4),
(0.,0.658822881651553,1.04966242800916,1.12777860787417,1.6152043752719,
2.27666472044823,2.65447358681698,2.96850721180304,2.98700678447604,3.25371381595271),
 .UNSPECIFIED.);
#4050=B_SPLINE_CURVE_WITH_KNOTS('',3,(#36535,#36536,#36537,#36538,#36539,
#36540),.UNSPECIFIED.,.F.,.F.,(4,2,4),(-2.32216477286167,-1.3409543646706,
-0.618253846678096),.UNSPECIFIED.);
#4051=B_SPLINE_CURVE_WITH_KNOTS('',3,(#36543,#36544,#36545,#36546),
 .UNSPECIFIED.,.F.,.F.,(4,4),(-2.64673758792282,-2.49658914637539),
 .UNSPECIFIED.);
#4052=B_SPLINE_CURVE_WITH_KNOTS('',3,(#36822,#36823,#36824,#36825,#36826,
#36827,#36828,#36829,#36830,#36831,#36832,#36833,#36834,#36835,#36836,#36837,
#36838,#36839,#36840,#36841),.UNSPECIFIED.,.F.,.F.,(4,2,2,2,2,2,2,2,2,4),
(0.,0.658822881651553,1.04966242800916,1.12777860787417,1.6152043752719,
2.27666472044823,2.65447358681698,2.96850721180304,2.98700678447604,3.25371381595271),
 .UNSPECIFIED.);
#4053=B_SPLINE_CURVE_WITH_KNOTS('',3,(#37034,#37035,#37036,#37037,#37038,
#37039),.UNSPECIFIED.,.F.,.F.,(4,2,4),(-2.32216477286167,-1.3409543646706,
-0.618253846678096),.UNSPECIFIED.);
#4054=B_SPLINE_CURVE_WITH_KNOTS('',3,(#37042,#37043,#37044,#37045),
 .UNSPECIFIED.,.F.,.F.,(4,4),(-2.64673758792282,-2.49658914637539),
 .UNSPECIFIED.);
#4055=B_SPLINE_CURVE_WITH_KNOTS('',3,(#37321,#37322,#37323,#37324,#37325,
#37326,#37327,#37328,#37329,#37330,#37331,#37332,#37333,#37334,#37335,#37336,
#37337,#37338,#37339,#37340),.UNSPECIFIED.,.F.,.F.,(4,2,2,2,2,2,2,2,2,4),
(0.,0.658822881651553,1.04966242800916,1.12777860787417,1.6152043752719,
2.27666472044823,2.65447358681698,2.96850721180304,2.98700678447604,3.25371381595271),
 .UNSPECIFIED.);
#4056=B_SPLINE_CURVE_WITH_KNOTS('',3,(#37543,#37544,#37545,#37546,#37547,
#37548),.UNSPECIFIED.,.F.,.F.,(4,2,4),(-2.32216477286167,-1.3409543646706,
-0.618253846678096),.UNSPECIFIED.);
#4057=B_SPLINE_CURVE_WITH_KNOTS('',3,(#37551,#37552,#37553,#37554),
 .UNSPECIFIED.,.F.,.F.,(4,4),(-2.64673758792282,-2.49658914637539),
 .UNSPECIFIED.);
#4058=B_SPLINE_CURVE_WITH_KNOTS('',3,(#37830,#37831,#37832,#37833,#37834,
#37835,#37836,#37837,#37838,#37839,#37840,#37841,#37842,#37843,#37844,#37845,
#37846,#37847,#37848,#37849),.UNSPECIFIED.,.F.,.F.,(4,2,2,2,2,2,2,2,2,4),
(0.,0.658822881651553,1.04966242800916,1.12777860787417,1.6152043752719,
2.27666472044823,2.65447358681698,2.96850721180304,2.98700678447604,3.25371381595271),
 .UNSPECIFIED.);
#4059=B_SPLINE_CURVE_WITH_KNOTS('',3,(#38062,#38063,#38064,#38065,#38066,
#38067),.UNSPECIFIED.,.F.,.F.,(4,2,4),(-2.32216477286167,-1.3409543646706,
-0.618253846678096),.UNSPECIFIED.);
#4060=B_SPLINE_CURVE_WITH_KNOTS('',3,(#38070,#38071,#38072,#38073),
 .UNSPECIFIED.,.F.,.F.,(4,4),(-2.64673758792282,-2.49658914637539),
 .UNSPECIFIED.);
#4061=B_SPLINE_CURVE_WITH_KNOTS('',3,(#38349,#38350,#38351,#38352,#38353,
#38354,#38355,#38356,#38357,#38358,#38359,#38360,#38361,#38362,#38363,#38364,
#38365,#38366,#38367,#38368),.UNSPECIFIED.,.F.,.F.,(4,2,2,2,2,2,2,2,2,4),
(0.,0.658822881651553,1.04966242800916,1.12777860787417,1.6152043752719,
2.27666472044823,2.65447358681698,2.96850721180304,2.98700678447604,3.25371381595271),
 .UNSPECIFIED.);
#4062=B_SPLINE_CURVE_WITH_KNOTS('',3,(#38561,#38562,#38563,#38564,#38565,
#38566),.UNSPECIFIED.,.F.,.F.,(4,2,4),(-2.32216477286167,-1.3409543646706,
-0.618253846678096),.UNSPECIFIED.);
#4063=B_SPLINE_CURVE_WITH_KNOTS('',3,(#38569,#38570,#38571,#38572),
 .UNSPECIFIED.,.F.,.F.,(4,4),(-2.64673758792282,-2.49658914637539),
 .UNSPECIFIED.);
#4064=B_SPLINE_CURVE_WITH_KNOTS('',3,(#38848,#38849,#38850,#38851,#38852,
#38853,#38854,#38855,#38856,#38857,#38858,#38859,#38860,#38861,#38862,#38863,
#38864,#38865,#38866,#38867),.UNSPECIFIED.,.F.,.F.,(4,2,2,2,2,2,2,2,2,4),
(0.,0.658822881651553,1.04966242800916,1.12777860787417,1.6152043752719,
2.27666472044823,2.65447358681698,2.96850721180304,2.98700678447604,3.25371381595271),
 .UNSPECIFIED.);
#4065=B_SPLINE_CURVE_WITH_KNOTS('',3,(#39070,#39071,#39072,#39073,#39074,
#39075),.UNSPECIFIED.,.F.,.F.,(4,2,4),(-2.32216477286167,-1.3409543646706,
-0.618253846678096),.UNSPECIFIED.);
#4066=B_SPLINE_CURVE_WITH_KNOTS('',3,(#39078,#39079,#39080,#39081),
 .UNSPECIFIED.,.F.,.F.,(4,4),(-2.64673758792282,-2.49658914637539),
 .UNSPECIFIED.);
#4067=B_SPLINE_CURVE_WITH_KNOTS('',3,(#39357,#39358,#39359,#39360,#39361,
#39362,#39363,#39364,#39365,#39366,#39367,#39368,#39369,#39370,#39371,#39372,
#39373,#39374,#39375,#39376),.UNSPECIFIED.,.F.,.F.,(4,2,2,2,2,2,2,2,2,4),
(0.,0.658822881651553,1.04966242800916,1.12777860787417,1.6152043752719,
2.27666472044823,2.65447358681698,2.96850721180304,2.98700678447604,3.25371381595271),
 .UNSPECIFIED.);
#4068=B_SPLINE_CURVE_WITH_KNOTS('',3,(#39589,#39590,#39591,#39592,#39593,
#39594),.UNSPECIFIED.,.F.,.F.,(4,2,4),(-2.32216477286167,-1.3409543646706,
-0.618253846678096),.UNSPECIFIED.);
#4069=B_SPLINE_CURVE_WITH_KNOTS('',3,(#39597,#39598,#39599,#39600),
 .UNSPECIFIED.,.F.,.F.,(4,4),(-2.64673758792282,-2.49658914637539),
 .UNSPECIFIED.);
#4070=B_SPLINE_CURVE_WITH_KNOTS('',3,(#39876,#39877,#39878,#39879,#39880,
#39881,#39882,#39883,#39884,#39885,#39886,#39887,#39888,#39889,#39890,#39891,
#39892,#39893,#39894,#39895),.UNSPECIFIED.,.F.,.F.,(4,2,2,2,2,2,2,2,2,4),
(0.,0.658822881651553,1.04966242800916,1.12777860787417,1.6152043752719,
2.27666472044823,2.65447358681698,2.96850721180304,2.98700678447604,3.25371381595271),
 .UNSPECIFIED.);
#4071=B_SPLINE_CURVE_WITH_KNOTS('',3,(#40098,#40099,#40100,#40101,#40102,
#40103),.UNSPECIFIED.,.F.,.F.,(4,2,4),(-2.32216477286167,-1.3409543646706,
-0.618253846678096),.UNSPECIFIED.);
#4072=B_SPLINE_CURVE_WITH_KNOTS('',3,(#40106,#40107,#40108,#40109),
 .UNSPECIFIED.,.F.,.F.,(4,4),(-2.64673758792282,-2.49658914637539),
 .UNSPECIFIED.);
#4073=B_SPLINE_CURVE_WITH_KNOTS('',3,(#40385,#40386,#40387,#40388,#40389,
#40390,#40391,#40392,#40393,#40394,#40395,#40396,#40397,#40398,#40399,#40400,
#40401,#40402,#40403,#40404),.UNSPECIFIED.,.F.,.F.,(4,2,2,2,2,2,2,2,2,4),
(0.,0.658822881651553,1.04966242800916,1.12777860787417,1.6152043752719,
2.27666472044823,2.65447358681698,2.96850721180304,2.98700678447604,3.25371381595271),
 .UNSPECIFIED.);
#4074=B_SPLINE_CURVE_WITH_KNOTS('',3,(#40607,#40608,#40609,#40610,#40611,
#40612),.UNSPECIFIED.,.F.,.F.,(4,2,4),(-2.32216477286167,-1.3409543646706,
-0.618253846678096),.UNSPECIFIED.);
#4075=B_SPLINE_CURVE_WITH_KNOTS('',3,(#40615,#40616,#40617,#40618),
 .UNSPECIFIED.,.F.,.F.,(4,4),(-2.64673758792282,-2.49658914637539),
 .UNSPECIFIED.);
#4076=B_SPLINE_CURVE_WITH_KNOTS('',3,(#40894,#40895,#40896,#40897,#40898,
#40899,#40900,#40901,#40902,#40903,#40904,#40905,#40906,#40907,#40908,#40909,
#40910,#40911,#40912,#40913),.UNSPECIFIED.,.F.,.F.,(4,2,2,2,2,2,2,2,2,4),
(0.,0.658822881651553,1.04966242800916,1.12777860787417,1.6152043752719,
2.27666472044823,2.65447358681698,2.96850721180304,2.98700678447604,3.25371381595271),
 .UNSPECIFIED.);
#4077=B_SPLINE_CURVE_WITH_KNOTS('',3,(#41126,#41127,#41128,#41129,#41130,
#41131),.UNSPECIFIED.,.F.,.F.,(4,2,4),(-2.32216477286167,-1.3409543646706,
-0.618253846678096),.UNSPECIFIED.);
#4078=B_SPLINE_CURVE_WITH_KNOTS('',3,(#41134,#41135,#41136,#41137),
 .UNSPECIFIED.,.F.,.F.,(4,4),(-2.64673758792282,-2.49658914637539),
 .UNSPECIFIED.);
#4079=B_SPLINE_CURVE_WITH_KNOTS('',3,(#41413,#41414,#41415,#41416,#41417,
#41418,#41419,#41420,#41421,#41422,#41423,#41424,#41425,#41426,#41427,#41428,
#41429,#41430,#41431,#41432),.UNSPECIFIED.,.F.,.F.,(4,2,2,2,2,2,2,2,2,4),
(0.,0.658822881651553,1.04966242800916,1.12777860787417,1.6152043752719,
2.27666472044823,2.65447358681698,2.96850721180304,2.98700678447604,3.25371381595271),
 .UNSPECIFIED.);
#4080=B_SPLINE_CURVE_WITH_KNOTS('',3,(#41786,#41787,#41788,#41789),
 .UNSPECIFIED.,.F.,.F.,(4,4),(-1.,0.),.UNSPECIFIED.);
#4081=B_SPLINE_CURVE_WITH_KNOTS('',3,(#41791,#41792,#41793,#41794,#41795,
#41796,#41797,#41798,#41799,#41800,#41801,#41802,#41803,#41804,#41805,#41806,
#41807),.UNSPECIFIED.,.F.,.F.,(4,1,1,1,1,1,1,1,1,1,1,1,1,1,4),(-0.999999887132374,
-0.928571428571429,-0.857142857142857,-0.785714285714286,-0.714285714285714,
-0.619047619047619,-0.571428571428571,-0.476190476190476,-0.428571428571429,
-0.357142857142857,-0.285714285714286,-0.214285714285714,-0.142857142857143,
-0.0714285714285714,-2.25735216844453E-7),.UNSPECIFIED.);
#4082=B_SPLINE_CURVE_WITH_KNOTS('',3,(#41809,#41810,#41811,#41812),
 .UNSPECIFIED.,.F.,.F.,(4,4),(0.,0.0212132034460131),.UNSPECIFIED.);
#4083=B_SPLINE_CURVE_WITH_KNOTS('',3,(#41813,#41814,#41815,#41816,#41817,
#41818,#41819,#41820,#41821,#41822,#41823,#41824,#41825,#41826,#41827,#41828,
#41829),.UNSPECIFIED.,.F.,.F.,(4,1,1,1,1,1,1,1,1,1,1,1,1,1,4),(0.,0.0714285714285714,
0.142857142857143,0.214285714285714,0.285714285714286,0.357142857142857,
0.428571428571429,0.476190476190476,0.571428571428571,0.619047619047619,
0.714285714285714,0.785714285714286,0.857142857142857,0.928571428571429,
1.),.UNSPECIFIED.);
#4084=B_SPLINE_CURVE_WITH_KNOTS('',3,(#41834,#41835,#41836,#41837),
 .UNSPECIFIED.,.F.,.F.,(4,4),(-1.,0.),.UNSPECIFIED.);
#4085=B_SPLINE_CURVE_WITH_KNOTS('',3,(#41841,#41842,#41843,#41844,#41845,
#41846),.UNSPECIFIED.,.F.,.F.,(4,2,4),(0.,0.0106066017229243,0.0212132034458491),
 .UNSPECIFIED.);
#4086=B_SPLINE_CURVE_WITH_KNOTS('',3,(#41850,#41851,#41852,#41853,#41854,
#41855),.UNSPECIFIED.,.F.,.F.,(4,2,4),(0.,0.0106066017229245,0.0212132034458491),
 .UNSPECIFIED.);
#4087=B_SPLINE_CURVE_WITH_KNOTS('',3,(#42589,#42590,#42591,#42592,#42593,
#42594,#42595,#42596,#42597,#42598,#42599,#42600,#42601,#42602,#42603,#42604,
#42605),.UNSPECIFIED.,.F.,.F.,(4,1,1,1,1,1,1,1,1,1,1,1,1,1,4),(-0.99999988713236,
-0.928571323765762,-0.857142760399165,-0.785714197032568,-0.71428563366597,
-0.642857070299373,-0.571428506932776,-0.523809464688377,-0.428571380199581,
-0.380952337955183,-0.285714253466386,-0.214285690099789,-0.142857126733191,
-0.071428563366594,3.39227166254691E-15),.UNSPECIFIED.);
#4088=B_SPLINE_CURVE_WITH_KNOTS('',3,(#42675,#42676,#42677,#42678),
 .UNSPECIFIED.,.F.,.F.,(4,4),(0.,0.021213203446013),.UNSPECIFIED.);
#4089=B_SPLINE_CURVE_WITH_KNOTS('',3,(#42679,#42680,#42681,#42682,#42683,
#42684,#42685,#42686,#42687,#42688,#42689,#42690,#42691,#42692,#42693,#42694,
#42695),.UNSPECIFIED.,.F.,.F.,(4,1,1,1,1,1,1,1,1,1,1,1,1,1,4),(1.12867617307888E-7,
0.071428563366594,0.142857126733191,0.214285690099789,0.285714253466386,
0.380952337955183,0.428571380199581,0.523809464688377,0.571428506932776,
0.642857070299373,0.71428563366597,0.785714197032568,0.857142760399165,
0.928571323765762,0.99999988713236),.UNSPECIFIED.);
#4090=B_SPLINE_CURVE_WITH_KNOTS('',3,(#42842,#42843,#42844,#42845,#42846,
#42847,#42848,#42849,#42850),.UNSPECIFIED.,.F.,.F.,(4,1,1,1,1,1,4),(-1.,
-0.285714285714286,-0.142857142857143,-0.107142857142857,-0.0714285714285714,
-0.0357142857142857,0.),.UNSPECIFIED.);
#4091=B_SPLINE_CURVE_WITH_KNOTS('',3,(#42851,#42852,#42853,#42854,#42855,
#42856,#42857,#42858,#42859,#42860,#42861,#42862,#42863,#42864,#42865,#42866),
 .UNSPECIFIED.,.F.,.F.,(4,1,1,1,1,1,1,1,1,1,1,1,1,4),(-1.,-0.910648148148148,
-0.821296296296296,-0.731944444444444,-0.642592592592592,-0.55324074074074,
-0.463888888888888,-0.39398148148148,-0.324074074074073,-0.254166666666666,
-0.184259259259259,-0.114351851851852,-0.0444444444444444,1.31922727866773E-7),
 .UNSPECIFIED.);
#4092=B_SPLINE_CURVE_WITH_KNOTS('',3,(#42867,#42868,#42869,#42870,#42871,
#42872,#42873,#42874,#42875,#42876,#42877,#42878,#42879,#42880,#42881,#42882),
 .UNSPECIFIED.,.F.,.F.,(4,1,1,1,1,1,1,1,1,1,1,1,1,4),(0.,0.0444444444444444,
0.114351851851852,0.184259259259259,0.254166666666666,0.324074074074073,
0.39398148148148,0.463888888888888,0.55324074074074,0.642592592592592,0.731944444444444,
0.821296296296296,0.910648148148148,1.),.UNSPECIFIED.);
#4093=B_SPLINE_CURVE_WITH_KNOTS('',3,(#43614,#43615,#43616,#43617,#43618,
#43619,#43620,#43621,#43622,#43623,#43624,#43625,#43626,#43627,#43628,#43629,
#43630),.UNSPECIFIED.,.F.,.F.,(4,1,1,1,1,1,1,1,1,1,1,1,1,1,4),(-1.,-0.910648148148148,
-0.821296296296296,-0.731944444444444,-0.642592592592592,-0.55324074074074,
-0.463888888888888,-0.39398148148148,-0.324074074074073,-0.254166666666666,
-0.184259259259259,-0.114351851851852,-0.0444444444444444,-0.0305555555555556,
-1.31922710467803E-7),.UNSPECIFIED.);
#4094=B_SPLINE_CURVE_WITH_KNOTS('',3,(#43701,#43702,#43703,#43704),
 .UNSPECIFIED.,.F.,.F.,(4,4),(-1.,0.),.UNSPECIFIED.);
#4095=B_SPLINE_CURVE_WITH_KNOTS('',3,(#43705,#43706,#43707,#43708,#43709,
#43710,#43711,#43712,#43713,#43714,#43715,#43716,#43717,#43718,#43719,#43720,
#43721),.UNSPECIFIED.,.F.,.F.,(4,1,1,1,1,1,1,1,1,1,1,1,1,1,4),(-1.31922727866773E-7,
0.0305555555555556,0.0444444444444444,0.114351851851852,0.184259259259259,
0.254166666666666,0.324074074074073,0.39398148148148,0.463888888888888,
0.55324074074074,0.642592592592592,0.731944444444444,0.821296296296296,
0.910648148148148,1.),.UNSPECIFIED.);
#4096=B_SPLINE_CURVE_WITH_KNOTS('',3,(#43970,#43971,#43972,#43973),
 .UNSPECIFIED.,.F.,.F.,(4,4),(0.,0.0304160109013453),.UNSPECIFIED.);
#4097=B_SPLINE_CURVE_WITH_KNOTS('',3,(#43977,#43978,#43979,#43980),
 .UNSPECIFIED.,.F.,.F.,(4,4),(0.,0.0304159808371363),.UNSPECIFIED.);
#4098=B_SPLINE_CURVE_WITH_KNOTS('',3,(#43989,#43990,#43991,#43992),
 .UNSPECIFIED.,.F.,.F.,(4,4),(0.,0.0304160109012714),.UNSPECIFIED.);
#4099=B_SPLINE_CURVE_WITH_KNOTS('',3,(#44006,#44007,#44008,#44009),
 .UNSPECIFIED.,.F.,.F.,(4,4),(0.,0.0304159808372897),.UNSPECIFIED.);
#4100=B_SPLINE_CURVE_WITH_KNOTS('',3,(#44232,#44233,#44234,#44235,#44236,
#44237,#44238,#44239,#44240,#44241),.UNSPECIFIED.,.F.,.F.,(4,2,2,2,4),(0.,
0.0377490101969186,0.0754980203938373,0.113245913367995,0.150993806342152),
 .UNSPECIFIED.);
#4101=B_SPLINE_CURVE_WITH_KNOTS('',3,(#44243,#44244,#44245,#44246,#44247,
#44248,#44249,#44250,#44251,#44252),.UNSPECIFIED.,.F.,.F.,(4,2,2,2,4),(0.452981419026456,
0.490729312000613,0.52847720497477,0.566226215171689,0.603975225368608),
 .UNSPECIFIED.);
#4102=B_SPLINE_CURVE_WITH_KNOTS('',3,(#44253,#44254,#44255,#44256,#44257,
#44258,#44259,#44260,#44261,#44262,#44263,#44264,#44265,#44266,#44267,#44268,
#44269,#44270),.UNSPECIFIED.,.F.,.F.,(4,2,2,2,2,2,2,2,4),(0.150993806342152,
0.188741699316309,0.226489592290467,0.264238602487385,0.301987612684304,
0.339736622881222,0.377485633078141,0.415233526052298,0.452981419026456),
 .UNSPECIFIED.);
#4103=B_SPLINE_CURVE_WITH_KNOTS('',3,(#45131,#45132,#45133,#45134),
 .UNSPECIFIED.,.F.,.F.,(4,4),(-1.,0.),.UNSPECIFIED.);
#4104=B_SPLINE_CURVE_WITH_KNOTS('',3,(#45136,#45137,#45138,#45139,#45140,
#45141,#45142,#45143,#45144,#45145,#45146,#45147,#45148,#45149),
 .UNSPECIFIED.,.F.,.F.,(4,1,1,1,1,1,1,1,1,1,1,4),(-0.999999865868381,-0.914814814814814,
-0.829629629629628,-0.744444444444442,-0.619444444444443,-0.504629629629628,
-0.389814814814814,-0.275,-0.266666666666666,-0.177777777777777,-0.0888888888888885,
-2.68263378817682E-7),.UNSPECIFIED.);
#4105=B_SPLINE_CURVE_WITH_KNOTS('',3,(#45151,#45152,#45153,#45154),
 .UNSPECIFIED.,.F.,.F.,(4,4),(0.,0.0212132034459712),.UNSPECIFIED.);
#4106=B_SPLINE_CURVE_WITH_KNOTS('',3,(#45155,#45156,#45157,#45158,#45159,
#45160,#45161,#45162,#45163,#45164,#45165,#45166,#45167,#45168),
 .UNSPECIFIED.,.F.,.F.,(4,1,1,1,1,1,1,1,1,1,1,4),(-3.29679099043599E-16,
0.0888888888888885,0.177777777777777,0.266666666666666,0.275,0.389814814814814,
0.504629629629628,0.619444444444443,0.744444444444442,0.829629629629628,
0.914814814814814,1.),.UNSPECIFIED.);
#4107=B_SPLINE_CURVE_WITH_KNOTS('',3,(#45173,#45174,#45175,#45176),
 .UNSPECIFIED.,.F.,.F.,(4,4),(-1.,0.),.UNSPECIFIED.);
#4108=B_SPLINE_CURVE_WITH_KNOTS('',3,(#45180,#45181,#45182,#45183,#45184,
#45185),.UNSPECIFIED.,.F.,.F.,(4,2,4),(0.,0.0106066017228885,0.0212132034457774),
 .UNSPECIFIED.);
#4109=B_SPLINE_CURVE_WITH_KNOTS('',3,(#45189,#45190,#45191,#45192,#45193,
#45194),.UNSPECIFIED.,.F.,.F.,(4,2,4),(0.,0.0106066017228885,0.0212132034457775),
 .UNSPECIFIED.);
#4110=B_SPLINE_CURVE_WITH_KNOTS('',3,(#45928,#45929,#45930,#45931,#45932,
#45933,#45934,#45935,#45936,#45937,#45938,#45939,#45940,#45941),
 .UNSPECIFIED.,.F.,.F.,(4,1,1,1,1,1,1,1,1,1,1,4),(-0.999999865868361,-0.914814725393722,
-0.829629584919082,-0.744444444444442,-0.619444444444443,-0.504629629629628,
-0.389814814814814,-0.275,-0.266666666666666,-0.177777777777776,-0.0888888888888856,
4.77815499535063E-15),.UNSPECIFIED.);
#4111=B_SPLINE_CURVE_WITH_KNOTS('',3,(#45999,#46000,#46001,#46002),
 .UNSPECIFIED.,.F.,.F.,(4,4),(0.,0.0212132034459714),.UNSPECIFIED.);
#4112=B_SPLINE_CURVE_WITH_KNOTS('',3,(#46003,#46004,#46005,#46006,#46007,
#46008,#46009,#46010,#46011,#46012,#46013,#46014,#46015,#46016),
 .UNSPECIFIED.,.F.,.F.,(4,1,1,1,1,1,1,1,1,1,1,4),(1.3413170185661E-7,0.0888888888888856,
0.177777777777776,0.266666666666666,0.275,0.389814814814814,0.504629629629628,
0.619444444444443,0.744444444444442,0.829629584919082,0.914814725393722,
0.999999865868361),.UNSPECIFIED.);
#4113=B_SPLINE_CURVE_WITH_KNOTS('',3,(#46123,#46124,#46125,#46126),
 .UNSPECIFIED.,.F.,.F.,(4,4),(-1.,0.),.UNSPECIFIED.);
#4114=B_SPLINE_CURVE_WITH_KNOTS('',3,(#46127,#46128,#46129,#46130,#46131,
#46132,#46133,#46134,#46135,#46136,#46137,#46138,#46139,#46140,#46141,#46142,
#46143,#46144,#46145,#46146,#46147,#46148,#46149,#46150,#46151,#46152),
 .UNSPECIFIED.,.F.,.F.,(4,1,1,1,1,1,1,1,1,1,1,1,1,1,1,1,1,1,1,1,1,1,1,4),
(-1.,-0.988888888888886,-0.969444444444442,-0.856944444444442,-0.744444444444442,
-0.688888888888887,-0.686111111111109,-0.658333333333332,-0.644444444444443,
-0.547222222222221,-0.466666666666666,-0.433333333333332,-0.36111111111111,
-0.277777777777777,-0.218055555555555,-0.158333333333333,-0.15,-0.147222222222222,
-0.130555555555556,-0.105555555555556,-0.102777777777778,-0.05,-0.00277777777777778,
1.52611180263545E-7),.UNSPECIFIED.);
#4115=B_SPLINE_CURVE_WITH_KNOTS('',3,(#46153,#46154,#46155,#46156,#46157,
#46158,#46159,#46160,#46161,#46162,#46163,#46164,#46165,#46166,#46167,#46168,
#46169,#46170,#46171,#46172,#46173,#46174,#46175,#46176,#46177,#46178),
 .UNSPECIFIED.,.F.,.F.,(4,1,1,1,1,1,1,1,1,1,1,1,1,1,1,1,1,1,1,1,1,1,1,4),
(-2.64697796016969E-23,0.00277777777777778,0.05,0.102777777777778,0.105555555555556,
0.130555555555556,0.147222222222222,0.15,0.158333333333333,0.218055555555555,
0.277777777777777,0.36111111111111,0.433333333333332,0.466666666666666,
0.547222222222221,0.644444444444443,0.658333333333332,0.686111111111109,
0.688888888888887,0.744444444444442,0.856944444444442,0.969444444444442,
0.988888888888886,1.),.UNSPECIFIED.);
#4116=B_SPLINE_CURVE_WITH_KNOTS('',3,(#46910,#46911,#46912,#46913,#46914,
#46915,#46916,#46917,#46918,#46919,#46920,#46921,#46922,#46923,#46924,#46925,
#46926,#46927,#46928,#46929,#46930,#46931,#46932,#46933),.UNSPECIFIED.,
 .F.,.F.,(4,1,1,1,1,1,1,1,1,1,1,1,1,1,1,1,1,1,1,1,1,4),(-1.,-0.988888888888886,
-0.969444444444442,-0.856944444444442,-0.744444444444442,-0.688888888888887,
-0.686111111111109,-0.658333333333332,-0.644444444444443,-0.547222222222221,
-0.466666666666666,-0.433333333333332,-0.36111111111111,-0.277777777777777,
-0.218055555555555,-0.158333333333333,-0.15,-0.147222222222222,-0.105555555555556,
-0.0527777777777778,-0.05,-1.52611156942486E-7),.UNSPECIFIED.);
#4117=B_SPLINE_CURVE_WITH_KNOTS('',3,(#47032,#47033,#47034,#47035),
 .UNSPECIFIED.,.F.,.F.,(4,4),(-1.,0.),.UNSPECIFIED.);
#4118=B_SPLINE_CURVE_WITH_KNOTS('',3,(#47036,#47037,#47038,#47039,#47040,
#47041,#47042,#47043,#47044,#47045,#47046,#47047,#47048,#47049,#47050,#47051,
#47052,#47053,#47054,#47055,#47056,#47057,#47058,#47059),.UNSPECIFIED.,
 .F.,.F.,(4,1,1,1,1,1,1,1,1,1,1,1,1,1,1,1,1,1,1,1,1,4),(-1.52611180304074E-7,
0.05,0.0527777777777778,0.105555555555556,0.147222222222222,0.15,0.158333333333333,
0.218055555555555,0.277777777777777,0.36111111111111,0.433333333333332,
0.466666666666666,0.547222222222221,0.644444444444443,0.658333333333332,
0.686111111111109,0.688888888888887,0.744444444444442,0.856944444444442,
0.969444444444442,0.988888888888886,1.),.UNSPECIFIED.);
#4119=B_SPLINE_CURVE_WITH_KNOTS('',3,(#47356,#47357,#47358,#47359,#47360,
#47361,#47362,#47363,#47364,#47365,#47366,#47367,#47368,#47369,#47370,#47371,
#47372,#47373,#47374),.UNSPECIFIED.,.F.,.F.,(4,3,3,3,3,3,4),(-1.95549230332054,
-1.75875950758926,-1.34349617171388,-1.06103160839237,-0.696688766685516,
-0.248712120243735,0.),.UNSPECIFIED.);
#4120=B_SPLINE_CURVE_WITH_KNOTS('',3,(#47378,#47379,#47380,#47381,#47382,
#47383,#47384,#47385,#47386,#47387,#47388,#47389,#47390,#47391),
 .UNSPECIFIED.,.F.,.F.,(4,2,2,2,2,2,4),(-1.99248695526351,-1.80900909844286,
-1.62729798971959,-1.17075046205492,-0.668721558370408,-0.361288435792572,
-0.0338550864812443),.UNSPECIFIED.);
#4121=B_SPLINE_CURVE_WITH_KNOTS('',3,(#47393,#47394,#47395,#47396),
 .UNSPECIFIED.,.F.,.F.,(4,4),(-0.777523289324711,-0.553838937397288),
 .UNSPECIFIED.);
#4122=B_SPLINE_CURVE_WITH_KNOTS('',3,(#47398,#47399,#47400,#47401,#47402,
#47403,#47404,#47405,#47406,#47407,#47408,#47409,#47410,#47411,#47412,#47413,
#47414,#47415,#47416,#47417,#47418,#47419,#47420,#47421,#47422,#47423,#47424,
#47425),.UNSPECIFIED.,.F.,.F.,(4,3,3,3,3,3,3,3,3,4),(-4.29295029284639,
-3.67766994703909,-2.9703163241262,-2.3742471528823,-2.00020115326112,-1.70071199906103,
-1.1320234547883,-0.387157778255963,-0.249187079614097,0.),
 .UNSPECIFIED.);
#4123=B_SPLINE_CURVE_WITH_KNOTS('',3,(#47428,#47429,#47430,#47431,#47432,
#47433,#47434,#47435,#47436,#47437,#47438,#47439,#47440,#47441,#47442,#47443,
#47444,#47445,#47446,#47447,#47448,#47449,#47450,#47451,#47452,#47453,#47454,
#47455,#47456,#47457,#47458,#47459,#47460,#47461,#47462,#47463,#47464,#47465,
#47466,#47467,#47468,#47469,#47470,#47471,#47472,#47473,#47474,#47475,#47476,
#47477,#47478,#47479),.UNSPECIFIED.,.F.,.F.,(4,3,3,3,3,3,3,3,3,3,3,3,3,
3,3,3,3,4),(-7.1293628449372,-6.73503958122377,-5.85541918839373,-5.49840246457414,
-4.52430913123556,-4.07614123330263,-3.82946470849973,-3.04197748945298,
-2.81695323321067,-2.4773465147895,-2.09725773417371,-1.9043847028781,-1.69190045714872,
-1.20885650102308,-0.931359575039856,-0.504800480040873,-0.274181197077094,
-0.172427513903814),.UNSPECIFIED.);
#4124=B_SPLINE_CURVE_WITH_KNOTS('',3,(#47483,#47484,#47485,#47486),
 .UNSPECIFIED.,.F.,.F.,(4,4),(-0.083488010518486,0.),.UNSPECIFIED.);
#4125=B_SPLINE_CURVE_WITH_KNOTS('',3,(#47490,#47491,#47492,#47493),
 .UNSPECIFIED.,.F.,.F.,(4,4),(-0.0834879590262616,0.),.UNSPECIFIED.);
#4126=B_SPLINE_CURVE_WITH_KNOTS('',3,(#47497,#47498,#47499,#47500),
 .UNSPECIFIED.,.F.,.F.,(4,4),(0.13198468181481,0.18198468181481),
 .UNSPECIFIED.);
#4127=B_SPLINE_CURVE_WITH_KNOTS('',3,(#47502,#47503,#47504,#47505),
 .UNSPECIFIED.,.F.,.F.,(4,4),(0.232761481296011,0.241956189842182),
 .UNSPECIFIED.);
#4128=B_SPLINE_CURVE_WITH_KNOTS('',3,(#47507,#47508,#47509,#47510,#47511,
#47512),.UNSPECIFIED.,.F.,.F.,(4,2,4),(-0.358152343845461,-0.17793853757118,
0.),.UNSPECIFIED.);
#4129=B_SPLINE_CURVE_WITH_KNOTS('',3,(#47516,#47517,#47518,#47519,#47520,
#47521),.UNSPECIFIED.,.F.,.F.,(4,2,4),(-0.346939061794772,-0.172188193249223,
0.),.UNSPECIFIED.);
#4130=B_SPLINE_CURVE_WITH_KNOTS('',3,(#47523,#47524,#47525,#47526),
 .UNSPECIFIED.,.F.,.F.,(4,4),(0.13198468181481,0.18198468181481),
 .UNSPECIFIED.);
#4131=B_SPLINE_CURVE_WITH_KNOTS('',3,(#47530,#47531,#47532,#47533),
 .UNSPECIFIED.,.F.,.F.,(4,4),(0.359141024466699,0.413101541919944),
 .UNSPECIFIED.);
#4132=B_SPLINE_CURVE_WITH_KNOTS('',3,(#47535,#47536,#47537,#47538,#47539,
#47540),.UNSPECIFIED.,.F.,.F.,(4,2,4),(-0.358152325449159,-0.177938418239515,
0.),.UNSPECIFIED.);
#4133=B_SPLINE_CURVE_WITH_KNOTS('',3,(#47544,#47545,#47546,#47547,#47548,
#47549),.UNSPECIFIED.,.F.,.F.,(4,2,4),(-0.346939061574871,-0.172188198132723,
0.),.UNSPECIFIED.);
#4134=B_SPLINE_CURVE_WITH_KNOTS('',3,(#47551,#47552,#47553,#47554),
 .UNSPECIFIED.,.F.,.F.,(4,4),(0.13198468181481,0.181984681814809),
 .UNSPECIFIED.);
#4135=B_SPLINE_CURVE_WITH_KNOTS('',3,(#47558,#47559,#47560,#47561),
 .UNSPECIFIED.,.F.,.F.,(4,4),(0.35914082376606,0.413101294181168),
 .UNSPECIFIED.);
#4136=B_SPLINE_CURVE_WITH_KNOTS('',3,(#47563,#47564,#47565,#47566,#47567,
#47568),.UNSPECIFIED.,.F.,.F.,(4,2,4),(-0.358152343845461,-0.17793853757118,
0.),.UNSPECIFIED.);
#4137=B_SPLINE_CURVE_WITH_KNOTS('',3,(#47572,#47573,#47574,#47575,#47576,
#47577),.UNSPECIFIED.,.F.,.F.,(4,2,4),(-0.346939061794772,-0.172188193249223,
0.),.UNSPECIFIED.);
#4138=B_SPLINE_CURVE_WITH_KNOTS('',3,(#47579,#47580,#47581,#47582),
 .UNSPECIFIED.,.F.,.F.,(4,4),(0.131984681814809,0.181984681814809),
 .UNSPECIFIED.);
#4139=B_SPLINE_CURVE_WITH_KNOTS('',3,(#47586,#47587,#47588,#47589),
 .UNSPECIFIED.,.F.,.F.,(4,4),(0.359141033252547,0.41310155276493),
 .UNSPECIFIED.);
#4140=B_SPLINE_CURVE_WITH_KNOTS('',3,(#47591,#47592,#47593,#47594,#47595,
#47596),.UNSPECIFIED.,.F.,.F.,(4,2,4),(-0.358152325449159,-0.177938418239515,
0.),.UNSPECIFIED.);
#4141=B_SPLINE_CURVE_WITH_KNOTS('',3,(#47600,#47601,#47602,#47603,#47604,
#47605),.UNSPECIFIED.,.F.,.F.,(4,2,4),(-0.346939061574871,-0.172188198132723,
0.),.UNSPECIFIED.);
#4142=B_SPLINE_CURVE_WITH_KNOTS('',3,(#47607,#47608,#47609,#47610),
 .UNSPECIFIED.,.F.,.F.,(4,4),(0.131984681814811,0.18198468181481),
 .UNSPECIFIED.);
#4143=B_SPLINE_CURVE_WITH_KNOTS('',3,(#47614,#47615,#47616,#47617),
 .UNSPECIFIED.,.F.,.F.,(4,4),(0.359140820403378,0.413101290030381),
 .UNSPECIFIED.);
#4144=B_SPLINE_CURVE_WITH_KNOTS('',3,(#47619,#47620,#47621,#47622,#47623,
#47624),.UNSPECIFIED.,.F.,.F.,(4,2,4),(-0.358152343845461,-0.17793853757118,
0.),.UNSPECIFIED.);
#4145=B_SPLINE_CURVE_WITH_KNOTS('',3,(#47628,#47629,#47630,#47631,#47632,
#47633),.UNSPECIFIED.,.F.,.F.,(4,2,4),(-0.346939061794772,-0.172188193249223,
0.),.UNSPECIFIED.);
#4146=B_SPLINE_CURVE_WITH_KNOTS('',3,(#47635,#47636,#47637,#47638),
 .UNSPECIFIED.,.F.,.F.,(4,4),(0.131984681814811,0.181984681814811),
 .UNSPECIFIED.);
#4147=B_SPLINE_CURVE_WITH_KNOTS('',3,(#47642,#47643,#47644,#47645),
 .UNSPECIFIED.,.F.,.F.,(4,4),(0.359141030289299,0.413101549107184),
 .UNSPECIFIED.);
#4148=B_SPLINE_CURVE_WITH_KNOTS('',3,(#47647,#47648,#47649,#47650,#47651,
#47652),.UNSPECIFIED.,.F.,.F.,(4,2,4),(-0.358152325449159,-0.177938418239515,
0.),.UNSPECIFIED.);
#4149=B_SPLINE_CURVE_WITH_KNOTS('',3,(#47656,#47657,#47658,#47659,#47660,
#47661),.UNSPECIFIED.,.F.,.F.,(4,2,4),(-0.346939061574871,-0.172188198132723,
0.),.UNSPECIFIED.);
#4150=B_SPLINE_CURVE_WITH_KNOTS('',3,(#47663,#47664,#47665,#47666),
 .UNSPECIFIED.,.F.,.F.,(4,4),(0.131984681814809,0.181984681814809),
 .UNSPECIFIED.);
#4151=B_SPLINE_CURVE_WITH_KNOTS('',3,(#47670,#47671,#47672,#47673),
 .UNSPECIFIED.,.F.,.F.,(4,4),(0.359140824117849,0.413101294615407),
 .UNSPECIFIED.);
#4152=B_SPLINE_CURVE_WITH_KNOTS('',3,(#47675,#47676,#47677,#47678,#47679,
#47680),.UNSPECIFIED.,.F.,.F.,(4,2,4),(-0.358152343845461,-0.17793853757118,
0.),.UNSPECIFIED.);
#4153=B_SPLINE_CURVE_WITH_KNOTS('',3,(#47689,#47690,#47691,#47692,#47693,
#47694),.UNSPECIFIED.,.F.,.F.,(4,2,4),(-0.346939061794772,-0.172188193249223,
0.),.UNSPECIFIED.);
#4154=B_SPLINE_CURVE_WITH_KNOTS('',3,(#47696,#47697,#47698,#47699),
 .UNSPECIFIED.,.F.,.F.,(4,4),(0.13198468181481,0.18198468181481),
 .UNSPECIFIED.);
#4155=B_SPLINE_CURVE_WITH_KNOTS('',3,(#47703,#47704,#47705,#47706),
 .UNSPECIFIED.,.F.,.F.,(4,4),(0.359141030289304,0.413101549107192),
 .UNSPECIFIED.);
#4156=B_SPLINE_CURVE_WITH_KNOTS('',3,(#47708,#47709,#47710,#47711,#47712,
#47713),.UNSPECIFIED.,.F.,.F.,(4,2,4),(-0.358152325449159,-0.177938418239515,
0.),.UNSPECIFIED.);
#4157=B_SPLINE_CURVE_WITH_KNOTS('',3,(#47717,#47718,#47719,#47720,#47721,
#47722),.UNSPECIFIED.,.F.,.F.,(4,2,4),(-0.346939061574871,-0.172188198132723,
0.),.UNSPECIFIED.);
#4158=B_SPLINE_CURVE_WITH_KNOTS('',3,(#47724,#47725,#47726,#47727),
 .UNSPECIFIED.,.F.,.F.,(4,4),(0.131984681814811,0.18198468181481),
 .UNSPECIFIED.);
#4159=B_SPLINE_CURVE_WITH_KNOTS('',3,(#47731,#47732,#47733,#47734),
 .UNSPECIFIED.,.F.,.F.,(4,4),(0.359140820403392,0.413101290030397),
 .UNSPECIFIED.);
#4160=B_SPLINE_CURVE_WITH_KNOTS('',3,(#47736,#47737,#47738,#47739,#47740,
#47741),.UNSPECIFIED.,.F.,.F.,(4,2,4),(-0.358152343845461,-0.17793853757118,
0.),.UNSPECIFIED.);
#4161=B_SPLINE_CURVE_WITH_KNOTS('',3,(#47745,#47746,#47747,#47748,#47749,
#47750),.UNSPECIFIED.,.F.,.F.,(4,2,4),(-0.346939061794772,-0.172188193249223,
0.),.UNSPECIFIED.);
#4162=B_SPLINE_CURVE_WITH_KNOTS('',3,(#47752,#47753,#47754,#47755),
 .UNSPECIFIED.,.F.,.F.,(4,4),(0.13198468181481,0.18198468181481),
 .UNSPECIFIED.);
#4163=B_SPLINE_CURVE_WITH_KNOTS('',3,(#47759,#47760,#47761,#47762),
 .UNSPECIFIED.,.F.,.F.,(4,4),(0.359141033252549,0.413101552764933),
 .UNSPECIFIED.);
#4164=B_SPLINE_CURVE_WITH_KNOTS('',3,(#47764,#47765,#47766,#47767,#47768,
#47769),.UNSPECIFIED.,.F.,.F.,(4,2,4),(-0.358152325449159,-0.177938418239515,
0.),.UNSPECIFIED.);
#4165=B_SPLINE_CURVE_WITH_KNOTS('',3,(#47773,#47774,#47775,#47776,#47777,
#47778),.UNSPECIFIED.,.F.,.F.,(4,2,4),(-0.346939061574871,-0.172188198132723,
0.),.UNSPECIFIED.);
#4166=B_SPLINE_CURVE_WITH_KNOTS('',3,(#47780,#47781,#47782,#47783),
 .UNSPECIFIED.,.F.,.F.,(4,4),(0.13198468181481,0.181984681814809),
 .UNSPECIFIED.);
#4167=B_SPLINE_CURVE_WITH_KNOTS('',3,(#47787,#47788,#47789,#47790),
 .UNSPECIFIED.,.F.,.F.,(4,4),(0.359140823766061,0.413101294181171),
 .UNSPECIFIED.);
#4168=B_SPLINE_CURVE_WITH_KNOTS('',3,(#47792,#47793,#47794,#47795,#47796,
#47797),.UNSPECIFIED.,.F.,.F.,(4,2,4),(-0.358152343845461,-0.17793853757118,
0.),.UNSPECIFIED.);
#4169=B_SPLINE_CURVE_WITH_KNOTS('',3,(#47801,#47802,#47803,#47804,#47805,
#47806),.UNSPECIFIED.,.F.,.F.,(4,2,4),(-0.346939061794772,-0.172188193249223,
0.),.UNSPECIFIED.);
#4170=B_SPLINE_CURVE_WITH_KNOTS('',3,(#47808,#47809,#47810,#47811),
 .UNSPECIFIED.,.F.,.F.,(4,4),(0.131984681814811,0.18198468181481),
 .UNSPECIFIED.);
#4171=B_SPLINE_CURVE_WITH_KNOTS('',3,(#47815,#47816,#47817,#47818),
 .UNSPECIFIED.,.F.,.F.,(4,4),(0.359141024466694,0.413101541919935),
 .UNSPECIFIED.);
#4172=B_SPLINE_CURVE_WITH_KNOTS('',3,(#47820,#47821,#47822,#47823,#47824,
#47825),.UNSPECIFIED.,.F.,.F.,(4,2,4),(-0.358152325449159,-0.177938418239515,
0.),.UNSPECIFIED.);
#4173=B_SPLINE_CURVE_WITH_KNOTS('',3,(#47829,#47830,#47831,#47832,#47833,
#47834),.UNSPECIFIED.,.F.,.F.,(4,2,4),(-0.346939061574871,-0.172188198132723,
0.),.UNSPECIFIED.);
#4174=B_SPLINE_CURVE_WITH_KNOTS('',3,(#47836,#47837,#47838,#47839),
 .UNSPECIFIED.,.F.,.F.,(4,4),(0.13198468181481,0.18198468181481),
 .UNSPECIFIED.);
#4175=B_SPLINE_CURVE_WITH_KNOTS('',3,(#47843,#47844,#47845,#47846),
 .UNSPECIFIED.,.F.,.F.,(4,4),(0.359140822627922,0.413101292776284),
 .UNSPECIFIED.);
#4176=B_SPLINE_CURVE_WITH_KNOTS('',3,(#47848,#47849,#47850,#47851,#47852,
#47853),.UNSPECIFIED.,.F.,.F.,(4,2,4),(-0.358152343845461,-0.17793853757118,
0.),.UNSPECIFIED.);
#4177=B_SPLINE_CURVE_WITH_KNOTS('',3,(#47857,#47858,#47859,#47860,#47861,
#47862),.UNSPECIFIED.,.F.,.F.,(4,2,4),(-0.346939061794772,-0.172188193249223,
0.),.UNSPECIFIED.);
#4178=B_SPLINE_CURVE_WITH_KNOTS('',3,(#47864,#47865,#47866,#47867),
 .UNSPECIFIED.,.F.,.F.,(4,4),(0.13198468181481,0.18198468181481),
 .UNSPECIFIED.);
#4179=B_SPLINE_CURVE_WITH_KNOTS('',3,(#47871,#47872,#47873,#47874),
 .UNSPECIFIED.,.F.,.F.,(4,4),(0.359141034166343,0.413101553892894),
 .UNSPECIFIED.);
#4180=B_SPLINE_CURVE_WITH_KNOTS('',3,(#47876,#47877,#47878,#47879,#47880,
#47881),.UNSPECIFIED.,.F.,.F.,(4,2,4),(-0.358152325449159,-0.177938418239515,
0.),.UNSPECIFIED.);
#4181=B_SPLINE_CURVE_WITH_KNOTS('',3,(#47884,#47885,#47886,#47887,#47888,
#47889),.UNSPECIFIED.,.F.,.F.,(4,2,4),(-0.346939061574871,-0.172188198132723,
0.),.UNSPECIFIED.);
#4182=B_SPLINE_CURVE_WITH_KNOTS('',3,(#47892,#47893,#47894,#47895),
 .UNSPECIFIED.,.F.,.F.,(4,4),(-0.0834880103557405,0.),.UNSPECIFIED.);
#4183=B_SPLINE_CURVE_WITH_KNOTS('',3,(#47897,#47898,#47899,#47900),
 .UNSPECIFIED.,.F.,.F.,(4,4),(-0.083487959129736,0.),.UNSPECIFIED.);
#4184=B_SPLINE_CURVE_WITH_KNOTS('',3,(#47904,#47905,#47906,#47907),
 .UNSPECIFIED.,.F.,.F.,(4,4),(-0.0834880111905181,0.),.UNSPECIFIED.);
#4185=B_SPLINE_CURVE_WITH_KNOTS('',3,(#47909,#47910,#47911,#47912),
 .UNSPECIFIED.,.F.,.F.,(4,4),(-0.0834879604909712,0.),.UNSPECIFIED.);
#4186=B_SPLINE_CURVE_WITH_KNOTS('',3,(#47916,#47917,#47918,#47919),
 .UNSPECIFIED.,.F.,.F.,(4,4),(-0.0834880110227881,0.),.UNSPECIFIED.);
#4187=B_SPLINE_CURVE_WITH_KNOTS('',3,(#47921,#47922,#47923,#47924),
 .UNSPECIFIED.,.F.,.F.,(4,4),(-0.0834879596098838,0.),.UNSPECIFIED.);
#4188=B_SPLINE_CURVE_WITH_KNOTS('',3,(#47928,#47929,#47930,#47931),
 .UNSPECIFIED.,.F.,.F.,(4,4),(-0.0834880104037423,0.),.UNSPECIFIED.);
#4189=B_SPLINE_CURVE_WITH_KNOTS('',3,(#47933,#47934,#47935,#47936),
 .UNSPECIFIED.,.F.,.F.,(4,4),(-0.083487958469891,0.),.UNSPECIFIED.);
#4190=B_SPLINE_CURVE_WITH_KNOTS('',3,(#47940,#47941,#47942,#47943),
 .UNSPECIFIED.,.F.,.F.,(4,4),(-0.0834880117617837,0.),.UNSPECIFIED.);
#4191=B_SPLINE_CURVE_WITH_KNOTS('',3,(#47945,#47946,#47947,#47948),
 .UNSPECIFIED.,.F.,.F.,(4,4),(-0.0834879580772816,0.),.UNSPECIFIED.);
#4192=B_SPLINE_CURVE_WITH_KNOTS('',3,(#47952,#47953,#47954,#47955),
 .UNSPECIFIED.,.F.,.F.,(4,4),(-0.0834880120026571,0.),.UNSPECIFIED.);
#4193=B_SPLINE_CURVE_WITH_KNOTS('',3,(#47957,#47958,#47959,#47960),
 .UNSPECIFIED.,.F.,.F.,(4,4),(-0.0834879591399868,0.),.UNSPECIFIED.);
#4194=B_SPLINE_CURVE_WITH_KNOTS('',3,(#47964,#47965,#47966,#47967),
 .UNSPECIFIED.,.F.,.F.,(4,4),(-0.0834880112339728,0.),.UNSPECIFIED.);
#4195=B_SPLINE_CURVE_WITH_KNOTS('',3,(#47969,#47970,#47971,#47972),
 .UNSPECIFIED.,.F.,.F.,(4,4),(-0.0834879586604845,0.),.UNSPECIFIED.);
#4196=B_SPLINE_CURVE_WITH_KNOTS('',3,(#47976,#47977,#47978,#47979),
 .UNSPECIFIED.,.F.,.F.,(4,4),(-0.0834880108880153,0.),.UNSPECIFIED.);
#4197=B_SPLINE_CURVE_WITH_KNOTS('',3,(#47981,#47982,#47983,#47984),
 .UNSPECIFIED.,.F.,.F.,(4,4),(-0.083487960114269,0.),.UNSPECIFIED.);
#4198=B_SPLINE_CURVE_WITH_KNOTS('',3,(#47988,#47989,#47990,#47991),
 .UNSPECIFIED.,.F.,.F.,(4,4),(-0.0834880111006107,0.),.UNSPECIFIED.);
#4199=B_SPLINE_CURVE_WITH_KNOTS('',3,(#47993,#47994,#47995,#47996),
 .UNSPECIFIED.,.F.,.F.,(4,4),(-0.0834879593252191,0.),.UNSPECIFIED.);
#4200=B_SPLINE_CURVE_WITH_KNOTS('',3,(#48000,#48001,#48002,#48003),
 .UNSPECIFIED.,.F.,.F.,(4,4),(-0.0834880109980362,0.),.UNSPECIFIED.);
#4201=B_SPLINE_CURVE_WITH_KNOTS('',3,(#48005,#48006,#48007,#48008),
 .UNSPECIFIED.,.F.,.F.,(4,4),(-0.0834879591189384,0.),.UNSPECIFIED.);
#4202=B_SPLINE_CURVE_WITH_KNOTS('',3,(#48012,#48013,#48014,#48015),
 .UNSPECIFIED.,.F.,.F.,(4,4),(-0.0834880113860417,0.),.UNSPECIFIED.);
#4203=B_SPLINE_CURVE_WITH_KNOTS('',3,(#48017,#48018,#48019,#48020),
 .UNSPECIFIED.,.F.,.F.,(4,4),(-0.0834879599185004,0.),.UNSPECIFIED.);
#4204=B_SPLINE_CURVE_WITH_KNOTS('',3,(#48024,#48025,#48026,#48027),
 .UNSPECIFIED.,.F.,.F.,(4,4),(-0.0834880117067383,0.),.UNSPECIFIED.);
#4205=B_SPLINE_CURVE_WITH_KNOTS('',3,(#48029,#48030,#48031,#48032),
 .UNSPECIFIED.,.F.,.F.,(4,4),(-0.0834879582890902,0.),.UNSPECIFIED.);
#4206=B_SPLINE_CURVE_WITH_KNOTS('',3,(#48036,#48037,#48038,#48039),
 .UNSPECIFIED.,.F.,.F.,(4,4),(-0.0834880121469109,0.),.UNSPECIFIED.);
#4207=B_SPLINE_CURVE_WITH_KNOTS('',3,(#48041,#48042,#48043,#48044),
 .UNSPECIFIED.,.F.,.F.,(4,4),(-0.0834879588321369,0.),.UNSPECIFIED.);
#4208=B_SPLINE_CURVE_WITH_KNOTS('',3,(#48179,#48180,#48181,#48182),
 .UNSPECIFIED.,.F.,.F.,(4,4),(19.6867712077087,23.2012226018398),
 .UNSPECIFIED.);
#4209=B_SPLINE_CURVE_WITH_KNOTS('',3,(#48184,#48185,#48186,#48187,#48188,
#48189,#48190,#48191,#48192,#48193,#48194,#48195,#48196,#48197,#48198,#48199,
#48200,#48201,#48202,#48203,#48204,#48205,#48206,#48207,#48208,#48209,#48210,
#48211),.UNSPECIFIED.,.F.,.F.,(4,3,3,3,3,3,3,3,3,4),(-4.29295029280653,
-3.67766994701249,-2.97031632412777,-2.37424715288027,-2.00020115318578,
-1.70071199888906,-1.13202345479137,-0.387157778243597,-0.249187079614106,
0.),.UNSPECIFIED.);
#4210=B_SPLINE_CURVE_WITH_KNOTS('',3,(#48213,#48214,#48215,#48216),
 .UNSPECIFIED.,.F.,.F.,(4,4),(-2.25355902969558,-0.8318795023757),
 .UNSPECIFIED.);
#4211=B_SPLINE_CURVE_WITH_KNOTS('',3,(#48217,#48218,#48219,#48220,#48221,
#48222,#48223,#48224,#48225,#48226,#48227,#48228,#48229,#48230,#48231,#48232,
#48233,#48234,#48235,#48236,#48237,#48238,#48239,#48240,#48241,#48242,#48243,
#48244),.UNSPECIFIED.,.F.,.F.,(4,3,3,3,3,3,3,3,3,4),(0.,0.198329530181083,
0.718473337675007,0.921591739443192,1.13394541355614,1.63848434558204,1.82278760043539,
1.95589943946294,2.14302327760794,2.31810070175045),.UNSPECIFIED.);
#4212=B_SPLINE_CURVE_WITH_KNOTS('',3,(#48247,#48248,#48249,#48250),
 .UNSPECIFIED.,.F.,.F.,(4,4),(-1.48876608190222,-1.26494675411689),
 .UNSPECIFIED.);
#4213=B_SPLINE_CURVE_WITH_KNOTS('',3,(#48252,#48253,#48254,#48255),
 .UNSPECIFIED.,.F.,.F.,(4,4),(-1.29366209142284,-0.119188359258344),
 .UNSPECIFIED.);
#4214=B_SPLINE_CURVE_WITH_KNOTS('',3,(#48392,#48393,#48394,#48395,#48396,
#48397,#48398,#48399,#48400,#48401,#48402,#48403,#48404,#48405,#48406,#48407,
#48408,#48409,#48410,#48411,#48412,#48413),.UNSPECIFIED.,.F.,.F.,(4,3,3,
3,3,3,3,4),(0.,0.569336161400378,0.749177341007451,1.14873589832855,1.30429792490941,
1.39106145779858,1.54578048897719,1.61726052349904),.UNSPECIFIED.);
#4215=B_SPLINE_CURVE_WITH_KNOTS('',3,(#48515,#48516,#48517,#48518,#48519,
#48520,#48521,#48522,#48523,#48524,#48525,#48526,#48527,#48528),
 .UNSPECIFIED.,.F.,.F.,(4,2,2,2,2,2,4),(-1.99248695527052,-1.80900909844907,
-1.62729798972499,-1.17075046205823,-0.668721558372462,-0.361288435792185,
-0.0338550864812489),.UNSPECIFIED.);
#4216=B_SPLINE_CURVE_WITH_KNOTS('',3,(#48529,#48530,#48531,#48532),
 .UNSPECIFIED.,.F.,.F.,(4,4),(0.0499883320126331,0.152208129868745),
 .UNSPECIFIED.);
#4217=B_SPLINE_CURVE_WITH_KNOTS('',3,(#48536,#48537,#48538,#48539),
 .UNSPECIFIED.,.F.,.F.,(4,4),(12.602295500632,15.0893405989718),
 .UNSPECIFIED.);
#4218=B_SPLINE_CURVE_WITH_KNOTS('',3,(#48649,#48650,#48651,#48652),
 .UNSPECIFIED.,.F.,.F.,(4,4),(19.6867712029998,23.2012225962489),
 .UNSPECIFIED.);
#4219=B_SPLINE_CURVE_WITH_KNOTS('',3,(#48654,#48655,#48656,#48657,#48658,
#48659,#48660,#48661,#48662,#48663,#48664,#48665,#48666,#48667,#48668,#48669,
#48670,#48671,#48672,#48673,#48674,#48675,#48676,#48677,#48678,#48679,#48680,
#48681),.UNSPECIFIED.,.F.,.F.,(4,3,3,3,3,3,3,3,3,4),(-4.29295029287552,
-3.67766994705724,-2.97031632412703,-2.37424715288522,-2.00020115328328,
-1.70071199910858,-1.1320234547884,-0.387157778250069,-0.249187079614229,
0.),.UNSPECIFIED.);
#4220=B_SPLINE_CURVE_WITH_KNOTS('',3,(#48683,#48684,#48685,#48686),
 .UNSPECIFIED.,.F.,.F.,(4,4),(-2.25355902969558,-0.8318795023757),
 .UNSPECIFIED.);
#4221=B_SPLINE_CURVE_WITH_KNOTS('',3,(#48687,#48688,#48689,#48690,#48691,
#48692,#48693,#48694,#48695,#48696,#48697,#48698,#48699,#48700,#48701,#48702,
#48703,#48704,#48705,#48706,#48707,#48708,#48709,#48710,#48711,#48712,#48713,
#48714),.UNSPECIFIED.,.F.,.F.,(4,3,3,3,3,3,3,3,3,4),(0.,0.198329530181083,
0.718473337674969,0.921591739443174,1.13394541355614,1.63848434558204,1.82278760043539,
1.95589943946292,2.14302327760794,2.31810070175045),.UNSPECIFIED.);
#4222=B_SPLINE_CURVE_WITH_KNOTS('',3,(#48717,#48718,#48719,#48720),
 .UNSPECIFIED.,.F.,.F.,(4,4),(-0.781276345008619,-0.557585090072962),
 .UNSPECIFIED.);
#4223=B_SPLINE_CURVE_WITH_KNOTS('',3,(#48722,#48723,#48724,#48725),
 .UNSPECIFIED.,.F.,.F.,(4,4),(-1.29366209142284,-0.119188359258344),
 .UNSPECIFIED.);
#4224=B_SPLINE_CURVE_WITH_KNOTS('',3,(#48862,#48863,#48864,#48865,#48866,
#48867,#48868,#48869,#48870,#48871,#48872,#48873,#48874,#48875,#48876,#48877,
#48878,#48879,#48880,#48881,#48882,#48883),.UNSPECIFIED.,.F.,.F.,(4,3,3,
3,3,3,3,4),(0.,0.569336161400378,0.749177341007442,1.14873589832855,1.30429792490947,
1.39106145779861,1.54578048897719,1.61726052349904),.UNSPECIFIED.);
#4225=B_SPLINE_CURVE_WITH_KNOTS('',3,(#48985,#48986,#48987,#48988,#48989,
#48990,#48991,#48992,#48993,#48994,#48995,#48996,#48997,#48998),
 .UNSPECIFIED.,.F.,.F.,(4,2,2,2,2,2,4),(-1.99248695526783,-1.80900909844662,
-1.62729798972286,-1.17075046205687,-0.668721558371707,-0.361288435792094,
-0.0338550864812445),.UNSPECIFIED.);
#4226=B_SPLINE_CURVE_WITH_KNOTS('',3,(#48999,#49000,#49001,#49002),
 .UNSPECIFIED.,.F.,.F.,(4,4),(0.0499883320437557,0.152208130107415),
 .UNSPECIFIED.);
#4227=B_SPLINE_CURVE_WITH_KNOTS('',3,(#49006,#49007,#49008,#49009),
 .UNSPECIFIED.,.F.,.F.,(4,4),(12.6022955008651,15.0893406002079),
 .UNSPECIFIED.);
#4228=B_SPLINE_CURVE_WITH_KNOTS('',3,(#49119,#49120,#49121,#49122),
 .UNSPECIFIED.,.F.,.F.,(4,4),(19.6867712066972,23.2012226007436),
 .UNSPECIFIED.);
#4229=B_SPLINE_CURVE_WITH_KNOTS('',3,(#49124,#49125,#49126,#49127,#49128,
#49129,#49130,#49131,#49132,#49133,#49134,#49135,#49136,#49137,#49138,#49139,
#49140,#49141,#49142,#49143,#49144,#49145,#49146,#49147,#49148,#49149,#49150,
#49151),.UNSPECIFIED.,.F.,.F.,(4,3,3,3,3,3,3,3,3,4),(-4.29295029284741,
-3.67766994703848,-2.97031632412736,-2.37424715288436,-2.00020115322997,
-1.7007119989863,-1.13202345479092,-0.387157778245483,-0.249187079614217,
0.),.UNSPECIFIED.);
#4230=B_SPLINE_CURVE_WITH_KNOTS('',3,(#49153,#49154,#49155,#49156),
 .UNSPECIFIED.,.F.,.F.,(4,4),(-2.25355902969558,-0.8318795023757),
 .UNSPECIFIED.);
#4231=B_SPLINE_CURVE_WITH_KNOTS('',3,(#49157,#49158,#49159,#49160,#49161,
#49162,#49163,#49164,#49165,#49166,#49167,#49168,#49169,#49170,#49171,#49172,
#49173,#49174,#49175,#49176,#49177,#49178,#49179,#49180,#49181,#49182,#49183,
#49184),.UNSPECIFIED.,.F.,.F.,(4,3,3,3,3,3,3,3,3,4),(0.,0.198329530181083,
0.718473337675054,0.921591739443259,1.13394541355614,1.63848434558204,1.82278760043542,
1.95589943946294,2.14302327760794,2.31810070175045),.UNSPECIFIED.);
#4232=B_SPLINE_CURVE_WITH_KNOTS('',3,(#49187,#49188,#49189,#49190),
 .UNSPECIFIED.,.F.,.F.,(4,4),(-1.48004174124428,-1.25625514156074),
 .UNSPECIFIED.);
#4233=B_SPLINE_CURVE_WITH_KNOTS('',3,(#49192,#49193,#49194,#49195),
 .UNSPECIFIED.,.F.,.F.,(4,4),(-1.29366209142284,-0.119188359258344),
 .UNSPECIFIED.);
#4234=B_SPLINE_CURVE_WITH_KNOTS('',3,(#49332,#49333,#49334,#49335,#49336,
#49337,#49338,#49339,#49340,#49341,#49342,#49343,#49344,#49345,#49346,#49347,
#49348,#49349,#49350,#49351,#49352,#49353),.UNSPECIFIED.,.F.,.F.,(4,3,3,
3,3,3,3,4),(0.,0.569336161400378,0.74917734100748,1.14873589832855,1.30429792490946,
1.39106145779859,1.54578048897719,1.61726052349904),.UNSPECIFIED.);
#4235=B_SPLINE_CURVE_WITH_KNOTS('',3,(#49455,#49456,#49457,#49458,#49459,
#49460,#49461,#49462,#49463,#49464,#49465,#49466,#49467,#49468),
 .UNSPECIFIED.,.F.,.F.,(4,2,2,2,2,2,4),(-1.99248695526,-1.80900909843983,
-1.62729798971706,-1.1707504620537,-0.668721558369746,-0.361288435792709,
-0.0338550864812414),.UNSPECIFIED.);
#4236=B_SPLINE_CURVE_WITH_KNOTS('',3,(#49469,#49470,#49471,#49472),
 .UNSPECIFIED.,.F.,.F.,(4,4),(0.0499883320353046,0.152208130042536),
 .UNSPECIFIED.);
#4237=B_SPLINE_CURVE_WITH_KNOTS('',3,(#49476,#49477,#49478,#49479),
 .UNSPECIFIED.,.F.,.F.,(4,4),(12.6022955009377,15.0893406005466),
 .UNSPECIFIED.);
#4238=B_SPLINE_CURVE_WITH_KNOTS('',3,(#49589,#49590,#49591,#49592),
 .UNSPECIFIED.,.F.,.F.,(4,4),(19.6867712047202,23.201222598638),
 .UNSPECIFIED.);
#4239=B_SPLINE_CURVE_WITH_KNOTS('',3,(#49594,#49595,#49596,#49597,#49598,
#49599,#49600,#49601,#49602,#49603,#49604,#49605,#49606,#49607,#49608,#49609,
#49610,#49611,#49612,#49613,#49614,#49615,#49616,#49617,#49618,#49619,#49620,
#49621),.UNSPECIFIED.,.F.,.F.,(4,3,3,3,3,3,3,3,3,4),(-4.29295029281412,
-3.677669947019,-2.9703163241297,-2.37424715288221,-2.00020115321966,-1.70071199896483,
-1.13202345479064,-0.387157778248161,-0.249187079614164,0.),
 .UNSPECIFIED.);
#4240=B_SPLINE_CURVE_WITH_KNOTS('',3,(#49623,#49624,#49625,#49626),
 .UNSPECIFIED.,.F.,.F.,(4,4),(-2.25355902969558,-0.8318795023757),
 .UNSPECIFIED.);
#4241=B_SPLINE_CURVE_WITH_KNOTS('',3,(#49627,#49628,#49629,#49630,#49631,
#49632,#49633,#49634,#49635,#49636,#49637,#49638,#49639,#49640,#49641,#49642,
#49643,#49644,#49645,#49646,#49647,#49648,#49649,#49650,#49651,#49652,#49653,
#49654),.UNSPECIFIED.,.F.,.F.,(4,3,3,3,3,3,3,3,3,4),(0.,0.198329530181083,
0.718473337675014,0.921591739443205,1.13394541355614,1.63848434558204,1.8227876004354,
1.95589943946296,2.14302327760794,2.31810070175045),.UNSPECIFIED.);
#4242=B_SPLINE_CURVE_WITH_KNOTS('',3,(#49657,#49658,#49659,#49660,#49661,
#49662),.UNSPECIFIED.,.F.,.F.,(4,2,4),(-1.24678830233717,-1.23436729644851,
-1.02314392866673),.UNSPECIFIED.);
#4243=B_SPLINE_CURVE_WITH_KNOTS('',3,(#49664,#49665,#49666,#49667),
 .UNSPECIFIED.,.F.,.F.,(4,4),(-1.29366209142284,-0.119188359258344),
 .UNSPECIFIED.);
#4244=B_SPLINE_CURVE_WITH_KNOTS('',3,(#49804,#49805,#49806,#49807,#49808,
#49809,#49810,#49811,#49812,#49813,#49814,#49815,#49816,#49817,#49818,#49819,
#49820,#49821,#49822,#49823,#49824,#49825),.UNSPECIFIED.,.F.,.F.,(4,3,3,
3,3,3,3,4),(0.,0.569336161400378,0.749177341007471,1.14873589832855,1.30429792490946,
1.39106145779861,1.54578048897719,1.61726052349904),.UNSPECIFIED.);
#4245=B_SPLINE_CURVE_WITH_KNOTS('',3,(#49927,#49928,#49929,#49930,#49931,
#49932,#49933,#49934,#49935,#49936,#49937,#49938,#49939,#49940),
 .UNSPECIFIED.,.F.,.F.,(4,2,2,2,2,2,4),(-1.99248695526232,-1.80900909844183,
-1.62729798971886,-1.17075046205496,-0.668721558369855,-0.361288435792721,
-0.0338550864812465),.UNSPECIFIED.);
#4246=B_SPLINE_CURVE_WITH_KNOTS('',3,(#49941,#49942,#49943,#49944),
 .UNSPECIFIED.,.F.,.F.,(4,4),(0.04998833204185,0.152208130092823),
 .UNSPECIFIED.);
#4247=B_SPLINE_CURVE_WITH_KNOTS('',3,(#49948,#49949,#49950,#49951),
 .UNSPECIFIED.,.F.,.F.,(4,4),(12.6022955007997,15.0893405996947),
 .UNSPECIFIED.);
#4248=B_SPLINE_CURVE_WITH_KNOTS('',3,(#50061,#50062,#50063,#50064),
 .UNSPECIFIED.,.F.,.F.,(4,4),(19.6867712021019,23.2012225955095),
 .UNSPECIFIED.);
#4249=B_SPLINE_CURVE_WITH_KNOTS('',3,(#50066,#50067,#50068,#50069,#50070,
#50071,#50072,#50073,#50074,#50075,#50076,#50077,#50078,#50079,#50080,#50081,
#50082,#50083,#50084,#50085,#50086,#50087,#50088,#50089,#50090,#50091,#50092,
#50093),.UNSPECIFIED.,.F.,.F.,(4,3,3,3,3,3,3,3,3,4),(-4.29295029283852,
-3.67766994703207,-2.97031632412226,-2.37424715288117,-2.00020115324444,
-1.70071199902372,-1.1320234547888,-0.387157778246094,-0.249187079614028,
0.),.UNSPECIFIED.);
#4250=B_SPLINE_CURVE_WITH_KNOTS('',3,(#50095,#50096,#50097,#50098),
 .UNSPECIFIED.,.F.,.F.,(4,4),(-2.25355902969558,-0.8318795023757),
 .UNSPECIFIED.);
#4251=B_SPLINE_CURVE_WITH_KNOTS('',3,(#50099,#50100,#50101,#50102,#50103,
#50104,#50105,#50106,#50107,#50108,#50109,#50110,#50111,#50112,#50113,#50114,
#50115,#50116,#50117,#50118,#50119,#50120,#50121,#50122,#50123,#50124,#50125,
#50126),.UNSPECIFIED.,.F.,.F.,(4,3,3,3,3,3,3,3,3,4),(0.,0.198329530181083,
0.718473337675043,0.921591739443273,1.13394541355614,1.63848434558204,1.8227876004354,
1.95589943946294,2.14302327760794,2.31810070175045),.UNSPECIFIED.);
#4252=B_SPLINE_CURVE_WITH_KNOTS('',3,(#50129,#50130,#50131,#50132,#50133,
#50134),.UNSPECIFIED.,.F.,.F.,(4,2,4),(-1.45143148105007,-1.23436729644851,
-1.22796157678455),.UNSPECIFIED.);
#4253=B_SPLINE_CURVE_WITH_KNOTS('',3,(#50136,#50137,#50138,#50139),
 .UNSPECIFIED.,.F.,.F.,(4,4),(-1.29366209142284,-0.119188359258344),
 .UNSPECIFIED.);
#4254=B_SPLINE_CURVE_WITH_KNOTS('',3,(#50276,#50277,#50278,#50279,#50280,
#50281,#50282,#50283,#50284,#50285,#50286,#50287,#50288,#50289,#50290,#50291,
#50292,#50293,#50294,#50295,#50296,#50297),.UNSPECIFIED.,.F.,.F.,(4,3,3,
3,3,3,3,4),(0.,0.569336161400378,0.749177341007454,1.14873589832855,1.30429792490945,
1.39106145779861,1.54578048897719,1.61726052349904),.UNSPECIFIED.);
#4255=B_SPLINE_CURVE_WITH_KNOTS('',3,(#50399,#50400,#50401,#50402,#50403,
#50404,#50405,#50406,#50407,#50408,#50409,#50410,#50411,#50412),
 .UNSPECIFIED.,.F.,.F.,(4,2,2,2,2,2,4),(-1.99248695526215,-1.80900909844175,
-1.62729798971876,-1.17075046205484,-0.66872155836966,-0.361288435792731,
-0.0338550864812428),.UNSPECIFIED.);
#4256=B_SPLINE_CURVE_WITH_KNOTS('',3,(#50413,#50414,#50415,#50416),
 .UNSPECIFIED.,.F.,.F.,(4,4),(0.0499883320345709,0.152208130037191),
 .UNSPECIFIED.);
#4257=B_SPLINE_CURVE_WITH_KNOTS('',3,(#50420,#50421,#50422,#50423),
 .UNSPECIFIED.,.F.,.F.,(4,4),(12.6022955008531,15.0893406000084),
 .UNSPECIFIED.);
#4258=B_SPLINE_CURVE_WITH_KNOTS('',3,(#50533,#50534,#50535,#50536),
 .UNSPECIFIED.,.F.,.F.,(4,4),(19.6867712068538,23.2012226010116),
 .UNSPECIFIED.);
#4259=B_SPLINE_CURVE_WITH_KNOTS('',3,(#50538,#50539,#50540,#50541,#50542,
#50543,#50544,#50545,#50546,#50547,#50548,#50549,#50550,#50551,#50552,#50553,
#50554,#50555,#50556,#50557,#50558,#50559,#50560,#50561,#50562,#50563,#50564,
#50565),.UNSPECIFIED.,.F.,.F.,(4,3,3,3,3,3,3,3,3,4),(-4.29295029283119,
-3.67766994702957,-2.97031632412832,-2.37424715288224,-2.00020115323496,
-1.70071199900048,-1.13202345478954,-0.38715777824571,-0.249187079614159,
0.),.UNSPECIFIED.);
#4260=B_SPLINE_CURVE_WITH_KNOTS('',3,(#50567,#50568,#50569,#50570),
 .UNSPECIFIED.,.F.,.F.,(4,4),(-2.25355902969558,-0.8318795023757),
 .UNSPECIFIED.);
#4261=B_SPLINE_CURVE_WITH_KNOTS('',3,(#50571,#50572,#50573,#50574,#50575,
#50576,#50577,#50578,#50579,#50580,#50581,#50582,#50583,#50584,#50585,#50586,
#50587,#50588,#50589,#50590,#50591,#50592,#50593,#50594,#50595,#50596,#50597,
#50598),.UNSPECIFIED.,.F.,.F.,(4,3,3,3,3,3,3,3,3,4),(0.,0.198329530181083,
0.718473337675035,0.921591739443244,1.13394541355614,1.63848434558204,1.82278760043539,
1.95589943946293,2.14302327760794,2.31810070175045),.UNSPECIFIED.);
#4262=B_SPLINE_CURVE_WITH_KNOTS('',3,(#50601,#50602,#50603,#50604),
 .UNSPECIFIED.,.F.,.F.,(4,4),(-1.47623053088356,-1.25245876190875),
 .UNSPECIFIED.);
#4263=B_SPLINE_CURVE_WITH_KNOTS('',3,(#50606,#50607,#50608,#50609),
 .UNSPECIFIED.,.F.,.F.,(4,4),(-1.29366209142284,-0.119188359258344),
 .UNSPECIFIED.);
#4264=B_SPLINE_CURVE_WITH_KNOTS('',3,(#50746,#50747,#50748,#50749,#50750,
#50751,#50752,#50753,#50754,#50755,#50756,#50757,#50758,#50759,#50760,#50761,
#50762,#50763,#50764,#50765,#50766,#50767),.UNSPECIFIED.,.F.,.F.,(4,3,3,
3,3,3,3,4),(0.,0.569336161400378,0.749177341007436,1.14873589832855,1.30429792490944,
1.39106145779861,1.54578048897719,1.61726052349904),.UNSPECIFIED.);
#4265=B_SPLINE_CURVE_WITH_KNOTS('',3,(#50869,#50870,#50871,#50872,#50873,
#50874,#50875,#50876,#50877,#50878,#50879,#50880,#50881,#50882),
 .UNSPECIFIED.,.F.,.F.,(4,2,2,2,2,2,4),(-1.9924869552618,-1.80900909844148,
-1.62729798971846,-1.17075046205436,-0.668721558370139,-0.361288435792605,
-0.0338550864812418),.UNSPECIFIED.);
#4266=B_SPLINE_CURVE_WITH_KNOTS('',3,(#50883,#50884,#50885,#50886),
 .UNSPECIFIED.,.F.,.F.,(4,4),(0.0499883320206314,0.152208129929869),
 .UNSPECIFIED.);
#4267=B_SPLINE_CURVE_WITH_KNOTS('',3,(#50890,#50891,#50892,#50893),
 .UNSPECIFIED.,.F.,.F.,(4,4),(12.6022955008471,15.0893406001972),
 .UNSPECIFIED.);
#4268=B_SPLINE_CURVE_WITH_KNOTS('',3,(#51002,#51003,#51004,#51005),
 .UNSPECIFIED.,.F.,.F.,(4,4),(19.6867712032198,23.2012225965881),
 .UNSPECIFIED.);
#4269=B_SPLINE_CURVE_WITH_KNOTS('',3,(#51007,#51008,#51009,#51010),
 .UNSPECIFIED.,.F.,.F.,(4,4),(-2.25355902969558,-0.831879502375701),
 .UNSPECIFIED.);
#4270=B_SPLINE_CURVE_WITH_KNOTS('',3,(#51011,#51012,#51013,#51014,#51015,
#51016,#51017,#51018,#51019,#51020,#51021,#51022,#51023,#51024,#51025,#51026,
#51027,#51028,#51029,#51030,#51031,#51032,#51033,#51034,#51035,#51036,#51037,
#51038),.UNSPECIFIED.,.F.,.F.,(4,3,3,3,3,3,3,3,3,4),(0.,0.198329530181083,
0.718473337675014,0.921591739443195,1.13394541355614,1.63848434558204,1.82278760043539,
1.95589943946293,2.14302327760794,2.31810070175045),.UNSPECIFIED.);
#4271=B_SPLINE_CURVE_WITH_KNOTS('',3,(#51041,#51042,#51043,#51044),
 .UNSPECIFIED.,.F.,.F.,(4,4),(-1.29366209142284,-0.119188359258344),
 .UNSPECIFIED.);
#4272=B_SPLINE_CURVE_WITH_KNOTS('',3,(#51181,#51182,#51183,#51184,#51185,
#51186,#51187,#51188,#51189,#51190,#51191,#51192,#51193,#51194,#51195,#51196,
#51197,#51198,#51199,#51200,#51201,#51202),.UNSPECIFIED.,.F.,.F.,(4,3,3,
3,3,3,3,4),(0.,0.569336161400378,0.749177341007455,1.14873589832855,1.30429792490947,
1.39106145779862,1.54578048897719,1.61726052349904),.UNSPECIFIED.);
#4273=B_SPLINE_CURVE_WITH_KNOTS('',3,(#51303,#51304,#51305,#51306),
 .UNSPECIFIED.,.F.,.F.,(4,4),(0.0499883320316304,0.152208130014649),
 .UNSPECIFIED.);
#4274=B_SPLINE_CURVE_WITH_KNOTS('',3,(#51308,#51309,#51310,#51311),
 .UNSPECIFIED.,.F.,.F.,(4,4),(12.60229550093,15.0893406007716),
 .UNSPECIFIED.);
#4275=B_SPLINE_CURVE_WITH_KNOTS('',3,(#51488,#51489,#51490,#51491,#51492,
#51493,#51494,#51495,#51496,#51497,#51498,#51499,#51500,#51501,#51502,#51503,
#51504,#51505,#51506,#51507,#51508,#51509,#51510,#51511,#51512,#51513,#51514,
#51515,#51516,#51517,#51518,#51519,#51520,#51521,#51522,#51523,#51524,#51525,
#51526,#51527,#51528,#51529,#51530,#51531,#51532,#51533),.UNSPECIFIED.,
 .F.,.F.,(4,3,3,3,3,3,3,3,3,3,3,3,3,3,3,4),(-3.56163244824597,-3.30468798711506,
-3.18832863267718,-3.03317964462045,-2.79853132681797,-2.75550071537558,
-2.52404318191444,-2.41525037355583,-2.16219512366447,-1.94576347076795,
-1.75875950761201,-1.34373914266847,-1.06103160840153,-0.696688766667217,
-0.248712120244377,0.),.UNSPECIFIED.);
#4276=B_SPLINE_CURVE_WITH_KNOTS('',3,(#51535,#51536,#51537,#51538,#51539,
#51540),.UNSPECIFIED.,.F.,.F.,(4,2,4),(-1.81367248236635,-1.45004244433882,
-0.253045058252053),.UNSPECIFIED.);
#4277=B_SPLINE_CURVE_WITH_KNOTS('',3,(#51542,#51543,#51544,#51545,#51546,
#51547,#51548,#51549,#51550,#51551,#51552,#51553),.UNSPECIFIED.,.F.,.F.,
(4,2,2,2,2,4),(1.08484844498112,2.49572829361744,3.80512145389228,4.87611899720136,
6.43508432402471,7.63234746756005),.UNSPECIFIED.);
#4278=B_SPLINE_CURVE_WITH_KNOTS('',3,(#51554,#51555,#51556,#51557,#51558,
#51559),.UNSPECIFIED.,.F.,.F.,(4,2,4),(0.,0.791088048129032,1.08484844498112),
 .UNSPECIFIED.);
#4279=B_SPLINE_CURVE_WITH_KNOTS('',3,(#51562,#51563,#51564,#51565,#51566,
#51567),.UNSPECIFIED.,.F.,.F.,(4,2,4),(-0.46225453508618,-0.379477414403806,
-0.20889105167514),.UNSPECIFIED.);
#4280=B_SPLINE_CURVE_WITH_KNOTS('',3,(#51569,#51570,#51571,#51572),
 .UNSPECIFIED.,.F.,.F.,(4,4),(-3.09523587865368,-0.674081646507512),
 .UNSPECIFIED.);
#4281=B_SPLINE_CURVE_WITH_KNOTS('',3,(#51849,#51850,#51851,#51852,#51853,
#51854,#51855,#51856,#51857,#51858,#51859,#51860,#51861,#51862,#51863,#51864,
#51865,#51866,#51867,#51868,#51869,#51870,#51871,#51872,#51873,#51874,#51875,
#51876,#51877,#51878,#51879,#51880,#51881,#51882,#51883,#51884,#51885,#51886,
#51887,#51888,#51889,#51890,#51891,#51892,#51893,#51894),.UNSPECIFIED.,
 .F.,.F.,(4,3,3,3,3,3,3,3,3,3,3,3,3,3,3,4),(0.,0.929985381254847,1.4414618647496,
1.65956723730638,2.03170963890847,2.3019465940753,2.89554149400049,3.67764692687497,
4.06869964331221,4.3263657455837,4.45975235974945,5.09319960112738,5.36523598622997,
5.53913936027952,5.55541982778557,5.8077795608208),.UNSPECIFIED.);
#4282=B_SPLINE_CURVE_WITH_KNOTS('',3,(#52076,#52077,#52078,#52079,#52080,
#52081,#52082,#52083,#52084,#52085,#52086,#52087,#52088,#52089,#52090,#52091,
#52092,#52093,#52094,#52095,#52096,#52097,#52098,#52099,#52100,#52101,#52102,
#52103,#52104,#52105,#52106,#52107,#52108,#52109,#52110,#52111,#52112,#52113,
#52114,#52115,#52116,#52117,#52118,#52119,#52120,#52121,#52122,#52123,#52124,
#52125,#52126,#52127),.UNSPECIFIED.,.F.,.F.,(4,3,3,3,3,3,3,3,3,3,3,3,3,
3,3,3,3,4),(-7.12936283646632,-6.73503957360069,-5.85541917358046,-5.49840246106417,
-4.52430913776898,-4.07614123026294,-3.82946471505583,-3.0419774933968,
-2.81695323655032,-2.47734651704596,-2.09725773516292,-1.90438470328338,
-1.69190045629947,-1.20885650127841,-0.931359575121362,-0.50480048004898,
-0.268904979593478,-0.0293416084169379),.UNSPECIFIED.);
#4283=B_SPLINE_CURVE_WITH_KNOTS('',3,(#52128,#52129,#52130,#52131),
 .UNSPECIFIED.,.F.,.F.,(4,4),(0.0499738748996539,0.152077174914533),
 .UNSPECIFIED.);
#4284=B_SPLINE_CURVE_WITH_KNOTS('',3,(#52310,#52311,#52312,#52313,#52314,
#52315,#52316,#52317,#52318,#52319,#52320,#52321,#52322,#52323,#52324,#52325,
#52326,#52327,#52328,#52329,#52330,#52331,#52332,#52333,#52334,#52335,#52336,
#52337,#52338,#52339,#52340,#52341,#52342,#52343,#52344,#52345,#52346,#52347,
#52348,#52349,#52350,#52351,#52352,#52353,#52354,#52355),.UNSPECIFIED.,
 .F.,.F.,(4,3,3,3,3,3,3,3,3,3,3,3,3,3,3,4),(-3.56163244787668,-3.3046879868165,
-3.18832863247323,-3.03317964444258,-2.79853132694452,-2.75550071530183,
-2.52404318184636,-2.41525037352192,-2.16219512342656,-1.94576347074032,
-1.75875950758838,-1.34373914265465,-1.06103160839068,-0.696688766680895,
-0.248712120243363,0.),.UNSPECIFIED.);
#4285=B_SPLINE_CURVE_WITH_KNOTS('',3,(#52357,#52358,#52359,#52360,#52361,
#52362),.UNSPECIFIED.,.F.,.F.,(4,2,4),(-1.81367248236635,-1.45004244433882,
-0.253045058252053),.UNSPECIFIED.);
#4286=B_SPLINE_CURVE_WITH_KNOTS('',3,(#52364,#52365,#52366,#52367,#52368,
#52369,#52370,#52371,#52372,#52373,#52374,#52375),.UNSPECIFIED.,.F.,.F.,
(4,2,2,2,2,4),(1.08484844498112,2.49572829361744,3.80512145389228,4.87611899720136,
6.43508432402471,7.63234746756005),.UNSPECIFIED.);
#4287=B_SPLINE_CURVE_WITH_KNOTS('',3,(#52376,#52377,#52378,#52379,#52380,
#52381),.UNSPECIFIED.,.F.,.F.,(4,2,4),(0.,0.791088048129032,1.08484844498112),
 .UNSPECIFIED.);
#4288=B_SPLINE_CURVE_WITH_KNOTS('',3,(#52384,#52385,#52386,#52387,#52388,
#52389),.UNSPECIFIED.,.F.,.F.,(4,2,4),(-0.667329469112299,-0.60653547892591,
-0.414285256061857),.UNSPECIFIED.);
#4289=B_SPLINE_CURVE_WITH_KNOTS('',3,(#52391,#52392,#52393,#52394),
 .UNSPECIFIED.,.F.,.F.,(4,4),(-3.09523587865368,-0.674081646507512),
 .UNSPECIFIED.);
#4290=B_SPLINE_CURVE_WITH_KNOTS('',3,(#52671,#52672,#52673,#52674,#52675,
#52676,#52677,#52678,#52679,#52680,#52681,#52682,#52683,#52684,#52685,#52686,
#52687,#52688,#52689,#52690,#52691,#52692,#52693,#52694,#52695,#52696,#52697,
#52698,#52699,#52700,#52701,#52702,#52703,#52704,#52705,#52706,#52707,#52708,
#52709,#52710,#52711,#52712,#52713,#52714,#52715,#52716),.UNSPECIFIED.,
 .F.,.F.,(4,3,3,3,3,3,3,3,3,3,3,3,3,3,3,4),(0.,0.929985381254847,1.44146186475008,
1.65956723730638,2.03170963890849,2.30194659407527,2.89554149400049,3.67764692687497,
4.06869964331221,4.3263657455837,4.45975235974945,5.09319960112738,5.36523598622995,
5.53913936027952,5.55541982778557,5.8077795608208),.UNSPECIFIED.);
#4291=B_SPLINE_CURVE_WITH_KNOTS('',3,(#52928,#52929,#52930,#52931,#52932,
#52933,#52934,#52935,#52936,#52937,#52938,#52939,#52940,#52941,#52942,#52943,
#52944,#52945,#52946,#52947,#52948,#52949,#52950,#52951,#52952,#52953,#52954,
#52955,#52956,#52957,#52958,#52959,#52960,#52961,#52962,#52963,#52964,#52965,
#52966,#52967,#52968,#52969,#52970,#52971,#52972,#52973,#52974,#52975,#52976,
#52977,#52978,#52979),.UNSPECIFIED.,.F.,.F.,(4,3,3,3,3,3,3,3,3,3,3,3,3,
3,3,3,3,4),(-7.129362849605,-6.73503958541797,-5.85541919680017,-5.49840246643452,
-4.52430912729766,-4.07614123495784,-3.82946470458214,-3.04197748709441,
-2.81695323121577,-2.47734651344292,-2.09725773358231,-1.90438470263432,
-1.69190045765133,-1.20885650086995,-0.931359574991274,-0.50480048003591,
-0.268904979566511,-0.0293416084169345),.UNSPECIFIED.);
#4292=B_SPLINE_CURVE_WITH_KNOTS('',3,(#52980,#52981,#52982,#52983),
 .UNSPECIFIED.,.F.,.F.,(4,4),(0.0499738749072504,0.152077174976504),
 .UNSPECIFIED.);
#4293=B_SPLINE_CURVE_WITH_KNOTS('',3,(#53167,#53168,#53169,#53170,#53171,
#53172,#53173,#53174,#53175,#53176,#53177,#53178,#53179,#53180,#53181,#53182,
#53183,#53184,#53185,#53186,#53187,#53188,#53189,#53190,#53191,#53192,#53193,
#53194,#53195,#53196,#53197,#53198,#53199,#53200,#53201,#53202,#53203,#53204,
#53205,#53206,#53207,#53208,#53209,#53210,#53211,#53212),.UNSPECIFIED.,
 .F.,.F.,(4,3,3,3,3,3,3,3,3,3,3,3,3,3,3,4),(-3.56163244831553,-3.30468798717037,
-3.18832863271292,-3.03317964465101,-2.79853132678738,-2.75550071538447,
-2.52404318192142,-2.41525037355563,-2.16219512370471,-1.94576347077165,
-1.75875950761067,-1.34373914266885,-1.06103160840174,-0.69668876667261,
-0.2487121202443,0.),.UNSPECIFIED.);
#4294=B_SPLINE_CURVE_WITH_KNOTS('',3,(#53214,#53215,#53216,#53217,#53218,
#53219),.UNSPECIFIED.,.F.,.F.,(4,2,4),(-1.81367248236635,-1.45004244433882,
-0.253045058252053),.UNSPECIFIED.);
#4295=B_SPLINE_CURVE_WITH_KNOTS('',3,(#53221,#53222,#53223,#53224,#53225,
#53226,#53227,#53228,#53229,#53230,#53231,#53232),.UNSPECIFIED.,.F.,.F.,
(4,2,2,2,2,4),(1.08484844498112,2.49572829361744,3.80512145389228,4.87611899720136,
6.43508432402471,7.63234746756005),.UNSPECIFIED.);
#4296=B_SPLINE_CURVE_WITH_KNOTS('',3,(#53233,#53234,#53235,#53236,#53237,
#53238),.UNSPECIFIED.,.F.,.F.,(4,2,4),(0.,0.791088048129032,1.08484844498112),
 .UNSPECIFIED.);
#4297=B_SPLINE_CURVE_WITH_KNOTS('',3,(#53241,#53242,#53243,#53244,#53245,
#53246),.UNSPECIFIED.,.F.,.F.,(4,2,4),(-0.477412011610917,-0.379477414403805,
-0.22405790136428),.UNSPECIFIED.);
#4298=B_SPLINE_CURVE_WITH_KNOTS('',3,(#53248,#53249,#53250,#53251),
 .UNSPECIFIED.,.F.,.F.,(4,4),(-3.09523587865368,-0.674081646507512),
 .UNSPECIFIED.);
#4299=B_SPLINE_CURVE_WITH_KNOTS('',3,(#53528,#53529,#53530,#53531,#53532,
#53533,#53534,#53535,#53536,#53537,#53538,#53539,#53540,#53541,#53542,#53543,
#53544,#53545,#53546,#53547,#53548,#53549,#53550,#53551,#53552,#53553,#53554,
#53555,#53556,#53557,#53558,#53559,#53560,#53561,#53562,#53563,#53564,#53565,
#53566,#53567,#53568,#53569,#53570,#53571,#53572,#53573),.UNSPECIFIED.,
 .F.,.F.,(4,3,3,3,3,3,3,3,3,3,3,3,3,3,3,4),(0.,0.929985381254847,1.44146186474994,
1.65956723730638,2.03170963890847,2.3019465940753,2.89554149400049,3.67764692687497,
4.06869964331221,4.3263657455837,4.45975235974945,5.09319960112738,5.36523598623069,
5.53913936027934,5.55541982778557,5.8077795608208),.UNSPECIFIED.);
#4300=B_SPLINE_CURVE_WITH_KNOTS('',3,(#53750,#53751,#53752,#53753,#53754,
#53755,#53756,#53757,#53758,#53759,#53760,#53761,#53762,#53763,#53764,#53765,
#53766,#53767,#53768,#53769,#53770,#53771,#53772,#53773,#53774,#53775,#53776,
#53777,#53778,#53779,#53780,#53781,#53782,#53783,#53784,#53785,#53786,#53787,
#53788,#53789,#53790,#53791,#53792,#53793,#53794,#53795,#53796,#53797,#53798,
#53799,#53800,#53801),.UNSPECIFIED.,.F.,.F.,(4,3,3,3,3,3,3,3,3,3,3,3,3,
3,3,3,3,4),(-7.1293628478505,-6.73503958384616,-5.85541919345525,-5.49840246578807,
-4.52430912902298,-4.07614123434755,-3.82946470627502,-3.04197748811397,
-2.81695323207643,-2.47734651402268,-2.09725773383644,-1.90438470273958,
-1.69190045743555,-1.20885650093581,-0.931359575012167,-0.50480048003812,
-0.268904979571344,-0.0293416084169348),.UNSPECIFIED.);
#4301=B_SPLINE_CURVE_WITH_KNOTS('',3,(#53802,#53803,#53804,#53805),
 .UNSPECIFIED.,.F.,.F.,(4,4),(0.0499738749087634,0.152077174988778),
 .UNSPECIFIED.);
#4302=B_SPLINE_CURVE_WITH_KNOTS('',3,(#53984,#53985,#53986,#53987,#53988,
#53989,#53990,#53991,#53992,#53993,#53994,#53995,#53996,#53997,#53998,#53999,
#54000,#54001,#54002,#54003,#54004,#54005,#54006,#54007,#54008,#54009,#54010,
#54011,#54012,#54013,#54014,#54015,#54016,#54017,#54018,#54019,#54020,#54021,
#54022,#54023,#54024,#54025,#54026,#54027,#54028,#54029),.UNSPECIFIED.,
 .F.,.F.,(4,3,3,3,3,3,3,3,3,3,3,3,3,3,3,4),(-3.56163244846089,-3.30468798728467,
-3.1883286327842,-3.03317964471123,-2.79853132670929,-2.75550071539819,
-2.52404318193367,-2.41525037355264,-2.16219512378884,-1.94576347076806,
-1.75875950760639,-1.34373914266426,-1.06103160839798,-0.696688766664339,
-0.248712120244048,0.),.UNSPECIFIED.);
#4303=B_SPLINE_CURVE_WITH_KNOTS('',3,(#54031,#54032,#54033,#54034,#54035,
#54036),.UNSPECIFIED.,.F.,.F.,(4,2,4),(-1.81367248236635,-1.45004244433882,
-0.253045058252053),.UNSPECIFIED.);
#4304=B_SPLINE_CURVE_WITH_KNOTS('',3,(#54038,#54039,#54040,#54041,#54042,
#54043,#54044,#54045,#54046,#54047,#54048,#54049),.UNSPECIFIED.,.F.,.F.,
(4,2,2,2,2,4),(1.08484844498112,2.49572829361744,3.80512145389228,4.87611899720136,
6.43508432402471,7.63234746756005),.UNSPECIFIED.);
#4305=B_SPLINE_CURVE_WITH_KNOTS('',3,(#54050,#54051,#54052,#54053,#54054,
#54055),.UNSPECIFIED.,.F.,.F.,(4,2,4),(0.,0.791088048129032,1.08484844498112),
 .UNSPECIFIED.);
#4306=B_SPLINE_CURVE_WITH_KNOTS('',3,(#54058,#54059,#54060,#54061,#54062,
#54063),.UNSPECIFIED.,.F.,.F.,(4,2,4),(-0.711364948515675,-0.629369591998026,
-0.458258817348068),.UNSPECIFIED.);
#4307=B_SPLINE_CURVE_WITH_KNOTS('',3,(#54065,#54066,#54067,#54068),
 .UNSPECIFIED.,.F.,.F.,(4,4),(-3.09523587865368,-0.674081646507512),
 .UNSPECIFIED.);
#4308=B_SPLINE_CURVE_WITH_KNOTS('',3,(#54345,#54346,#54347,#54348,#54349,
#54350,#54351,#54352,#54353,#54354,#54355,#54356,#54357,#54358,#54359,#54360,
#54361,#54362,#54363,#54364,#54365,#54366,#54367,#54368,#54369,#54370,#54371,
#54372,#54373,#54374,#54375,#54376,#54377,#54378,#54379,#54380,#54381,#54382,
#54383,#54384,#54385,#54386,#54387,#54388,#54389,#54390),.UNSPECIFIED.,
 .F.,.F.,(4,3,3,3,3,3,3,3,3,3,3,3,3,3,3,4),(0.,0.929985381254847,1.441461864751,
1.65956723730638,2.03170963890802,2.30194659407528,2.89554149400049,3.67764692687497,
4.06869964331221,4.3263657455837,4.45975235974945,5.09319960112738,5.36523598622979,
5.53913936027954,5.55541982778557,5.8077795608208),.UNSPECIFIED.);
#4309=B_SPLINE_CURVE_WITH_KNOTS('',3,(#54602,#54603,#54604,#54605,#54606,
#54607,#54608,#54609,#54610,#54611,#54612,#54613,#54614,#54615,#54616,#54617,
#54618,#54619,#54620,#54621,#54622,#54623,#54624,#54625,#54626,#54627,#54628,
#54629,#54630,#54631,#54632,#54633,#54634,#54635,#54636,#54637,#54638,#54639,
#54640,#54641,#54642,#54643,#54644,#54645,#54646,#54647,#54648,#54649,#54650,
#54651,#54652,#54653),.UNSPECIFIED.,.F.,.F.,(4,3,3,3,3,3,3,3,3,3,3,3,3,
3,3,3,3,4),(-7.12936284888383,-6.73503958477952,-5.85541919513442,-5.49840246625061,
-4.52430912838489,-4.07614123472496,-3.82946470561722,-3.04197748771621,
-2.81695323173874,-2.47734651379395,-2.0972577337344,-1.90438470269788,
-1.69190045751967,-1.20885650091009,-0.931359575004032,-0.50480048003733,
-0.268904979571053,-0.0293416084169338),.UNSPECIFIED.);
#4310=B_SPLINE_CURVE_WITH_KNOTS('',3,(#54654,#54655,#54656,#54657),
 .UNSPECIFIED.,.F.,.F.,(4,4),(0.0499738749069921,0.152077174974249),
 .UNSPECIFIED.);
#4311=B_SPLINE_CURVE_WITH_KNOTS('',3,(#54836,#54837,#54838,#54839,#54840,
#54841,#54842,#54843,#54844,#54845,#54846,#54847,#54848,#54849,#54850,#54851,
#54852,#54853,#54854,#54855,#54856,#54857,#54858,#54859,#54860,#54861,#54862,
#54863,#54864,#54865,#54866,#54867,#54868,#54869,#54870,#54871,#54872,#54873,
#54874,#54875,#54876,#54877,#54878,#54879,#54880,#54881),.UNSPECIFIED.,
 .F.,.F.,(4,3,3,3,3,3,3,3,3,3,3,3,3,3,3,4),(-3.56163244787237,-3.30468798681601,
-3.18832863247848,-3.0331796444491,-2.79853132696934,-2.75550071531438,
-2.5240431818579,-2.4152503735364,-2.16219512344052,-1.94576347075244,-1.75875950760127,
-1.34373914266267,-1.06103160839734,-0.696688766676754,-0.248712120244055,
0.),.UNSPECIFIED.);
#4312=B_SPLINE_CURVE_WITH_KNOTS('',3,(#54883,#54884,#54885,#54886,#54887,
#54888),.UNSPECIFIED.,.F.,.F.,(4,2,4),(-1.81367248236635,-1.45004244433882,
-0.253045058252053),.UNSPECIFIED.);
#4313=B_SPLINE_CURVE_WITH_KNOTS('',3,(#54890,#54891,#54892,#54893,#54894,
#54895,#54896,#54897,#54898,#54899,#54900,#54901),.UNSPECIFIED.,.F.,.F.,
(4,2,2,2,2,4),(1.08484844498112,2.49572829361744,3.80512145389228,4.87611899720136,
6.43508432402471,7.63234746756005),.UNSPECIFIED.);
#4314=B_SPLINE_CURVE_WITH_KNOTS('',3,(#54902,#54903,#54904,#54905,#54906,
#54907),.UNSPECIFIED.,.F.,.F.,(4,2,4),(0.,0.791088048129032,1.08484844498112),
 .UNSPECIFIED.);
#4315=B_SPLINE_CURVE_WITH_KNOTS('',3,(#54910,#54911,#54912,#54913,#54914,
#54915),.UNSPECIFIED.,.F.,.F.,(4,2,4),(-0.465430185158785,-0.379477414403806,
-0.212084448966329),.UNSPECIFIED.);
#4316=B_SPLINE_CURVE_WITH_KNOTS('',3,(#54917,#54918,#54919,#54920),
 .UNSPECIFIED.,.F.,.F.,(4,4),(-3.09523587865368,-0.674081646507512),
 .UNSPECIFIED.);
#4317=B_SPLINE_CURVE_WITH_KNOTS('',3,(#55197,#55198,#55199,#55200,#55201,
#55202,#55203,#55204,#55205,#55206,#55207,#55208,#55209,#55210,#55211,#55212,
#55213,#55214,#55215,#55216,#55217,#55218,#55219,#55220,#55221,#55222,#55223,
#55224,#55225,#55226,#55227,#55228,#55229,#55230,#55231,#55232,#55233,#55234,
#55235,#55236,#55237,#55238,#55239,#55240,#55241,#55242),.UNSPECIFIED.,
 .F.,.F.,(4,3,3,3,3,3,3,3,3,3,3,3,3,3,3,4),(0.,0.929985381254847,1.44146186475097,
1.65956723730638,2.03170963890849,2.30194659407532,2.89554149400049,3.67764692687497,
4.06869964331221,4.3263657455837,4.45975235974945,5.09319960112738,5.36523598623038,
5.5391393602794,5.55541982778557,5.8077795608208),.UNSPECIFIED.);
#4318=B_SPLINE_CURVE_WITH_KNOTS('',3,(#55419,#55420,#55421,#55422,#55423,
#55424,#55425,#55426,#55427,#55428,#55429,#55430,#55431,#55432,#55433,#55434,
#55435,#55436,#55437,#55438,#55439,#55440,#55441,#55442,#55443,#55444,#55445,
#55446,#55447,#55448,#55449,#55450,#55451,#55452,#55453,#55454,#55455,#55456,
#55457,#55458,#55459,#55460,#55461,#55462,#55463,#55464,#55465,#55466,#55467,
#55468,#55469,#55470),.UNSPECIFIED.,.F.,.F.,(4,3,3,3,3,3,3,3,3,3,3,3,3,
3,3,3,3,4),(-7.12936285432264,-6.73503958969706,-5.85541920372173,-5.49840246875718,
-4.5243091253641,-4.07614123673017,-3.82946470246266,-3.04197748581819,
-2.81695323012233,-2.47734651269469,-2.0972577332487,-1.90438470249889,
-1.69190045792947,-1.20885650078461,-0.931359574963469,-0.504800480033217,
-0.268904979561171,-0.0293416084169337),.UNSPECIFIED.);
#4319=B_SPLINE_CURVE_WITH_KNOTS('',3,(#55471,#55472,#55473,#55474),
 .UNSPECIFIED.,.F.,.F.,(4,4),(0.0499738749012791,0.152077174927713),
 .UNSPECIFIED.);
#4320=B_SPLINE_CURVE_WITH_KNOTS('',3,(#55653,#55654,#55655,#55656,#55657,
#55658,#55659,#55660,#55661,#55662,#55663,#55664,#55665,#55666,#55667,#55668,
#55669,#55670,#55671,#55672,#55673,#55674,#55675,#55676,#55677,#55678,#55679,
#55680,#55681,#55682,#55683,#55684,#55685,#55686,#55687,#55688,#55689,#55690,
#55691,#55692,#55693,#55694,#55695,#55696,#55697,#55698),.UNSPECIFIED.,
 .F.,.F.,(4,3,3,3,3,3,3,3,3,3,3,3,3,3,3,4),(-3.56163244820022,-3.30468798707926,
-3.18832863265333,-3.03317964460065,-2.79853132683733,-2.75550071536956,
-2.52404318190956,-2.41525037355576,-2.16219512362947,-1.94576347077181,
-1.75875950761541,-1.34373914267237,-1.06103160840431,-0.696688766670289,
-0.248712120244514,0.),.UNSPECIFIED.);
#4321=B_SPLINE_CURVE_WITH_KNOTS('',3,(#55700,#55701,#55702,#55703,#55704,
#55705),.UNSPECIFIED.,.F.,.F.,(4,2,4),(-1.81367248236635,-1.45004244433882,
-0.253045058252053),.UNSPECIFIED.);
#4322=B_SPLINE_CURVE_WITH_KNOTS('',3,(#55707,#55708,#55709,#55710,#55711,
#55712,#55713,#55714,#55715,#55716,#55717,#55718),.UNSPECIFIED.,.F.,.F.,
(4,2,2,2,2,4),(1.08484844498112,2.49572829361744,3.80512145389228,4.87611899720136,
6.43508432402471,7.63234746756005),.UNSPECIFIED.);
#4323=B_SPLINE_CURVE_WITH_KNOTS('',3,(#55719,#55720,#55721,#55722,#55723,
#55724),.UNSPECIFIED.,.F.,.F.,(4,2,4),(0.,0.791088048129032,1.08484844498112),
 .UNSPECIFIED.);
#4324=B_SPLINE_CURVE_WITH_KNOTS('',3,(#55727,#55728,#55729,#55730,#55731,
#55732),.UNSPECIFIED.,.F.,.F.,(4,2,4),(-0.461840180389379,-0.379477414403805,
-0.309127170343164),.UNSPECIFIED.);
#4325=B_SPLINE_CURVE_WITH_KNOTS('',3,(#55734,#55735,#55736,#55737),
 .UNSPECIFIED.,.F.,.F.,(4,4),(-0.562176391928348,-0.461840180389379),
 .UNSPECIFIED.);
#4326=B_SPLINE_CURVE_WITH_KNOTS('',3,(#55739,#55740,#55741,#55742),
 .UNSPECIFIED.,.F.,.F.,(4,4),(-3.09523587865368,-0.674081646507512),
 .UNSPECIFIED.);
#4327=B_SPLINE_CURVE_WITH_KNOTS('',3,(#56019,#56020,#56021,#56022,#56023,
#56024,#56025,#56026,#56027,#56028,#56029,#56030,#56031,#56032,#56033,#56034,
#56035,#56036,#56037,#56038,#56039,#56040,#56041,#56042,#56043,#56044,#56045,
#56046,#56047,#56048,#56049,#56050,#56051,#56052,#56053,#56054,#56055,#56056,
#56057,#56058,#56059,#56060,#56061,#56062,#56063,#56064),.UNSPECIFIED.,
 .F.,.F.,(4,3,3,3,3,3,3,3,3,3,3,3,3,3,3,4),(0.,0.929985381254847,1.44146186474925,
1.65956723730638,2.03170963890846,2.30194659407528,2.89554149400049,3.67764692687497,
4.06869964331221,4.3263657455837,4.45975235974945,5.09319960112738,5.36523598622953,
5.53913936027956,5.55541982778557,5.8077795608208),.UNSPECIFIED.);
#4328=B_SPLINE_CURVE_WITH_KNOTS('',3,(#56245,#56246,#56247,#56248),
 .UNSPECIFIED.,.F.,.F.,(4,4),(-0.172427513903814,-0.0293416084169363),
 .UNSPECIFIED.);
#4329=B_SPLINE_CURVE_WITH_KNOTS('',3,(#56249,#56250,#56251,#56252),
 .UNSPECIFIED.,.F.,.F.,(4,4),(0.0499738748984973,0.152077174905035),
 .UNSPECIFIED.);
#4330=B_SPLINE_CURVE_WITH_KNOTS('',3,(#56539,#56540,#56541,#56542,#56543,
#56544,#56545,#56546,#56547,#56548,#56549,#56550,#56551,#56552,#56553,#56554,
#56555,#56556,#56557,#56558,#56559,#56560,#56561,#56562,#56563,#56564,#56565,
#56566,#56567,#56568,#56569,#56570,#56571,#56572,#56573,#56574,#56575,#56576,
#56577,#56578,#56579,#56580,#56581,#56582,#56583,#56584,#56585,#56586,#56587,
#56588,#56589,#56590),.UNSPECIFIED.,.F.,.F.,(4,3,3,3,3,3,3,3,3,3,3,3,3,
3,3,3,3,4),(-7.12936283895551,-6.73503957583632,-5.85541917810278,-5.49840246204903,
-4.52430913563507,-4.07614123114609,-3.82946471293636,-3.04197749212362,
-2.81695323547345,-2.47734651631999,-2.09725773484647,-1.90438470315448,
-1.69190045657557,-1.20885650119729,-0.931359575096543,-0.504800480046614,
-0.268904979590904,-0.0293416084169361),.UNSPECIFIED.);
#4331=B_SPLINE_CURVE_WITH_KNOTS('',3,(#56592,#56593,#56594,#56595,#56596,
#56597),.UNSPECIFIED.,.F.,.F.,(4,2,4),(-0.427788912726286,-0.283829973314833,
-0.17460945272576),.UNSPECIFIED.);
#4332=B_SPLINE_CURVE_WITH_KNOTS('',3,(#56598,#56599,#56600,#56601,#56602,
#56603,#56604,#56605,#56606,#56607,#56608,#56609,#56610,#56611,#56612,#56613,
#56614,#56615,#56616,#56617,#56618,#56619,#56620,#56621,#56622,#56623,#56624,
#56625),.UNSPECIFIED.,.F.,.F.,(4,3,3,3,3,3,3,3,3,4),(-3.56163244767533,
-3.30468798665615,-3.18832863236903,-3.03317964435316,-2.79853132703271,
-2.75550071527398,-2.5240431818226,-2.41525037351813,-2.15906056771207,
-1.95549230332054),.UNSPECIFIED.);
#4333=B_SPLINE_CURVE_WITH_KNOTS('',3,(#56802,#56803,#56804,#56805,#56806,
#56807),.UNSPECIFIED.,.F.,.F.,(4,2,4),(-1.81367248236635,-1.45004244433882,
-0.253045058252053),.UNSPECIFIED.);
#4334=B_SPLINE_CURVE_WITH_KNOTS('',3,(#56809,#56810,#56811,#56812,#56813,
#56814,#56815,#56816,#56817,#56818,#56819,#56820),.UNSPECIFIED.,.F.,.F.,
(4,2,2,2,2,4),(1.08484844498112,2.49572829361744,3.80512145389228,4.87611899720136,
6.43508432402471,7.63234746756005),.UNSPECIFIED.);
#4335=B_SPLINE_CURVE_WITH_KNOTS('',3,(#56821,#56822,#56823,#56824,#56825,
#56826),.UNSPECIFIED.,.F.,.F.,(4,2,4),(0.,0.791088048129032,1.08484844498112),
 .UNSPECIFIED.);
#4336=B_SPLINE_CURVE_WITH_KNOTS('',3,(#56829,#56830,#56831,#56832),
 .UNSPECIFIED.,.F.,.F.,(4,4),(-3.09523587865368,-0.674081646507512),
 .UNSPECIFIED.);
#4337=B_SPLINE_CURVE_WITH_KNOTS('',3,(#57109,#57110,#57111,#57112,#57113,
#57114,#57115,#57116,#57117,#57118,#57119,#57120,#57121,#57122,#57123,#57124,
#57125,#57126,#57127,#57128,#57129,#57130,#57131,#57132,#57133,#57134,#57135,
#57136,#57137,#57138,#57139,#57140,#57141,#57142,#57143,#57144,#57145,#57146,
#57147,#57148,#57149,#57150,#57151,#57152,#57153,#57154),.UNSPECIFIED.,
 .F.,.F.,(4,3,3,3,3,3,3,3,3,3,3,3,3,3,3,4),(0.,0.929985381254847,1.44146186475013,
1.65956723730638,2.03170963890882,2.30194659407531,2.89554149400049,3.67764692687497,
4.06869964331221,4.3263657455837,4.45975235974945,5.09319960112738,5.36523598623043,
5.5391393602794,5.55541982778557,5.8077795608208),.UNSPECIFIED.);
#4338=B_SPLINE_CURVE_WITH_KNOTS('',3,(#57365,#57366,#57367,#57368),
 .UNSPECIFIED.,.F.,.F.,(4,4),(0.0499738749129155,0.152077175022647),
 .UNSPECIFIED.);
#4339=B_SPLINE_CURVE_WITH_KNOTS('',3,(#57386,#57387,#57388,#57389,#57390,
#57391,#57392),.UNSPECIFIED.,.F.,.F.,(4,3,4),(-0.0308504286108349,-0.027608334705132,
0.),.UNSPECIFIED.);
#4340=B_SPLINE_CURVE_WITH_KNOTS('',3,(#57399,#57400,#57401,#57402,#57403,
#57404),.UNSPECIFIED.,.F.,.F.,(4,2,4),(-0.0558053859643163,-0.0275791003961777,
-0.0249547869966958),.UNSPECIFIED.);
#4341=B_SPLINE_CURVE_WITH_KNOTS('',3,(#57407,#57408,#57409,#57410),
 .UNSPECIFIED.,.F.,.F.,(4,4),(-0.221927025840791,-0.0865063411776193),
 .UNSPECIFIED.);
#4342=B_SPLINE_CURVE_WITH_KNOTS('',3,(#57431,#57432,#57433,#57434),
 .UNSPECIFIED.,.F.,.F.,(4,4),(-0.0621213240389596,-0.0358629876218588),
 .UNSPECIFIED.);
#4343=B_SPLINE_CURVE_WITH_KNOTS('',3,(#57436,#57437,#57438,#57439),
 .UNSPECIFIED.,.F.,.F.,(4,4),(0.0934461854545239,0.23169515901548),
 .UNSPECIFIED.);
#4344=B_SPLINE_CURVE_WITH_KNOTS('',3,(#57441,#57442,#57443,#57444),
 .UNSPECIFIED.,.F.,.F.,(4,4),(-1.,-0.380102179092201),.UNSPECIFIED.);
#4345=B_SPLINE_CURVE_WITH_KNOTS('',3,(#57445,#57446,#57447,#57448),
 .UNSPECIFIED.,.F.,.F.,(4,4),(0.03639808094533,0.0611452087600889),
 .UNSPECIFIED.);
#4346=B_SPLINE_CURVE_WITH_KNOTS('',3,(#57452,#57453,#57454,#57455,#57456,
#57457,#57458),.UNSPECIFIED.,.F.,.F.,(4,3,4),(-0.0308504286108392,-0.0276083347051348,
0.),.UNSPECIFIED.);
#4347=B_SPLINE_CURVE_WITH_KNOTS('',3,(#57465,#57466,#57467,#57468,#57469,
#57470),.UNSPECIFIED.,.F.,.F.,(4,2,4),(-0.0558053859644324,-0.0275791003962552,
-0.0249547869967625),.UNSPECIFIED.);
#4348=B_SPLINE_CURVE_WITH_KNOTS('',3,(#57473,#57474,#57475,#57476),
 .UNSPECIFIED.,.F.,.F.,(4,4),(-0.221927025840791,-0.0865063411776191),
 .UNSPECIFIED.);
#4349=B_SPLINE_CURVE_WITH_KNOTS('',3,(#57497,#57498,#57499,#57500),
 .UNSPECIFIED.,.F.,.F.,(4,4),(-0.0621213249674689,-0.0358629968300687),
 .UNSPECIFIED.);
#4350=B_SPLINE_CURVE_WITH_KNOTS('',3,(#57502,#57503,#57504,#57505),
 .UNSPECIFIED.,.F.,.F.,(4,4),(0.0934461854545238,0.23169515901548),
 .UNSPECIFIED.);
#4351=B_SPLINE_CURVE_WITH_KNOTS('',3,(#57507,#57508,#57509,#57510),
 .UNSPECIFIED.,.F.,.F.,(4,4),(-1.,-0.380102179092223),.UNSPECIFIED.);
#4352=B_SPLINE_CURVE_WITH_KNOTS('',3,(#57511,#57512,#57513,#57514),
 .UNSPECIFIED.,.F.,.F.,(4,4),(-0.0223584778582685,0.),.UNSPECIFIED.);
#4353=B_SPLINE_CURVE_WITH_KNOTS('',3,(#57518,#57519,#57520,#57521,#57522,
#57523,#57524),.UNSPECIFIED.,.F.,.F.,(4,3,4),(-0.0308504286108605,-0.0276083347051509,
0.),.UNSPECIFIED.);
#4354=B_SPLINE_CURVE_WITH_KNOTS('',3,(#57531,#57532,#57533,#57534,#57535,
#57536),.UNSPECIFIED.,.F.,.F.,(4,2,4),(-0.055805384881149,-0.0275402333550594,
-0.0249547910584523),.UNSPECIFIED.);
#4355=B_SPLINE_CURVE_WITH_KNOTS('',3,(#57539,#57540,#57541,#57542),
 .UNSPECIFIED.,.F.,.F.,(4,4),(-0.221927025840791,-0.0865063411776189),
 .UNSPECIFIED.);
#4356=B_SPLINE_CURVE_WITH_KNOTS('',3,(#57563,#57564,#57565,#57566),
 .UNSPECIFIED.,.F.,.F.,(4,4),(-0.0621213333145467,-0.0358630796440704),
 .UNSPECIFIED.);
#4357=B_SPLINE_CURVE_WITH_KNOTS('',3,(#57568,#57569,#57570,#57571),
 .UNSPECIFIED.,.F.,.F.,(4,4),(0.0934461854545234,0.231695159015479),
 .UNSPECIFIED.);
#4358=B_SPLINE_CURVE_WITH_KNOTS('',3,(#57573,#57574,#57575,#57576),
 .UNSPECIFIED.,.F.,.F.,(4,4),(-1.,-0.380102179092208),.UNSPECIFIED.);
#4359=B_SPLINE_CURVE_WITH_KNOTS('',3,(#57577,#57578,#57579,#57580),
 .UNSPECIFIED.,.F.,.F.,(4,4),(-0.0223585244164941,0.),.UNSPECIFIED.);
#4360=B_SPLINE_CURVE_WITH_KNOTS('',3,(#57602,#57603,#57604,#57605,#57606,
#57607),.UNSPECIFIED.,.F.,.F.,(4,2,4),(0.,0.0279210080669517,0.0559552409499635),
 .UNSPECIFIED.);
#4361=B_SPLINE_CURVE_WITH_KNOTS('',3,(#57633,#57634,#57635,#57636),
 .UNSPECIFIED.,.F.,.F.,(4,4),(0.0934461854545252,0.204724982524033),
 .UNSPECIFIED.);
#4362=B_SPLINE_CURVE_WITH_KNOTS('',3,(#57638,#57639,#57640,#57641),
 .UNSPECIFIED.,.F.,.F.,(4,4),(0.12699083482214,0.265239808385091),
 .UNSPECIFIED.);
#4363=B_SPLINE_CURVE_WITH_KNOTS('',3,(#57643,#57644,#57645,#57646),
 .UNSPECIFIED.,.F.,.F.,(4,4),(0.112193136713498,0.12699083482214),
 .UNSPECIFIED.);
#4364=B_SPLINE_CURVE_WITH_KNOTS('',3,(#57649,#57650,#57651,#57652),
 .UNSPECIFIED.,.F.,.F.,(4,4),(0.231695159015479,0.246492857124062),
 .UNSPECIFIED.);
#4365=B_SPLINE_CURVE_WITH_KNOTS('',3,(#57653,#57654,#57655,#57656),
 .UNSPECIFIED.,.F.,.F.,(4,4),(0.153961011313853,0.265239808385092),
 .UNSPECIFIED.);
#4366=B_SPLINE_CURVE_WITH_KNOTS('',3,(#57670,#57671,#57672,#57673,#57674,
#57675,#57676),.UNSPECIFIED.,.F.,.F.,(4,3,4),(-0.0308504286107679,-0.0276083347050827,
0.),.UNSPECIFIED.);
#4367=B_SPLINE_CURVE_WITH_KNOTS('',3,(#57683,#57684,#57685,#57686,#57687,
#57688),.UNSPECIFIED.,.F.,.F.,(4,2,4),(-0.0558053859642229,-0.0275791003961709,
-0.0249547869966901),.UNSPECIFIED.);
#4368=B_SPLINE_CURVE_WITH_KNOTS('',3,(#57691,#57692,#57693,#57694),
 .UNSPECIFIED.,.F.,.F.,(4,4),(-0.221927025840791,-0.0865063411776191),
 .UNSPECIFIED.);
#4369=B_SPLINE_CURVE_WITH_KNOTS('',3,(#57715,#57716,#57717,#57718),
 .UNSPECIFIED.,.F.,.F.,(4,4),(0.0358629876217305,0.0621213240386919),
 .UNSPECIFIED.);
#4370=B_SPLINE_CURVE_WITH_KNOTS('',3,(#57720,#57721,#57722,#57723),
 .UNSPECIFIED.,.F.,.F.,(4,4),(0.0934461854545239,0.23169515901548),
 .UNSPECIFIED.);
#4371=B_SPLINE_CURVE_WITH_KNOTS('',3,(#57725,#57726,#57727,#57728),
 .UNSPECIFIED.,.F.,.F.,(4,4),(-1.,-0.380102179090426),.UNSPECIFIED.);
#4372=B_SPLINE_CURVE_WITH_KNOTS('',3,(#57729,#57730,#57731,#57732),
 .UNSPECIFIED.,.F.,.F.,(4,4),(-0.0611452087602006,-0.036398080945426),
 .UNSPECIFIED.);
#4373=B_SPLINE_CURVE_WITH_KNOTS('',3,(#57750,#57751,#57752,#57753),
 .UNSPECIFIED.,.F.,.F.,(4,4),(-0.272179652662196,-0.136758967898484),
 .UNSPECIFIED.);
#4374=B_SPLINE_CURVE_WITH_KNOTS('',3,(#57755,#57756,#57757,#57758),
 .UNSPECIFIED.,.F.,.F.,(4,4),(0.,0.0223584778581466),.UNSPECIFIED.);
#4375=B_SPLINE_CURVE_WITH_KNOTS('',3,(#57760,#57761,#57762,#57763),
 .UNSPECIFIED.,.F.,.F.,(4,4),(-1.,-0.380102179090391),.UNSPECIFIED.);
#4376=B_SPLINE_CURVE_WITH_KNOTS('',3,(#57764,#57765,#57766,#57767),
 .UNSPECIFIED.,.F.,.F.,(4,4),(0.126990834822138,0.265239808385089),
 .UNSPECIFIED.);
#4377=B_SPLINE_CURVE_WITH_KNOTS('',3,(#57771,#57772,#57773,#57774,#57775,
#57776,#57777),.UNSPECIFIED.,.F.,.F.,(4,3,4),(-0.030850428610866,-0.0276083347051545,
0.),.UNSPECIFIED.);
#4378=B_SPLINE_CURVE_WITH_KNOTS('',3,(#57784,#57785,#57786,#57787,#57788,
#57789),.UNSPECIFIED.,.F.,.F.,(4,2,4),(-0.0558053859639273,-0.0275791003960369,
-0.024954786996575),.UNSPECIFIED.);
#4379=B_SPLINE_CURVE_WITH_KNOTS('',3,(#57791,#57792,#57793,#57794),
 .UNSPECIFIED.,.F.,.F.,(4,4),(-0.221927025840791,-0.0865063411776187),
 .UNSPECIFIED.);
#4380=B_SPLINE_CURVE_WITH_KNOTS('',3,(#57815,#57816,#57817,#57818),
 .UNSPECIFIED.,.F.,.F.,(4,4),(0.0358629968298236,0.0621213249669539),
 .UNSPECIFIED.);
#4381=B_SPLINE_CURVE_WITH_KNOTS('',3,(#57820,#57821,#57822,#57823),
 .UNSPECIFIED.,.F.,.F.,(4,4),(0.0934461854545234,0.231695159015479),
 .UNSPECIFIED.);
#4382=B_SPLINE_CURVE_WITH_KNOTS('',3,(#57824,#57825,#57826,#57827),
 .UNSPECIFIED.,.F.,.F.,(4,4),(-1.,-0.380102179090419),.UNSPECIFIED.);
#4383=B_SPLINE_CURVE_WITH_KNOTS('',3,(#57845,#57846,#57847,#57848),
 .UNSPECIFIED.,.F.,.F.,(4,4),(-0.272179652662199,-0.136758967898488),
 .UNSPECIFIED.);
#4384=B_SPLINE_CURVE_WITH_KNOTS('',3,(#57850,#57851,#57852,#57853),
 .UNSPECIFIED.,.F.,.F.,(4,4),(0.,0.0223585244163726),.UNSPECIFIED.);
#4385=B_SPLINE_CURVE_WITH_KNOTS('',3,(#57855,#57856,#57857,#57858),
 .UNSPECIFIED.,.F.,.F.,(4,4),(-1.,-0.380102179090403),.UNSPECIFIED.);
#4386=B_SPLINE_CURVE_WITH_KNOTS('',3,(#57859,#57860,#57861,#57862),
 .UNSPECIFIED.,.F.,.F.,(4,4),(0.126990834822142,0.265239808385093),
 .UNSPECIFIED.);
#4387=B_SPLINE_CURVE_WITH_KNOTS('',3,(#57866,#57867,#57868,#57869,#57870,
#57871,#57872),.UNSPECIFIED.,.F.,.F.,(4,3,4),(-0.0308504286107312,-0.0276083347050556,
0.),.UNSPECIFIED.);
#4388=B_SPLINE_CURVE_WITH_KNOTS('',3,(#57879,#57880,#57881,#57882,#57883,
#57884),.UNSPECIFIED.,.F.,.F.,(4,2,4),(-0.0558053859644204,-0.0275791003962489,
-0.0249547869967569),.UNSPECIFIED.);
#4389=B_SPLINE_CURVE_WITH_KNOTS('',3,(#57886,#57887,#57888,#57889),
 .UNSPECIFIED.,.F.,.F.,(4,4),(-0.221927025840791,-0.0865063411776193),
 .UNSPECIFIED.);
#4390=B_SPLINE_CURVE_WITH_KNOTS('',3,(#57910,#57911,#57912,#57913),
 .UNSPECIFIED.,.F.,.F.,(4,4),(-0.0621213333145166,-0.0358630796440529),
 .UNSPECIFIED.);
#4391=B_SPLINE_CURVE_WITH_KNOTS('',3,(#57915,#57916,#57917,#57918),
 .UNSPECIFIED.,.F.,.F.,(4,4),(0.093446185454524,0.231695159015479),
 .UNSPECIFIED.);
#4392=B_SPLINE_CURVE_WITH_KNOTS('',3,(#57919,#57920,#57921,#57922),
 .UNSPECIFIED.,.F.,.F.,(4,4),(-1.,-0.38010217909043),.UNSPECIFIED.);
#4393=B_SPLINE_CURVE_WITH_KNOTS('',3,(#57926,#57927,#57928,#57929,#57930,
#57931,#57932),.UNSPECIFIED.,.F.,.F.,(4,3,4),(-0.0308504336262779,-0.0275666040082405,
0.),.UNSPECIFIED.);
#4394=B_SPLINE_CURVE_WITH_KNOTS('',3,(#57939,#57940,#57941,#57942,#57943,
#57944),.UNSPECIFIED.,.F.,.F.,(4,2,4),(-0.0558053859643313,-0.027579100396226,
-0.0249547870387722),.UNSPECIFIED.);
#4395=B_SPLINE_CURVE_WITH_KNOTS('',3,(#57947,#57948,#57949,#57950),
 .UNSPECIFIED.,.F.,.F.,(4,4),(-0.221927025906161,-0.0865063411775655),
 .UNSPECIFIED.);
#4396=B_SPLINE_CURVE_WITH_KNOTS('',3,(#57970,#57971,#57972,#57973),
 .UNSPECIFIED.,.F.,.F.,(4,4),(-0.0299494398134785,0.),.UNSPECIFIED.);
#4397=B_SPLINE_CURVE_WITH_KNOTS('',3,(#57974,#57975,#57976,#57977,#57978,
#57979),.UNSPECIFIED.,.F.,.F.,(4,2,4),(0.,0.0280015594495552,0.0559551731920623),
 .UNSPECIFIED.);
#4398=B_SPLINE_CURVE_WITH_KNOTS('',3,(#57997,#57998,#57999,#58000),
 .UNSPECIFIED.,.F.,.F.,(4,4),(-0.272179652662197,-0.136758967898486),
 .UNSPECIFIED.);
#4399=B_SPLINE_CURVE_WITH_KNOTS('',3,(#58002,#58003,#58004,#58005),
 .UNSPECIFIED.,.F.,.F.,(4,4),(-0.0611452087600435,-0.036398080945399),
 .UNSPECIFIED.);
#4400=B_SPLINE_CURVE_WITH_KNOTS('',3,(#58006,#58007,#58008,#58009),
 .UNSPECIFIED.,.F.,.F.,(4,4),(-1.,-0.380102179090411),.UNSPECIFIED.);
#4401=B_SPLINE_CURVE_WITH_KNOTS('',3,(#58013,#58014,#58015,#58016,#58017,
#58018,#58019),.UNSPECIFIED.,.F.,.F.,(4,3,4),(-0.0308504286108225,-0.0276083347051228,
0.),.UNSPECIFIED.);
#4402=B_SPLINE_CURVE_WITH_KNOTS('',3,(#58026,#58027,#58028,#58029,#58030,
#58031),.UNSPECIFIED.,.F.,.F.,(4,2,4),(-0.0558053859642228,-0.0275791003961684,
-0.0249547869966877),.UNSPECIFIED.);
#4403=B_SPLINE_CURVE_WITH_KNOTS('',3,(#58033,#58034,#58035,#58036),
 .UNSPECIFIED.,.F.,.F.,(4,4),(-0.221927025840792,-0.0865063411776193),
 .UNSPECIFIED.);
#4404=B_SPLINE_CURVE_WITH_KNOTS('',3,(#58057,#58058,#58059,#58060),
 .UNSPECIFIED.,.F.,.F.,(4,4),(0.0358629876219686,0.0621213240391899),
 .UNSPECIFIED.);
#4405=B_SPLINE_CURVE_WITH_KNOTS('',3,(#58062,#58063,#58064,#58065),
 .UNSPECIFIED.,.F.,.F.,(4,4),(0.0934461854545239,0.23169515901548),
 .UNSPECIFIED.);
#4406=B_SPLINE_CURVE_WITH_KNOTS('',3,(#58066,#58067,#58068,#58069),
 .UNSPECIFIED.,.F.,.F.,(4,4),(-1.,-0.380102179090436),.UNSPECIFIED.);
#4407=B_SPLINE_CURVE_WITH_KNOTS('',3,(#58087,#58088,#58089,#58090),
 .UNSPECIFIED.,.F.,.F.,(4,4),(-0.272179652662196,-0.136758967898484),
 .UNSPECIFIED.);
#4408=B_SPLINE_CURVE_WITH_KNOTS('',3,(#58092,#58093,#58094,#58095),
 .UNSPECIFIED.,.F.,.F.,(4,4),(0.,0.0223584778581942),.UNSPECIFIED.);
#4409=B_SPLINE_CURVE_WITH_KNOTS('',3,(#58097,#58098,#58099,#58100),
 .UNSPECIFIED.,.F.,.F.,(4,4),(-1.,-0.380102179090398),.UNSPECIFIED.);
#4410=B_SPLINE_CURVE_WITH_KNOTS('',3,(#58101,#58102,#58103,#58104),
 .UNSPECIFIED.,.F.,.F.,(4,4),(0.126990834822138,0.265239808385089),
 .UNSPECIFIED.);
#4411=B_SPLINE_CURVE_WITH_KNOTS('',3,(#58108,#58109,#58110,#58111,#58112,
#58113,#58114),.UNSPECIFIED.,.F.,.F.,(4,3,4),(-0.0308504286108342,-0.0276083347051315,
0.),.UNSPECIFIED.);
#4412=B_SPLINE_CURVE_WITH_KNOTS('',3,(#58121,#58122,#58123,#58124,#58125,
#58126),.UNSPECIFIED.,.F.,.F.,(4,2,4),(-0.0558053859641433,-0.0275791003961202,
-0.0249547869966467),.UNSPECIFIED.);
#4413=B_SPLINE_CURVE_WITH_KNOTS('',3,(#58128,#58129,#58130,#58131),
 .UNSPECIFIED.,.F.,.F.,(4,4),(-0.221927025840791,-0.0865063411776189),
 .UNSPECIFIED.);
#4414=B_SPLINE_CURVE_WITH_KNOTS('',3,(#58152,#58153,#58154,#58155),
 .UNSPECIFIED.,.F.,.F.,(4,4),(0.0358629968298035,0.0621213249668936),
 .UNSPECIFIED.);
#4415=B_SPLINE_CURVE_WITH_KNOTS('',3,(#58157,#58158,#58159,#58160),
 .UNSPECIFIED.,.F.,.F.,(4,4),(0.0934461854545236,0.231695159015479),
 .UNSPECIFIED.);
#4416=B_SPLINE_CURVE_WITH_KNOTS('',3,(#58161,#58162,#58163,#58164),
 .UNSPECIFIED.,.F.,.F.,(4,4),(-1.,-0.380102179090424),.UNSPECIFIED.);
#4417=B_SPLINE_CURVE_WITH_KNOTS('',3,(#58182,#58183,#58184,#58185),
 .UNSPECIFIED.,.F.,.F.,(4,4),(-0.2721796526622,-0.136758967898487),
 .UNSPECIFIED.);
#4418=B_SPLINE_CURVE_WITH_KNOTS('',3,(#58187,#58188,#58189,#58190),
 .UNSPECIFIED.,.F.,.F.,(4,4),(0.,0.0223585244163923),.UNSPECIFIED.);
#4419=B_SPLINE_CURVE_WITH_KNOTS('',3,(#58192,#58193,#58194,#58195),
 .UNSPECIFIED.,.F.,.F.,(4,4),(-1.,-0.380102179090384),.UNSPECIFIED.);
#4420=B_SPLINE_CURVE_WITH_KNOTS('',3,(#58196,#58197,#58198,#58199),
 .UNSPECIFIED.,.F.,.F.,(4,4),(0.126990834822142,0.265239808385093),
 .UNSPECIFIED.);
#4421=B_SPLINE_CURVE_WITH_KNOTS('',3,(#58203,#58204,#58205,#58206,#58207,
#58208,#58209),.UNSPECIFIED.,.F.,.F.,(4,3,4),(-0.0308504286108346,-0.0276083347051322,
0.),.UNSPECIFIED.);
#4422=B_SPLINE_CURVE_WITH_KNOTS('',3,(#58216,#58217,#58218,#58219,#58220,
#58221),.UNSPECIFIED.,.F.,.F.,(4,2,4),(-0.055805385964261,-0.0275791003961853,
-0.0249547869967028),.UNSPECIFIED.);
#4423=B_SPLINE_CURVE_WITH_KNOTS('',3,(#58223,#58224,#58225,#58226),
 .UNSPECIFIED.,.F.,.F.,(4,4),(-0.221927025840791,-0.0865063411776194),
 .UNSPECIFIED.);
#4424=B_SPLINE_CURVE_WITH_KNOTS('',3,(#58247,#58248,#58249,#58250),
 .UNSPECIFIED.,.F.,.F.,(4,4),(0.0358630796439579,0.0621213333143259),
 .UNSPECIFIED.);
#4425=B_SPLINE_CURVE_WITH_KNOTS('',3,(#58252,#58253,#58254,#58255),
 .UNSPECIFIED.,.F.,.F.,(4,4),(0.0934461854545242,0.23169515901548),
 .UNSPECIFIED.);
#4426=B_SPLINE_CURVE_WITH_KNOTS('',3,(#58256,#58257,#58258,#58259),
 .UNSPECIFIED.,.F.,.F.,(4,4),(-1.,-0.380102179090412),.UNSPECIFIED.);
#4427=B_SPLINE_CURVE_WITH_KNOTS('',3,(#58276,#58277,#58278,#58279),
 .UNSPECIFIED.,.F.,.F.,(4,4),(-0.272179652662197,-0.136758967898484),
 .UNSPECIFIED.);
#4428=B_SPLINE_CURVE_WITH_KNOTS('',3,(#58281,#58282,#58283,#58284),
 .UNSPECIFIED.,.F.,.F.,(4,4),(-1.,-0.380102179090404),.UNSPECIFIED.);
#4429=B_SPLINE_CURVE_WITH_KNOTS('',3,(#58285,#58286,#58287,#58288),
 .UNSPECIFIED.,.F.,.F.,(4,4),(0.126990834822139,0.26523980838509),
 .UNSPECIFIED.);
#4430=B_SPLINE_CURVE_WITH_KNOTS('',3,(#58306,#58307,#58308,#58309),
 .UNSPECIFIED.,.F.,.F.,(4,4),(0.231695159015479,0.246492857124062),
 .UNSPECIFIED.);
#4431=B_SPLINE_CURVE_WITH_KNOTS('',3,(#58311,#58312,#58313,#58314),
 .UNSPECIFIED.,.F.,.F.,(4,4),(0.,0.000438960297707012),.UNSPECIFIED.);
#4432=B_SPLINE_CURVE_WITH_KNOTS('',3,(#58315,#58316,#58317,#58318,#58319,
#58320,#58321),.UNSPECIFIED.,.F.,.F.,(4,3,4),(0.0223585244163726,0.0288578077806512,
0.0552143212839845),.UNSPECIFIED.);
#4433=B_SPLINE_CURVE_WITH_KNOTS('',3,(#58339,#58340,#58341,#58342),
 .UNSPECIFIED.,.F.,.F.,(4,4),(0.231695159015479,0.246492857124062),
 .UNSPECIFIED.);
#4434=B_SPLINE_CURVE_WITH_KNOTS('',3,(#58344,#58345,#58346,#58347),
 .UNSPECIFIED.,.F.,.F.,(4,4),(0.,0.000438960191917479),.UNSPECIFIED.);
#4435=B_SPLINE_CURVE_WITH_KNOTS('',3,(#58348,#58349,#58350,#58351,#58352,
#58353,#58354),.UNSPECIFIED.,.F.,.F.,(4,3,4),(0.0223584778581466,0.028857534403892,
0.0552146089787789),.UNSPECIFIED.);
#4436=B_SPLINE_CURVE_WITH_KNOTS('',3,(#58372,#58373,#58374,#58375),
 .UNSPECIFIED.,.F.,.F.,(4,4),(0.23169515901548,0.246492857124062),
 .UNSPECIFIED.);
#4437=B_SPLINE_CURVE_WITH_KNOTS('',3,(#58377,#58378,#58379,#58380),
 .UNSPECIFIED.,.F.,.F.,(4,4),(0.,0.000438960107757425),.UNSPECIFIED.);
#4438=B_SPLINE_CURVE_WITH_KNOTS('',3,(#58381,#58382,#58383,#58384,#58385,
#58386,#58387),.UNSPECIFIED.,.F.,.F.,(4,3,4),(-0.036398080945426,-0.0291445555386541,
-0.000145193969552124),.UNSPECIFIED.);
#4439=B_SPLINE_CURVE_WITH_KNOTS('',3,(#58405,#58406,#58407,#58408),
 .UNSPECIFIED.,.F.,.F.,(4,4),(0.23169515901548,0.246492857124062),
 .UNSPECIFIED.);
#4440=B_SPLINE_CURVE_WITH_KNOTS('',3,(#58410,#58411,#58412,#58413),
 .UNSPECIFIED.,.F.,.F.,(4,4),(0.,0.00043896029770756),.UNSPECIFIED.);
#4441=B_SPLINE_CURVE_WITH_KNOTS('',3,(#58414,#58415,#58416,#58417,#58418,
#58419,#58420),.UNSPECIFIED.,.F.,.F.,(4,3,4),(0.0223585244163923,0.0288578077807066,
0.0552143212841931),.UNSPECIFIED.);
#4442=B_SPLINE_CURVE_WITH_KNOTS('',3,(#58438,#58439,#58440,#58441),
 .UNSPECIFIED.,.F.,.F.,(4,4),(0.231695159015479,0.246492857124062),
 .UNSPECIFIED.);
#4443=B_SPLINE_CURVE_WITH_KNOTS('',3,(#58443,#58444,#58445,#58446),
 .UNSPECIFIED.,.F.,.F.,(4,4),(0.,0.00043896019191799),.UNSPECIFIED.);
#4444=B_SPLINE_CURVE_WITH_KNOTS('',3,(#58447,#58448,#58449,#58450,#58451,
#58452,#58453),.UNSPECIFIED.,.F.,.F.,(4,3,4),(0.0223584778581942,0.0288575344040074,
0.0552146089787722),.UNSPECIFIED.);
#4445=B_SPLINE_CURVE_WITH_KNOTS('',3,(#58471,#58472,#58473,#58474),
 .UNSPECIFIED.,.F.,.F.,(4,4),(0.23169515901548,0.246492857124063),
 .UNSPECIFIED.);
#4446=B_SPLINE_CURVE_WITH_KNOTS('',3,(#58476,#58477,#58478,#58479),
 .UNSPECIFIED.,.F.,.F.,(4,4),(0.,0.000438960107757499),.UNSPECIFIED.);
#4447=B_SPLINE_CURVE_WITH_KNOTS('',3,(#58480,#58481,#58482,#58483,#58484,
#58485,#58486),.UNSPECIFIED.,.F.,.F.,(4,3,4),(-0.036398080945399,-0.0291445555386185,
-0.000145193969552187),.UNSPECIFIED.);
#4448=B_SPLINE_CURVE_WITH_KNOTS('',3,(#58503,#58504,#58505,#58506),
 .UNSPECIFIED.,.F.,.F.,(4,4),(-0.272179652662197,-0.136758967898485),
 .UNSPECIFIED.);
#4449=B_SPLINE_CURVE_WITH_KNOTS('',3,(#58508,#58509,#58510,#58511),
 .UNSPECIFIED.,.F.,.F.,(4,4),(-1.,-0.380102179092181),.UNSPECIFIED.);
#4450=B_SPLINE_CURVE_WITH_KNOTS('',3,(#58512,#58513,#58514,#58515),
 .UNSPECIFIED.,.F.,.F.,(4,4),(0.12699083482214,0.26523980838509),
 .UNSPECIFIED.);
#4451=B_SPLINE_CURVE_WITH_KNOTS('',3,(#58533,#58534,#58535,#58536),
 .UNSPECIFIED.,.F.,.F.,(4,4),(0.23169515901548,0.246492857124062),
 .UNSPECIFIED.);
#4452=B_SPLINE_CURVE_WITH_KNOTS('',3,(#58538,#58539,#58540,#58541),
 .UNSPECIFIED.,.F.,.F.,(4,4),(2.71050543121376E-20,0.00043896010775766),
 .UNSPECIFIED.);
#4453=B_SPLINE_CURVE_WITH_KNOTS('',3,(#58542,#58543,#58544,#58545,#58546,
#58547,#58548),.UNSPECIFIED.,.F.,.F.,(4,3,4),(0.000145193969552055,0.0291445555386256,
0.03639808094533),.UNSPECIFIED.);
#4454=B_SPLINE_CURVE_WITH_KNOTS('',3,(#58565,#58566,#58567,#58568),
 .UNSPECIFIED.,.F.,.F.,(4,4),(-0.272179652662198,-0.136758967898486),
 .UNSPECIFIED.);
#4455=B_SPLINE_CURVE_WITH_KNOTS('',3,(#58570,#58571,#58572,#58573),
 .UNSPECIFIED.,.F.,.F.,(4,4),(-1.,-0.380102179092193),.UNSPECIFIED.);
#4456=B_SPLINE_CURVE_WITH_KNOTS('',3,(#58574,#58575,#58576,#58577),
 .UNSPECIFIED.,.F.,.F.,(4,4),(0.12699083482214,0.265239808385091),
 .UNSPECIFIED.);
#4457=B_SPLINE_CURVE_WITH_KNOTS('',3,(#58595,#58596,#58597,#58598),
 .UNSPECIFIED.,.F.,.F.,(4,4),(0.23169515901548,0.246492857124063),
 .UNSPECIFIED.);
#4458=B_SPLINE_CURVE_WITH_KNOTS('',3,(#58600,#58601,#58602,#58603),
 .UNSPECIFIED.,.F.,.F.,(4,4),(0.,0.000438960191917556),.UNSPECIFIED.);
#4459=B_SPLINE_CURVE_WITH_KNOTS('',3,(#58604,#58605,#58606,#58607,#58608,
#58609,#58610),.UNSPECIFIED.,.F.,.F.,(4,3,4),(-0.055214608979223,-0.0288575344040253,
-0.0223584778582685),.UNSPECIFIED.);
#4460=B_SPLINE_CURVE_WITH_KNOTS('',3,(#58627,#58628,#58629,#58630),
 .UNSPECIFIED.,.F.,.F.,(4,4),(-0.272179652662197,-0.136758967898485),
 .UNSPECIFIED.);
#4461=B_SPLINE_CURVE_WITH_KNOTS('',3,(#58632,#58633,#58634,#58635),
 .UNSPECIFIED.,.F.,.F.,(4,4),(-1.,-0.380102179092185),.UNSPECIFIED.);
#4462=B_SPLINE_CURVE_WITH_KNOTS('',3,(#58636,#58637,#58638,#58639),
 .UNSPECIFIED.,.F.,.F.,(4,4),(0.12699083482214,0.26523980838509),
 .UNSPECIFIED.);
#4463=B_SPLINE_CURVE_WITH_KNOTS('',3,(#58657,#58658,#58659,#58660),
 .UNSPECIFIED.,.F.,.F.,(4,4),(0.,0.000438960297707225),.UNSPECIFIED.);
#4464=B_SPLINE_CURVE_WITH_KNOTS('',3,(#58661,#58662,#58663,#58664,#58665,
#58666,#58667),.UNSPECIFIED.,.F.,.F.,(4,3,4),(-0.0552143212843298,-0.0288578077807816,
-0.0223585244164941),.UNSPECIFIED.);
#4465=B_SPLINE_CURVE_WITH_KNOTS('',3,(#58684,#58685,#58686,#58687),
 .UNSPECIFIED.,.F.,.F.,(4,4),(-0.272179652662254,-0.136758967931396),
 .UNSPECIFIED.);
#4466=B_SPLINE_CURVE_WITH_KNOTS('',3,(#58705,#58706,#58707,#58708),
 .UNSPECIFIED.,.F.,.F.,(4,4),(0.149113104129392,0.14946619853298),
 .UNSPECIFIED.);
#4467=B_SPLINE_CURVE_WITH_KNOTS('',3,(#58709,#58710,#58711,#58712),
 .UNSPECIFIED.,.F.,.F.,(4,4),(0.112193136713498,0.12699083482214),
 .UNSPECIFIED.);
#4468=B_SPLINE_CURVE_WITH_KNOTS('',3,(#58730,#58731,#58732,#58733),
 .UNSPECIFIED.,.F.,.F.,(4,4),(0.149111564070519,0.149464659958529),
 .UNSPECIFIED.);
#4469=B_SPLINE_CURVE_WITH_KNOTS('',3,(#58734,#58735,#58736,#58737),
 .UNSPECIFIED.,.F.,.F.,(4,4),(0.112193136713498,0.12699083482214),
 .UNSPECIFIED.);
#4470=B_SPLINE_CURVE_WITH_KNOTS('',3,(#58755,#58756,#58757,#58758),
 .UNSPECIFIED.,.F.,.F.,(4,4),(0.149109634661021,0.149462732410104),
 .UNSPECIFIED.);
#4471=B_SPLINE_CURVE_WITH_KNOTS('',3,(#58759,#58760,#58761,#58762),
 .UNSPECIFIED.,.F.,.F.,(4,4),(0.112193136713498,0.12699083482214),
 .UNSPECIFIED.);
#4472=B_SPLINE_CURVE_WITH_KNOTS('',3,(#58779,#58780,#58781,#58782),
 .UNSPECIFIED.,.F.,.F.,(4,4),(0.149109634661038,0.149462732410121),
 .UNSPECIFIED.);
#4473=B_SPLINE_CURVE_WITH_KNOTS('',3,(#58800,#58801,#58802,#58803),
 .UNSPECIFIED.,.F.,.F.,(4,4),(0.149111564070538,0.149464659958548),
 .UNSPECIFIED.);
#4474=B_SPLINE_CURVE_WITH_KNOTS('',3,(#58804,#58805,#58806,#58807),
 .UNSPECIFIED.,.F.,.F.,(4,4),(0.112193136713496,0.126990834822138),
 .UNSPECIFIED.);
#4475=B_SPLINE_CURVE_WITH_KNOTS('',3,(#58825,#58826,#58827,#58828),
 .UNSPECIFIED.,.F.,.F.,(4,4),(0.149113104129386,0.149466198532974),
 .UNSPECIFIED.);
#4476=B_SPLINE_CURVE_WITH_KNOTS('',3,(#58829,#58830,#58831,#58832),
 .UNSPECIFIED.,.F.,.F.,(4,4),(0.1121931367135,0.126990834822142),
 .UNSPECIFIED.);
#4477=B_SPLINE_CURVE_WITH_KNOTS('',3,(#58850,#58851,#58852,#58853),
 .UNSPECIFIED.,.F.,.F.,(4,4),(0.14910963466104,0.149462732410123),
 .UNSPECIFIED.);
#4478=B_SPLINE_CURVE_WITH_KNOTS('',3,(#58854,#58855,#58856,#58857),
 .UNSPECIFIED.,.F.,.F.,(4,4),(0.112193136713497,0.126990834822139),
 .UNSPECIFIED.);
#4479=B_SPLINE_CURVE_WITH_KNOTS('',3,(#58875,#58876,#58877,#58878),
 .UNSPECIFIED.,.F.,.F.,(4,4),(0.149111564070554,0.149464659958564),
 .UNSPECIFIED.);
#4480=B_SPLINE_CURVE_WITH_KNOTS('',3,(#58879,#58880,#58881,#58882),
 .UNSPECIFIED.,.F.,.F.,(4,4),(0.112193136713496,0.126990834822138),
 .UNSPECIFIED.);
#4481=B_SPLINE_CURVE_WITH_KNOTS('',3,(#58900,#58901,#58902,#58903),
 .UNSPECIFIED.,.F.,.F.,(4,4),(0.149113104129403,0.149466198532991),
 .UNSPECIFIED.);
#4482=B_SPLINE_CURVE_WITH_KNOTS('',3,(#58904,#58905,#58906,#58907),
 .UNSPECIFIED.,.F.,.F.,(4,4),(0.112193136713501,0.126990834822142),
 .UNSPECIFIED.);
#4483=B_SPLINE_CURVE_WITH_KNOTS('',3,(#59035,#59036,#59037,#59038,#59039,
#59040,#59041,#59042,#59043,#59044,#59045,#59046,#59047,#59048,#59049,#59050,
#59051,#59052),.UNSPECIFIED.,.F.,.F.,(4,2,2,2,2,2,2,2,4),(0.165944509231404,
0.207430432450317,0.24891635566923,0.290402687066019,0.331889018462808,
0.373375349859597,0.414861681256386,0.456347604475299,0.497833527694212),
 .UNSPECIFIED.);
#4484=B_SPLINE_CURVE_WITH_KNOTS('',3,(#59053,#59054,#59055,#59056,#59057,
#59058,#59059,#59060,#59061,#59062,#59063,#59064,#59065,#59066,#59067,#59068,
#59069,#59070,#59071),.UNSPECIFIED.,.F.,.F.,(4,2,2,2,3,2,2,2,4),(0.497833527694212,
0.539319450913125,0.580805374132038,0.622291705528827,0.663778036925616,
0.705264368322405,0.746750699719194,0.788236622938107,0.82972254615702),
 .UNSPECIFIED.);
#4485=B_SPLINE_CURVE_WITH_KNOTS('',3,(#59075,#59076,#59077,#59078,#59079,
#59080,#59081,#59082,#59083,#59084),.UNSPECIFIED.,.F.,.F.,(4,2,2,2,4),(0.,
0.0415565701679523,0.0831131403359046,0.12466741609854,0.166221691861175),
 .UNSPECIFIED.);
#4486=B_SPLINE_CURVE_WITH_KNOTS('',3,(#59085,#59086,#59087,#59088,#59089,
#59090,#59091,#59092,#59093,#59094,#59095,#59096,#59097,#59098,#59099,#59100,
#59101,#59102,#59103,#59104,#59105,#59106,#59107,#59108,#59109,#59110),
 .UNSPECIFIED.,.F.,.F.,(4,2,2,2,2,2,2,2,2,2,2,2,4),(0.166221691861175,0.20777596762381,
0.249330243386446,0.290886813554398,0.33244338372235,0.373999953890303,
0.415556524058255,0.45711079982089,0.498665075583526,0.540219351346161,
0.581773627108796,0.623330197276748,0.664886767444701),.UNSPECIFIED.);
#4487=B_SPLINE_CURVE_WITH_KNOTS('',3,(#59114,#59115,#59116,#59117,#59118,
#59119,#59120,#59121,#59122,#59123,#59124,#59125,#59126,#59127,#59128,#59129,
#59130,#59131),.UNSPECIFIED.,.F.,.F.,(4,2,2,2,2,2,2,2,4),(0.165944509231404,
0.207430432450317,0.24891635566923,0.290402687066019,0.331889018462808,
0.373375349859597,0.414861681256386,0.456347604475299,0.497833527694212),
 .UNSPECIFIED.);
#4488=B_SPLINE_CURVE_WITH_KNOTS('',3,(#59132,#59133,#59134,#59135,#59136,
#59137,#59138,#59139,#59140,#59141,#59142,#59143,#59144,#59145,#59146,#59147,
#59148,#59149,#59150),.UNSPECIFIED.,.F.,.F.,(4,2,2,2,3,2,2,2,4),(0.497833527694212,
0.539319450913125,0.580805374132038,0.622291705528827,0.663778036925616,
0.705264368322405,0.746750699719194,0.788236622938107,0.82972254615702),
 .UNSPECIFIED.);
#4489=B_SPLINE_CURVE_WITH_KNOTS('',3,(#59154,#59155,#59156,#59157,#59158,
#59159,#59160,#59161,#59162,#59163),.UNSPECIFIED.,.F.,.F.,(4,2,2,2,4),(0.,
0.0415565701679523,0.0831131403359046,0.12466741609854,0.166221691861175),
 .UNSPECIFIED.);
#4490=B_SPLINE_CURVE_WITH_KNOTS('',3,(#59164,#59165,#59166,#59167,#59168,
#59169,#59170,#59171,#59172,#59173,#59174,#59175,#59176,#59177,#59178,#59179,
#59180,#59181,#59182,#59183,#59184,#59185,#59186,#59187,#59188,#59189),
 .UNSPECIFIED.,.F.,.F.,(4,2,2,2,2,2,2,2,2,2,2,2,4),(0.166221691861175,0.20777596762381,
0.249330243386446,0.290886813554398,0.33244338372235,0.373999953890303,
0.415556524058255,0.45711079982089,0.498665075583525,0.540219351346161,
0.581773627108796,0.623330197276748,0.664886767444701),.UNSPECIFIED.);
#4491=B_SPLINE_CURVE_WITH_KNOTS('',3,(#59193,#59194,#59195,#59196,#59197,
#59198,#59199,#59200,#59201,#59202,#59203,#59204,#59205,#59206,#59207,#59208,
#59209,#59210),.UNSPECIFIED.,.F.,.F.,(4,2,2,2,2,2,2,2,4),(0.165944509231404,
0.207430432450317,0.24891635566923,0.290402687066019,0.331889018462808,
0.373375349859597,0.414861681256386,0.456347604475299,0.497833527694212),
 .UNSPECIFIED.);
#4492=B_SPLINE_CURVE_WITH_KNOTS('',3,(#59211,#59212,#59213,#59214,#59215,
#59216,#59217,#59218,#59219,#59220,#59221,#59222,#59223,#59224,#59225,#59226,
#59227,#59228,#59229),.UNSPECIFIED.,.F.,.F.,(4,2,2,2,3,2,2,2,4),(0.497833527694212,
0.539319450913125,0.580805374132038,0.622291705528827,0.663778036925616,
0.705264368322405,0.746750699719194,0.788236622938107,0.82972254615702),
 .UNSPECIFIED.);
#4493=B_SPLINE_CURVE_WITH_KNOTS('',3,(#59233,#59234,#59235,#59236,#59237,
#59238,#59239,#59240,#59241,#59242),.UNSPECIFIED.,.F.,.F.,(4,2,2,2,4),(0.,
0.0415565701679523,0.0831131403359045,0.12466741609854,0.166221691861175),
 .UNSPECIFIED.);
#4494=B_SPLINE_CURVE_WITH_KNOTS('',3,(#59244,#59245,#59246,#59247,#59248,
#59249,#59250,#59251,#59252,#59253),.UNSPECIFIED.,.F.,.F.,(4,2,2,2,4),(0.498665075583525,
0.540219351346161,0.581773627108796,0.623330197276748,0.664886767444701),
 .UNSPECIFIED.);
#4495=B_SPLINE_CURVE_WITH_KNOTS('',3,(#59254,#59255,#59256,#59257,#59258,
#59259,#59260,#59261,#59262,#59263,#59264,#59265,#59266,#59267,#59268,#59269,
#59270,#59271),.UNSPECIFIED.,.F.,.F.,(4,2,2,2,2,2,2,2,4),(0.166221691861175,
0.20777596762381,0.249330243386446,0.290886813554398,0.33244338372235,0.373999953890303,
0.415556524058255,0.45711079982089,0.498665075583525),.UNSPECIFIED.);
#4496=B_SPLINE_CURVE_WITH_KNOTS('',3,(#59275,#59276,#59277,#59278,#59279,
#59280,#59281,#59282,#59283,#59284,#59285,#59286,#59287,#59288,#59289,#59290,
#59291,#59292),.UNSPECIFIED.,.F.,.F.,(4,2,2,2,2,2,2,2,4),(0.165944509231404,
0.207430432450317,0.24891635566923,0.290402687066019,0.331889018462808,
0.373375349859597,0.414861681256386,0.456347604475299,0.497833527694212),
 .UNSPECIFIED.);
#4497=B_SPLINE_CURVE_WITH_KNOTS('',3,(#59293,#59294,#59295,#59296,#59297,
#59298,#59299,#59300,#59301,#59302,#59303,#59304,#59305,#59306,#59307,#59308,
#59309,#59310,#59311),.UNSPECIFIED.,.F.,.F.,(4,2,2,2,3,2,2,2,4),(0.497833527694212,
0.539319450913125,0.580805374132038,0.622291705528827,0.663778036925616,
0.705264368322405,0.746750699719194,0.788236622938107,0.82972254615702),
 .UNSPECIFIED.);
#4498=B_SPLINE_CURVE_WITH_KNOTS('',3,(#59315,#59316,#59317,#59318,#59319,
#59320,#59321,#59322,#59323,#59324),.UNSPECIFIED.,.F.,.F.,(4,2,2,2,4),(0.,
0.0415565701679523,0.0831131403359046,0.12466741609854,0.166221691861175),
 .UNSPECIFIED.);
#4499=B_SPLINE_CURVE_WITH_KNOTS('',3,(#59325,#59326,#59327,#59328,#59329,
#59330,#59331,#59332,#59333,#59334,#59335,#59336,#59337,#59338,#59339,#59340,
#59341,#59342,#59343,#59344,#59345,#59346,#59347,#59348,#59349,#59350),
 .UNSPECIFIED.,.F.,.F.,(4,2,2,2,2,2,2,2,2,2,2,2,4),(0.166221691861175,0.20777596762381,
0.249330243386446,0.290886813554398,0.33244338372235,0.373999953890303,
0.415556524058255,0.45711079982089,0.498665075583525,0.540219351346161,
0.581773627108796,0.623330197276748,0.664886767444701),.UNSPECIFIED.);
#4500=LINE('',#23615,#5912);
#4501=LINE('',#23639,#5913);
#4502=LINE('',#23687,#5914);
#4503=LINE('',#23735,#5915);
#4504=LINE('',#23789,#5916);
#4505=LINE('',#23837,#5917);
#4506=LINE('',#23885,#5918);
#4507=LINE('',#23939,#5919);
#4508=LINE('',#23987,#5920);
#4509=LINE('',#24035,#5921);
#4510=LINE('',#24089,#5922);
#4511=LINE('',#24137,#5923);
#4512=LINE('',#24185,#5924);
#4513=LINE('',#24239,#5925);
#4514=LINE('',#24287,#5926);
#4515=LINE('',#24335,#5927);
#4516=LINE('',#26593,#5928);
#4517=LINE('',#26611,#5929);
#4518=LINE('',#26636,#5930);
#4519=LINE('',#26661,#5931);
#4520=LINE('',#26685,#5932);
#4521=LINE('',#26710,#5933);
#4522=LINE('',#26735,#5934);
#4523=LINE('',#26759,#5935);
#4524=LINE('',#26784,#5936);
#4525=LINE('',#26809,#5937);
#4526=LINE('',#26833,#5938);
#4527=LINE('',#26858,#5939);
#4528=LINE('',#26883,#5940);
#4529=LINE('',#26907,#5941);
#4530=LINE('',#26932,#5942);
#4531=LINE('',#26957,#5943);
#4532=LINE('',#26982,#5944);
#4533=LINE('',#26988,#5945);
#4534=LINE('',#26996,#5946);
#4535=LINE('',#26998,#5947);
#4536=LINE('',#27000,#5948);
#4537=LINE('',#27002,#5949);
#4538=LINE('',#27003,#5950);
#4539=LINE('',#27006,#5951);
#4540=LINE('',#27008,#5952);
#4541=LINE('',#27009,#5953);
#4542=LINE('',#27012,#5954);
#4543=LINE('',#27014,#5955);
#4544=LINE('',#27015,#5956);
#4545=LINE('',#27018,#5957);
#4546=LINE('',#27020,#5958);
#4547=LINE('',#27021,#5959);
#4548=LINE('',#27025,#5960);
#4549=LINE('',#27027,#5961);
#4550=LINE('',#27029,#5962);
#4551=LINE('',#27031,#5963);
#4552=LINE('',#27032,#5964);
#4553=LINE('',#27035,#5965);
#4554=LINE('',#27037,#5966);
#4555=LINE('',#27038,#5967);
#4556=LINE('',#27041,#5968);
#4557=LINE('',#27043,#5969);
#4558=LINE('',#27044,#5970);
#4559=LINE('',#27046,#5971);
#4560=LINE('',#27047,#5972);
#4561=LINE('',#27051,#5973);
#4562=LINE('',#27053,#5974);
#4563=LINE('',#27055,#5975);
#4564=LINE('',#27057,#5976);
#4565=LINE('',#27058,#5977);
#4566=LINE('',#27061,#5978);
#4567=LINE('',#27063,#5979);
#4568=LINE('',#27064,#5980);
#4569=LINE('',#27067,#5981);
#4570=LINE('',#27069,#5982);
#4571=LINE('',#27070,#5983);
#4572=LINE('',#27072,#5984);
#4573=LINE('',#27073,#5985);
#4574=LINE('',#27077,#5986);
#4575=LINE('',#27079,#5987);
#4576=LINE('',#27081,#5988);
#4577=LINE('',#27083,#5989);
#4578=LINE('',#27084,#5990);
#4579=LINE('',#27087,#5991);
#4580=LINE('',#27089,#5992);
#4581=LINE('',#27090,#5993);
#4582=LINE('',#27093,#5994);
#4583=LINE('',#27095,#5995);
#4584=LINE('',#27096,#5996);
#4585=LINE('',#27098,#5997);
#4586=LINE('',#27099,#5998);
#4587=LINE('',#27103,#5999);
#4588=LINE('',#27105,#6000);
#4589=LINE('',#27107,#6001);
#4590=LINE('',#27109,#6002);
#4591=LINE('',#27110,#6003);
#4592=LINE('',#27113,#6004);
#4593=LINE('',#27115,#6005);
#4594=LINE('',#27116,#6006);
#4595=LINE('',#27119,#6007);
#4596=LINE('',#27121,#6008);
#4597=LINE('',#27122,#6009);
#4598=LINE('',#27124,#6010);
#4599=LINE('',#27125,#6011);
#4600=LINE('',#27129,#6012);
#4601=LINE('',#27131,#6013);
#4602=LINE('',#27133,#6014);
#4603=LINE('',#27135,#6015);
#4604=LINE('',#27136,#6016);
#4605=LINE('',#27138,#6017);
#4606=LINE('',#27140,#6018);
#4607=LINE('',#27141,#6019);
#4608=LINE('',#27144,#6020);
#4609=LINE('',#27145,#6021);
#4610=LINE('',#27148,#6022);
#4611=LINE('',#27150,#6023);
#4612=LINE('',#27151,#6024);
#4613=LINE('',#27155,#6025);
#4614=LINE('',#27157,#6026);
#4615=LINE('',#27159,#6027);
#4616=LINE('',#27161,#6028);
#4617=LINE('',#27162,#6029);
#4618=LINE('',#27164,#6030);
#4619=LINE('',#27166,#6031);
#4620=LINE('',#27167,#6032);
#4621=LINE('',#27170,#6033);
#4622=LINE('',#27171,#6034);
#4623=LINE('',#27175,#6035);
#4624=LINE('',#27177,#6036);
#4625=LINE('',#27179,#6037);
#4626=LINE('',#27181,#6038);
#4627=LINE('',#27182,#6039);
#4628=LINE('',#27185,#6040);
#4629=LINE('',#27187,#6041);
#4630=LINE('',#27188,#6042);
#4631=LINE('',#27191,#6043);
#4632=LINE('',#27193,#6044);
#4633=LINE('',#27194,#6045);
#4634=LINE('',#27197,#6046);
#4635=LINE('',#27199,#6047);
#4636=LINE('',#27200,#6048);
#4637=LINE('',#27204,#6049);
#4638=LINE('',#27206,#6050);
#4639=LINE('',#27208,#6051);
#4640=LINE('',#27210,#6052);
#4641=LINE('',#27211,#6053);
#4642=LINE('',#27213,#6054);
#4643=LINE('',#27215,#6055);
#4644=LINE('',#27216,#6056);
#4645=LINE('',#27219,#6057);
#4646=LINE('',#27220,#6058);
#4647=LINE('',#27223,#6059);
#4648=LINE('',#27225,#6060);
#4649=LINE('',#27226,#6061);
#4650=LINE('',#27230,#6062);
#4651=LINE('',#27232,#6063);
#4652=LINE('',#27234,#6064);
#4653=LINE('',#27236,#6065);
#4654=LINE('',#27237,#6066);
#4655=LINE('',#27239,#6067);
#4656=LINE('',#27241,#6068);
#4657=LINE('',#27242,#6069);
#4658=LINE('',#27245,#6070);
#4659=LINE('',#27246,#6071);
#4660=LINE('',#27249,#6072);
#4661=LINE('',#27251,#6073);
#4662=LINE('',#27252,#6074);
#4663=LINE('',#27256,#6075);
#4664=LINE('',#27258,#6076);
#4665=LINE('',#27260,#6077);
#4666=LINE('',#27262,#6078);
#4667=LINE('',#27263,#6079);
#4668=LINE('',#27265,#6080);
#4669=LINE('',#27267,#6081);
#4670=LINE('',#27268,#6082);
#4671=LINE('',#27271,#6083);
#4672=LINE('',#27272,#6084);
#4673=LINE('',#27275,#6085);
#4674=LINE('',#27277,#6086);
#4675=LINE('',#27278,#6087);
#4676=LINE('',#27282,#6088);
#4677=LINE('',#27284,#6089);
#4678=LINE('',#27286,#6090);
#4679=LINE('',#27288,#6091);
#4680=LINE('',#27289,#6092);
#4681=LINE('',#27291,#6093);
#4682=LINE('',#27293,#6094);
#4683=LINE('',#27294,#6095);
#4684=LINE('',#27297,#6096);
#4685=LINE('',#27298,#6097);
#4686=LINE('',#27300,#6098);
#4687=LINE('',#27301,#6099);
#4688=LINE('',#32833,#6100);
#4689=LINE('',#32841,#6101);
#4690=LINE('',#32846,#6102);
#4691=LINE('',#32853,#6103);
#4692=LINE('',#32862,#6104);
#4693=LINE('',#32871,#6105);
#4694=LINE('',#32914,#6106);
#4695=LINE('',#32921,#6107);
#4696=LINE('',#32945,#6108);
#4697=LINE('',#32949,#6109);
#4698=LINE('',#32974,#6110);
#4699=LINE('',#32981,#6111);
#4700=LINE('',#33005,#6112);
#4701=LINE('',#33009,#6113);
#4702=LINE('',#33034,#6114);
#4703=LINE('',#33041,#6115);
#4704=LINE('',#33065,#6116);
#4705=LINE('',#33069,#6117);
#4706=LINE('',#33094,#6118);
#4707=LINE('',#33101,#6119);
#4708=LINE('',#33125,#6120);
#4709=LINE('',#33129,#6121);
#4710=LINE('',#33154,#6122);
#4711=LINE('',#33161,#6123);
#4712=LINE('',#33223,#6124);
#4713=LINE('',#33228,#6125);
#4714=LINE('',#33245,#6126);
#4715=LINE('',#33265,#6127);
#4716=LINE('',#33280,#6128);
#4717=LINE('',#33287,#6129);
#4718=LINE('',#33319,#6130);
#4719=LINE('',#33324,#6131);
#4720=LINE('',#33336,#6132);
#4721=LINE('',#33343,#6133);
#4722=LINE('',#33375,#6134);
#4723=LINE('',#33380,#6135);
#4724=LINE('',#33392,#6136);
#4725=LINE('',#33399,#6137);
#4726=LINE('',#33431,#6138);
#4727=LINE('',#33436,#6139);
#4728=LINE('',#33448,#6140);
#4729=LINE('',#33455,#6141);
#4730=LINE('',#33487,#6142);
#4731=LINE('',#33492,#6143);
#4732=LINE('',#33504,#6144);
#4733=LINE('',#33511,#6145);
#4734=LINE('',#33543,#6146);
#4735=LINE('',#33548,#6147);
#4736=LINE('',#33553,#6148);
#4737=LINE('',#33583,#6149);
#4738=LINE('',#33590,#6150);
#4739=LINE('',#33602,#6151);
#4740=LINE('',#35493,#6152);
#4741=LINE('',#35502,#6153);
#4742=LINE('',#35504,#6154);
#4743=LINE('',#41624,#6155);
#4744=LINE('',#41625,#6156);
#4745=LINE('',#41627,#6157);
#4746=LINE('',#41629,#6158);
#4747=LINE('',#41631,#6159);
#4748=LINE('',#41633,#6160);
#4749=LINE('',#41635,#6161);
#4750=LINE('',#41637,#6162);
#4751=LINE('',#41640,#6163);
#4752=LINE('',#41642,#6164);
#4753=LINE('',#41644,#6165);
#4754=LINE('',#41646,#6166);
#4755=LINE('',#41648,#6167);
#4756=LINE('',#41650,#6168);
#4757=LINE('',#41655,#6169);
#4758=LINE('',#41657,#6170);
#4759=LINE('',#41659,#6171);
#4760=LINE('',#41663,#6172);
#4761=LINE('',#41670,#6173);
#4762=LINE('',#41674,#6174);
#4763=LINE('',#41678,#6175);
#4764=LINE('',#41682,#6176);
#4765=LINE('',#41689,#6177);
#4766=LINE('',#41693,#6178);
#4767=LINE('',#41697,#6179);
#4768=LINE('',#41701,#6180);
#4769=LINE('',#41705,#6181);
#4770=LINE('',#41707,#6182);
#4771=LINE('',#41713,#6183);
#4772=LINE('',#41832,#6184);
#4773=LINE('',#41839,#6185);
#4774=LINE('',#41848,#6186);
#4775=LINE('',#41856,#6187);
#4776=LINE('',#42588,#6188);
#4777=LINE('',#43631,#6189);
#4778=LINE('',#43723,#6190);
#4779=LINE('',#43724,#6191);
#4780=LINE('',#43732,#6192);
#4781=LINE('',#43737,#6193);
#4782=LINE('',#43741,#6194);
#4783=LINE('',#43747,#6195);
#4784=LINE('',#43751,#6196);
#4785=LINE('',#43755,#6197);
#4786=LINE('',#43762,#6198);
#4787=LINE('',#43764,#6199);
#4788=LINE('',#43766,#6200);
#4789=LINE('',#43767,#6201);
#4790=LINE('',#43770,#6202);
#4791=LINE('',#43772,#6203);
#4792=LINE('',#43773,#6204);
#4793=LINE('',#43778,#6205);
#4794=LINE('',#43780,#6206);
#4795=LINE('',#43781,#6207);
#4796=LINE('',#43784,#6208);
#4797=LINE('',#43786,#6209);
#4798=LINE('',#43796,#6210);
#4799=LINE('',#43798,#6211);
#4800=LINE('',#43800,#6212);
#4801=LINE('',#43802,#6213);
#4802=LINE('',#43804,#6214);
#4803=LINE('',#43806,#6215);
#4804=LINE('',#43808,#6216);
#4805=LINE('',#43810,#6217);
#4806=LINE('',#43812,#6218);
#4807=LINE('',#43814,#6219);
#4808=LINE('',#43816,#6220);
#4809=LINE('',#43818,#6221);
#4810=LINE('',#43820,#6222);
#4811=LINE('',#43821,#6223);
#4812=LINE('',#43824,#6224);
#4813=LINE('',#43826,#6225);
#4814=LINE('',#43828,#6226);
#4815=LINE('',#43830,#6227);
#4816=LINE('',#43832,#6228);
#4817=LINE('',#43834,#6229);
#4818=LINE('',#43836,#6230);
#4819=LINE('',#43838,#6231);
#4820=LINE('',#43840,#6232);
#4821=LINE('',#43842,#6233);
#4822=LINE('',#43844,#6234);
#4823=LINE('',#43846,#6235);
#4824=LINE('',#43848,#6236);
#4825=LINE('',#43849,#6237);
#4826=LINE('',#43852,#6238);
#4827=LINE('',#43854,#6239);
#4828=LINE('',#43856,#6240);
#4829=LINE('',#43858,#6241);
#4830=LINE('',#43860,#6242);
#4831=LINE('',#43862,#6243);
#4832=LINE('',#43864,#6244);
#4833=LINE('',#43866,#6245);
#4834=LINE('',#43868,#6246);
#4835=LINE('',#43870,#6247);
#4836=LINE('',#43872,#6248);
#4837=LINE('',#43874,#6249);
#4838=LINE('',#43876,#6250);
#4839=LINE('',#43877,#6251);
#4840=LINE('',#43880,#6252);
#4841=LINE('',#43882,#6253);
#4842=LINE('',#43884,#6254);
#4843=LINE('',#43886,#6255);
#4844=LINE('',#43888,#6256);
#4845=LINE('',#43890,#6257);
#4846=LINE('',#43892,#6258);
#4847=LINE('',#43894,#6259);
#4848=LINE('',#43896,#6260);
#4849=LINE('',#43898,#6261);
#4850=LINE('',#43900,#6262);
#4851=LINE('',#43902,#6263);
#4852=LINE('',#43904,#6264);
#4853=LINE('',#43905,#6265);
#4854=LINE('',#43908,#6266);
#4855=LINE('',#43910,#6267);
#4856=LINE('',#43912,#6268);
#4857=LINE('',#43914,#6269);
#4858=LINE('',#43916,#6270);
#4859=LINE('',#43918,#6271);
#4860=LINE('',#43920,#6272);
#4861=LINE('',#43922,#6273);
#4862=LINE('',#43924,#6274);
#4863=LINE('',#43926,#6275);
#4864=LINE('',#43928,#6276);
#4865=LINE('',#43930,#6277);
#4866=LINE('',#43932,#6278);
#4867=LINE('',#43933,#6279);
#4868=LINE('',#43936,#6280);
#4869=LINE('',#43938,#6281);
#4870=LINE('',#43940,#6282);
#4871=LINE('',#43942,#6283);
#4872=LINE('',#43944,#6284);
#4873=LINE('',#43946,#6285);
#4874=LINE('',#43948,#6286);
#4875=LINE('',#43950,#6287);
#4876=LINE('',#43952,#6288);
#4877=LINE('',#43954,#6289);
#4878=LINE('',#43956,#6290);
#4879=LINE('',#43958,#6291);
#4880=LINE('',#43960,#6292);
#4881=LINE('',#43961,#6293);
#4882=LINE('',#43986,#6294);
#4883=LINE('',#43988,#6295);
#4884=LINE('',#44011,#6296);
#4885=LINE('',#44012,#6297);
#4886=LINE('',#44014,#6298);
#4887=LINE('',#44016,#6299);
#4888=LINE('',#44025,#6300);
#4889=LINE('',#44027,#6301);
#4890=LINE('',#44029,#6302);
#4891=LINE('',#44031,#6303);
#4892=LINE('',#44033,#6304);
#4893=LINE('',#44035,#6305);
#4894=LINE('',#44037,#6306);
#4895=LINE('',#44039,#6307);
#4896=LINE('',#44041,#6308);
#4897=LINE('',#44043,#6309);
#4898=LINE('',#44045,#6310);
#4899=LINE('',#44047,#6311);
#4900=LINE('',#44049,#6312);
#4901=LINE('',#44050,#6313);
#4902=LINE('',#44053,#6314);
#4903=LINE('',#44055,#6315);
#4904=LINE('',#44057,#6316);
#4905=LINE('',#44059,#6317);
#4906=LINE('',#44061,#6318);
#4907=LINE('',#44063,#6319);
#4908=LINE('',#44065,#6320);
#4909=LINE('',#44067,#6321);
#4910=LINE('',#44069,#6322);
#4911=LINE('',#44071,#6323);
#4912=LINE('',#44073,#6324);
#4913=LINE('',#44075,#6325);
#4914=LINE('',#44077,#6326);
#4915=LINE('',#44078,#6327);
#4916=LINE('',#44081,#6328);
#4917=LINE('',#44083,#6329);
#4918=LINE('',#44085,#6330);
#4919=LINE('',#44087,#6331);
#4920=LINE('',#44089,#6332);
#4921=LINE('',#44091,#6333);
#4922=LINE('',#44093,#6334);
#4923=LINE('',#44095,#6335);
#4924=LINE('',#44097,#6336);
#4925=LINE('',#44099,#6337);
#4926=LINE('',#44101,#6338);
#4927=LINE('',#44103,#6339);
#4928=LINE('',#44105,#6340);
#4929=LINE('',#44106,#6341);
#4930=LINE('',#44109,#6342);
#4931=LINE('',#44111,#6343);
#4932=LINE('',#44113,#6344);
#4933=LINE('',#44115,#6345);
#4934=LINE('',#44117,#6346);
#4935=LINE('',#44119,#6347);
#4936=LINE('',#44121,#6348);
#4937=LINE('',#44123,#6349);
#4938=LINE('',#44125,#6350);
#4939=LINE('',#44127,#6351);
#4940=LINE('',#44129,#6352);
#4941=LINE('',#44131,#6353);
#4942=LINE('',#44133,#6354);
#4943=LINE('',#44134,#6355);
#4944=LINE('',#44137,#6356);
#4945=LINE('',#44139,#6357);
#4946=LINE('',#44141,#6358);
#4947=LINE('',#44143,#6359);
#4948=LINE('',#44145,#6360);
#4949=LINE('',#44147,#6361);
#4950=LINE('',#44149,#6362);
#4951=LINE('',#44151,#6363);
#4952=LINE('',#44153,#6364);
#4953=LINE('',#44155,#6365);
#4954=LINE('',#44157,#6366);
#4955=LINE('',#44159,#6367);
#4956=LINE('',#44161,#6368);
#4957=LINE('',#44162,#6369);
#4958=LINE('',#44165,#6370);
#4959=LINE('',#44167,#6371);
#4960=LINE('',#44169,#6372);
#4961=LINE('',#44171,#6373);
#4962=LINE('',#44173,#6374);
#4963=LINE('',#44175,#6375);
#4964=LINE('',#44177,#6376);
#4965=LINE('',#44179,#6377);
#4966=LINE('',#44181,#6378);
#4967=LINE('',#44183,#6379);
#4968=LINE('',#44185,#6380);
#4969=LINE('',#44187,#6381);
#4970=LINE('',#44189,#6382);
#4971=LINE('',#44190,#6383);
#4972=LINE('',#44196,#6384);
#4973=LINE('',#44200,#6385);
#4974=LINE('',#44203,#6386);
#4975=LINE('',#44206,#6387);
#4976=LINE('',#44210,#6388);
#4977=LINE('',#44213,#6389);
#4978=LINE('',#44216,#6390);
#4979=LINE('',#44220,#6391);
#4980=LINE('',#44223,#6392);
#4981=LINE('',#44226,#6393);
#4982=LINE('',#44230,#6394);
#4983=LINE('',#44273,#6395);
#4984=LINE('',#44275,#6396);
#4985=LINE('',#44276,#6397);
#4986=LINE('',#44279,#6398);
#4987=LINE('',#44280,#6399);
#4988=LINE('',#44283,#6400);
#4989=LINE('',#44284,#6401);
#4990=LINE('',#44287,#6402);
#4991=LINE('',#44288,#6403);
#4992=LINE('',#44291,#6404);
#4993=LINE('',#44292,#6405);
#4994=LINE('',#44295,#6406);
#4995=LINE('',#44296,#6407);
#4996=LINE('',#44299,#6408);
#4997=LINE('',#44300,#6409);
#4998=LINE('',#44303,#6410);
#4999=LINE('',#44304,#6411);
#5000=LINE('',#44307,#6412);
#5001=LINE('',#44308,#6413);
#5002=LINE('',#44311,#6414);
#5003=LINE('',#44312,#6415);
#5004=LINE('',#44315,#6416);
#5005=LINE('',#44316,#6417);
#5006=LINE('',#44319,#6418);
#5007=LINE('',#44320,#6419);
#5008=LINE('',#44323,#6420);
#5009=LINE('',#44324,#6421);
#5010=LINE('',#44326,#6422);
#5011=LINE('',#44330,#6423);
#5012=LINE('',#44332,#6424);
#5013=LINE('',#44333,#6425);
#5014=LINE('',#44336,#6426);
#5015=LINE('',#44337,#6427);
#5016=LINE('',#44340,#6428);
#5017=LINE('',#44341,#6429);
#5018=LINE('',#44344,#6430);
#5019=LINE('',#44345,#6431);
#5020=LINE('',#44348,#6432);
#5021=LINE('',#44349,#6433);
#5022=LINE('',#44352,#6434);
#5023=LINE('',#44353,#6435);
#5024=LINE('',#44356,#6436);
#5025=LINE('',#44357,#6437);
#5026=LINE('',#44360,#6438);
#5027=LINE('',#44361,#6439);
#5028=LINE('',#44364,#6440);
#5029=LINE('',#44365,#6441);
#5030=LINE('',#44368,#6442);
#5031=LINE('',#44369,#6443);
#5032=LINE('',#44372,#6444);
#5033=LINE('',#44373,#6445);
#5034=LINE('',#44376,#6446);
#5035=LINE('',#44377,#6447);
#5036=LINE('',#44380,#6448);
#5037=LINE('',#44381,#6449);
#5038=LINE('',#44383,#6450);
#5039=LINE('',#44387,#6451);
#5040=LINE('',#44389,#6452);
#5041=LINE('',#44390,#6453);
#5042=LINE('',#44393,#6454);
#5043=LINE('',#44394,#6455);
#5044=LINE('',#44397,#6456);
#5045=LINE('',#44398,#6457);
#5046=LINE('',#44401,#6458);
#5047=LINE('',#44402,#6459);
#5048=LINE('',#44405,#6460);
#5049=LINE('',#44406,#6461);
#5050=LINE('',#44409,#6462);
#5051=LINE('',#44410,#6463);
#5052=LINE('',#44413,#6464);
#5053=LINE('',#44414,#6465);
#5054=LINE('',#44417,#6466);
#5055=LINE('',#44418,#6467);
#5056=LINE('',#44421,#6468);
#5057=LINE('',#44422,#6469);
#5058=LINE('',#44425,#6470);
#5059=LINE('',#44426,#6471);
#5060=LINE('',#44429,#6472);
#5061=LINE('',#44430,#6473);
#5062=LINE('',#44433,#6474);
#5063=LINE('',#44434,#6475);
#5064=LINE('',#44437,#6476);
#5065=LINE('',#44438,#6477);
#5066=LINE('',#44440,#6478);
#5067=LINE('',#44444,#6479);
#5068=LINE('',#44446,#6480);
#5069=LINE('',#44447,#6481);
#5070=LINE('',#44450,#6482);
#5071=LINE('',#44451,#6483);
#5072=LINE('',#44454,#6484);
#5073=LINE('',#44455,#6485);
#5074=LINE('',#44458,#6486);
#5075=LINE('',#44459,#6487);
#5076=LINE('',#44462,#6488);
#5077=LINE('',#44463,#6489);
#5078=LINE('',#44466,#6490);
#5079=LINE('',#44467,#6491);
#5080=LINE('',#44470,#6492);
#5081=LINE('',#44471,#6493);
#5082=LINE('',#44474,#6494);
#5083=LINE('',#44475,#6495);
#5084=LINE('',#44478,#6496);
#5085=LINE('',#44479,#6497);
#5086=LINE('',#44482,#6498);
#5087=LINE('',#44483,#6499);
#5088=LINE('',#44486,#6500);
#5089=LINE('',#44487,#6501);
#5090=LINE('',#44490,#6502);
#5091=LINE('',#44491,#6503);
#5092=LINE('',#44494,#6504);
#5093=LINE('',#44495,#6505);
#5094=LINE('',#44497,#6506);
#5095=LINE('',#44501,#6507);
#5096=LINE('',#44503,#6508);
#5097=LINE('',#44504,#6509);
#5098=LINE('',#44507,#6510);
#5099=LINE('',#44508,#6511);
#5100=LINE('',#44511,#6512);
#5101=LINE('',#44512,#6513);
#5102=LINE('',#44515,#6514);
#5103=LINE('',#44516,#6515);
#5104=LINE('',#44519,#6516);
#5105=LINE('',#44520,#6517);
#5106=LINE('',#44523,#6518);
#5107=LINE('',#44524,#6519);
#5108=LINE('',#44527,#6520);
#5109=LINE('',#44528,#6521);
#5110=LINE('',#44531,#6522);
#5111=LINE('',#44532,#6523);
#5112=LINE('',#44535,#6524);
#5113=LINE('',#44536,#6525);
#5114=LINE('',#44539,#6526);
#5115=LINE('',#44540,#6527);
#5116=LINE('',#44543,#6528);
#5117=LINE('',#44544,#6529);
#5118=LINE('',#44547,#6530);
#5119=LINE('',#44548,#6531);
#5120=LINE('',#44551,#6532);
#5121=LINE('',#44552,#6533);
#5122=LINE('',#44554,#6534);
#5123=LINE('',#44558,#6535);
#5124=LINE('',#44560,#6536);
#5125=LINE('',#44561,#6537);
#5126=LINE('',#44564,#6538);
#5127=LINE('',#44565,#6539);
#5128=LINE('',#44568,#6540);
#5129=LINE('',#44569,#6541);
#5130=LINE('',#44572,#6542);
#5131=LINE('',#44573,#6543);
#5132=LINE('',#44576,#6544);
#5133=LINE('',#44577,#6545);
#5134=LINE('',#44580,#6546);
#5135=LINE('',#44581,#6547);
#5136=LINE('',#44584,#6548);
#5137=LINE('',#44585,#6549);
#5138=LINE('',#44588,#6550);
#5139=LINE('',#44589,#6551);
#5140=LINE('',#44592,#6552);
#5141=LINE('',#44593,#6553);
#5142=LINE('',#44596,#6554);
#5143=LINE('',#44597,#6555);
#5144=LINE('',#44600,#6556);
#5145=LINE('',#44601,#6557);
#5146=LINE('',#44604,#6558);
#5147=LINE('',#44605,#6559);
#5148=LINE('',#44608,#6560);
#5149=LINE('',#44609,#6561);
#5150=LINE('',#44611,#6562);
#5151=LINE('',#44615,#6563);
#5152=LINE('',#44617,#6564);
#5153=LINE('',#44618,#6565);
#5154=LINE('',#44621,#6566);
#5155=LINE('',#44622,#6567);
#5156=LINE('',#44625,#6568);
#5157=LINE('',#44626,#6569);
#5158=LINE('',#44629,#6570);
#5159=LINE('',#44630,#6571);
#5160=LINE('',#44633,#6572);
#5161=LINE('',#44634,#6573);
#5162=LINE('',#44637,#6574);
#5163=LINE('',#44638,#6575);
#5164=LINE('',#44641,#6576);
#5165=LINE('',#44642,#6577);
#5166=LINE('',#44645,#6578);
#5167=LINE('',#44646,#6579);
#5168=LINE('',#44649,#6580);
#5169=LINE('',#44650,#6581);
#5170=LINE('',#44653,#6582);
#5171=LINE('',#44654,#6583);
#5172=LINE('',#44657,#6584);
#5173=LINE('',#44658,#6585);
#5174=LINE('',#44661,#6586);
#5175=LINE('',#44662,#6587);
#5176=LINE('',#44665,#6588);
#5177=LINE('',#44666,#6589);
#5178=LINE('',#44668,#6590);
#5179=LINE('',#44672,#6591);
#5180=LINE('',#44674,#6592);
#5181=LINE('',#44675,#6593);
#5182=LINE('',#44678,#6594);
#5183=LINE('',#44679,#6595);
#5184=LINE('',#44682,#6596);
#5185=LINE('',#44683,#6597);
#5186=LINE('',#44686,#6598);
#5187=LINE('',#44687,#6599);
#5188=LINE('',#44690,#6600);
#5189=LINE('',#44691,#6601);
#5190=LINE('',#44694,#6602);
#5191=LINE('',#44695,#6603);
#5192=LINE('',#44698,#6604);
#5193=LINE('',#44699,#6605);
#5194=LINE('',#44702,#6606);
#5195=LINE('',#44703,#6607);
#5196=LINE('',#44706,#6608);
#5197=LINE('',#44707,#6609);
#5198=LINE('',#44710,#6610);
#5199=LINE('',#44711,#6611);
#5200=LINE('',#44714,#6612);
#5201=LINE('',#44715,#6613);
#5202=LINE('',#44718,#6614);
#5203=LINE('',#44719,#6615);
#5204=LINE('',#44722,#6616);
#5205=LINE('',#44723,#6617);
#5206=LINE('',#44725,#6618);
#5207=LINE('',#44729,#6619);
#5208=LINE('',#44731,#6620);
#5209=LINE('',#44732,#6621);
#5210=LINE('',#44735,#6622);
#5211=LINE('',#44736,#6623);
#5212=LINE('',#44739,#6624);
#5213=LINE('',#44740,#6625);
#5214=LINE('',#44743,#6626);
#5215=LINE('',#44744,#6627);
#5216=LINE('',#44747,#6628);
#5217=LINE('',#44748,#6629);
#5218=LINE('',#44751,#6630);
#5219=LINE('',#44752,#6631);
#5220=LINE('',#44755,#6632);
#5221=LINE('',#44756,#6633);
#5222=LINE('',#44759,#6634);
#5223=LINE('',#44760,#6635);
#5224=LINE('',#44763,#6636);
#5225=LINE('',#44764,#6637);
#5226=LINE('',#44767,#6638);
#5227=LINE('',#44768,#6639);
#5228=LINE('',#44771,#6640);
#5229=LINE('',#44772,#6641);
#5230=LINE('',#44775,#6642);
#5231=LINE('',#44776,#6643);
#5232=LINE('',#44779,#6644);
#5233=LINE('',#44780,#6645);
#5234=LINE('',#44782,#6646);
#5235=LINE('',#44786,#6647);
#5236=LINE('',#44788,#6648);
#5237=LINE('',#44789,#6649);
#5238=LINE('',#44792,#6650);
#5239=LINE('',#44793,#6651);
#5240=LINE('',#44796,#6652);
#5241=LINE('',#44797,#6653);
#5242=LINE('',#44800,#6654);
#5243=LINE('',#44801,#6655);
#5244=LINE('',#44804,#6656);
#5245=LINE('',#44805,#6657);
#5246=LINE('',#44808,#6658);
#5247=LINE('',#44809,#6659);
#5248=LINE('',#44812,#6660);
#5249=LINE('',#44813,#6661);
#5250=LINE('',#44816,#6662);
#5251=LINE('',#44817,#6663);
#5252=LINE('',#44820,#6664);
#5253=LINE('',#44821,#6665);
#5254=LINE('',#44824,#6666);
#5255=LINE('',#44825,#6667);
#5256=LINE('',#44828,#6668);
#5257=LINE('',#44829,#6669);
#5258=LINE('',#44832,#6670);
#5259=LINE('',#44833,#6671);
#5260=LINE('',#44836,#6672);
#5261=LINE('',#44837,#6673);
#5262=LINE('',#44839,#6674);
#5263=LINE('',#44843,#6675);
#5264=LINE('',#44845,#6676);
#5265=LINE('',#44846,#6677);
#5266=LINE('',#44849,#6678);
#5267=LINE('',#44850,#6679);
#5268=LINE('',#44853,#6680);
#5269=LINE('',#44854,#6681);
#5270=LINE('',#44857,#6682);
#5271=LINE('',#44858,#6683);
#5272=LINE('',#44861,#6684);
#5273=LINE('',#44862,#6685);
#5274=LINE('',#44865,#6686);
#5275=LINE('',#44866,#6687);
#5276=LINE('',#44869,#6688);
#5277=LINE('',#44870,#6689);
#5278=LINE('',#44873,#6690);
#5279=LINE('',#44874,#6691);
#5280=LINE('',#44877,#6692);
#5281=LINE('',#44878,#6693);
#5282=LINE('',#44881,#6694);
#5283=LINE('',#44882,#6695);
#5284=LINE('',#44885,#6696);
#5285=LINE('',#44886,#6697);
#5286=LINE('',#44889,#6698);
#5287=LINE('',#44890,#6699);
#5288=LINE('',#44893,#6700);
#5289=LINE('',#44894,#6701);
#5290=LINE('',#44896,#6702);
#5291=LINE('',#44900,#6703);
#5292=LINE('',#44902,#6704);
#5293=LINE('',#44903,#6705);
#5294=LINE('',#44906,#6706);
#5295=LINE('',#44907,#6707);
#5296=LINE('',#44910,#6708);
#5297=LINE('',#44911,#6709);
#5298=LINE('',#44914,#6710);
#5299=LINE('',#44915,#6711);
#5300=LINE('',#44918,#6712);
#5301=LINE('',#44919,#6713);
#5302=LINE('',#44922,#6714);
#5303=LINE('',#44923,#6715);
#5304=LINE('',#44926,#6716);
#5305=LINE('',#44927,#6717);
#5306=LINE('',#44930,#6718);
#5307=LINE('',#44931,#6719);
#5308=LINE('',#44934,#6720);
#5309=LINE('',#44935,#6721);
#5310=LINE('',#44938,#6722);
#5311=LINE('',#44939,#6723);
#5312=LINE('',#44942,#6724);
#5313=LINE('',#44943,#6725);
#5314=LINE('',#44946,#6726);
#5315=LINE('',#44947,#6727);
#5316=LINE('',#44950,#6728);
#5317=LINE('',#44951,#6729);
#5318=LINE('',#44953,#6730);
#5319=LINE('',#44956,#6731);
#5320=LINE('',#44957,#6732);
#5321=LINE('',#44964,#6733);
#5322=LINE('',#44971,#6734);
#5323=LINE('',#44978,#6735);
#5324=LINE('',#44985,#6736);
#5325=LINE('',#44992,#6737);
#5326=LINE('',#44999,#6738);
#5327=LINE('',#45006,#6739);
#5328=LINE('',#45017,#6740);
#5329=LINE('',#45022,#6741);
#5330=LINE('',#45027,#6742);
#5331=LINE('',#45034,#6743);
#5332=LINE('',#45038,#6744);
#5333=LINE('',#45042,#6745);
#5334=LINE('',#45049,#6746);
#5335=LINE('',#45051,#6747);
#5336=LINE('',#45055,#6748);
#5337=LINE('',#45061,#6749);
#5338=LINE('',#45065,#6750);
#5339=LINE('',#45069,#6751);
#5340=LINE('',#45171,#6752);
#5341=LINE('',#45178,#6753);
#5342=LINE('',#45187,#6754);
#5343=LINE('',#45195,#6755);
#5344=LINE('',#45927,#6756);
#5345=LINE('',#46934,#6757);
#5346=LINE('',#47061,#6758);
#5347=LINE('',#47062,#6759);
#5348=LINE('',#47684,#6760);
#5349=LINE('',#48050,#6761);
#5350=LINE('',#48059,#6762);
#5351=LINE('',#48065,#6763);
#5352=LINE('',#57370,#6764);
#5353=LINE('',#57375,#6765);
#5354=LINE('',#57379,#6766);
#5355=LINE('',#57381,#6767);
#5356=LINE('',#57394,#6768);
#5357=LINE('',#57396,#6769);
#5358=LINE('',#57398,#6770);
#5359=LINE('',#57412,#6771);
#5360=LINE('',#57413,#6772);
#5361=LINE('',#57460,#6773);
#5362=LINE('',#57462,#6774);
#5363=LINE('',#57464,#6775);
#5364=LINE('',#57478,#6776);
#5365=LINE('',#57479,#6777);
#5366=LINE('',#57526,#6778);
#5367=LINE('',#57528,#6779);
#5368=LINE('',#57530,#6780);
#5369=LINE('',#57544,#6781);
#5370=LINE('',#57545,#6782);
#5371=LINE('',#57588,#6783);
#5372=LINE('',#57590,#6784);
#5373=LINE('',#57591,#6785);
#5374=LINE('',#57609,#6786);
#5375=LINE('',#57610,#6787);
#5376=LINE('',#57659,#6788);
#5377=LINE('',#57661,#6789);
#5378=LINE('',#57662,#6790);
#5379=LINE('',#57665,#6791);
#5380=LINE('',#57666,#6792);
#5381=LINE('',#57678,#6793);
#5382=LINE('',#57680,#6794);
#5383=LINE('',#57682,#6795);
#5384=LINE('',#57696,#6796);
#5385=LINE('',#57697,#6797);
#5386=LINE('',#57779,#6798);
#5387=LINE('',#57781,#6799);
#5388=LINE('',#57783,#6800);
#5389=LINE('',#57796,#6801);
#5390=LINE('',#57797,#6802);
#5391=LINE('',#57874,#6803);
#5392=LINE('',#57876,#6804);
#5393=LINE('',#57878,#6805);
#5394=LINE('',#57891,#6806);
#5395=LINE('',#57892,#6807);
#5396=LINE('',#57934,#6808);
#5397=LINE('',#57936,#6809);
#5398=LINE('',#57938,#6810);
#5399=LINE('',#57952,#6811);
#5400=LINE('',#57953,#6812);
#5401=LINE('',#58021,#6813);
#5402=LINE('',#58023,#6814);
#5403=LINE('',#58025,#6815);
#5404=LINE('',#58038,#6816);
#5405=LINE('',#58039,#6817);
#5406=LINE('',#58116,#6818);
#5407=LINE('',#58118,#6819);
#5408=LINE('',#58120,#6820);
#5409=LINE('',#58133,#6821);
#5410=LINE('',#58134,#6822);
#5411=LINE('',#58211,#6823);
#5412=LINE('',#58213,#6824);
#5413=LINE('',#58215,#6825);
#5414=LINE('',#58228,#6826);
#5415=LINE('',#58229,#6827);
#5416=LINE('',#58909,#6828);
#5417=LINE('',#58911,#6829);
#5418=LINE('',#58913,#6830);
#5419=LINE('',#58915,#6831);
#5420=LINE('',#58938,#6832);
#5421=LINE('',#58943,#6833);
#5422=LINE('',#58946,#6834);
#5423=LINE('',#58948,#6835);
#5424=LINE('',#58950,#6836);
#5425=LINE('',#58952,#6837);
#5426=LINE('',#58954,#6838);
#5427=LINE('',#58956,#6839);
#5428=LINE('',#58958,#6840);
#5429=LINE('',#58960,#6841);
#5430=LINE('',#58962,#6842);
#5431=LINE('',#58969,#6843);
#5432=LINE('',#58973,#6844);
#5433=LINE('',#58977,#6845);
#5434=LINE('',#58987,#6846);
#5435=LINE('',#58990,#6847);
#5436=LINE('',#59000,#6848);
#5437=LINE('',#59003,#6849);
#5438=LINE('',#59013,#6850);
#5439=LINE('',#59016,#6851);
#5440=LINE('',#59026,#6852);
#5441=LINE('',#59029,#6853);
#5442=LINE('',#59073,#6854);
#5443=LINE('',#59152,#6855);
#5444=LINE('',#59231,#6856);
#5445=LINE('',#59313,#6857);
#5446=LINE('',#59354,#6858);
#5447=LINE('',#59356,#6859);
#5448=LINE('',#59367,#6860);
#5449=LINE('',#59372,#6861);
#5450=LINE('',#59375,#6862);
#5451=LINE('',#59379,#6863);
#5452=LINE('',#59385,#6864);
#5453=LINE('',#59388,#6865);
#5454=LINE('',#59390,#6866);
#5455=LINE('',#59394,#6867);
#5456=LINE('',#59402,#6868);
#5457=LINE('',#59406,#6869);
#5458=LINE('',#59411,#6870);
#5459=LINE('',#59413,#6871);
#5460=LINE('',#59415,#6872);
#5461=LINE('',#59417,#6873);
#5462=LINE('',#59419,#6874);
#5463=LINE('',#59421,#6875);
#5464=LINE('',#59423,#6876);
#5465=LINE('',#59425,#6877);
#5466=LINE('',#59427,#6878);
#5467=LINE('',#59429,#6879);
#5468=LINE('',#59431,#6880);
#5469=LINE('',#59433,#6881);
#5470=LINE('',#59435,#6882);
#5471=LINE('',#59437,#6883);
#5472=LINE('',#59439,#6884);
#5473=LINE('',#59441,#6885);
#5474=LINE('',#59443,#6886);
#5475=LINE('',#59445,#6887);
#5476=LINE('',#59447,#6888);
#5477=LINE('',#59449,#6889);
#5478=LINE('',#59451,#6890);
#5479=LINE('',#59453,#6891);
#5480=LINE('',#59455,#6892);
#5481=LINE('',#59457,#6893);
#5482=LINE('',#59459,#6894);
#5483=LINE('',#59461,#6895);
#5484=LINE('',#59463,#6896);
#5485=LINE('',#59465,#6897);
#5486=LINE('',#59467,#6898);
#5487=LINE('',#59469,#6899);
#5488=LINE('',#59471,#6900);
#5489=LINE('',#59473,#6901);
#5490=LINE('',#59475,#6902);
#5491=LINE('',#59477,#6903);
#5492=LINE('',#59479,#6904);
#5493=LINE('',#59481,#6905);
#5494=LINE('',#59483,#6906);
#5495=LINE('',#59485,#6907);
#5496=LINE('',#59487,#6908);
#5497=LINE('',#59489,#6909);
#5498=LINE('',#59491,#6910);
#5499=LINE('',#59493,#6911);
#5500=LINE('',#59495,#6912);
#5501=LINE('',#59497,#6913);
#5502=LINE('',#59499,#6914);
#5503=LINE('',#59501,#6915);
#5504=LINE('',#59503,#6916);
#5505=LINE('',#59505,#6917);
#5506=LINE('',#59507,#6918);
#5507=LINE('',#59509,#6919);
#5508=LINE('',#59511,#6920);
#5509=LINE('',#59513,#6921);
#5510=LINE('',#59515,#6922);
#5511=LINE('',#59517,#6923);
#5512=LINE('',#59519,#6924);
#5513=LINE('',#59521,#6925);
#5514=LINE('',#59523,#6926);
#5515=LINE('',#59525,#6927);
#5516=LINE('',#59527,#6928);
#5517=LINE('',#59529,#6929);
#5518=LINE('',#59531,#6930);
#5519=LINE('',#59533,#6931);
#5520=LINE('',#59535,#6932);
#5521=LINE('',#59537,#6933);
#5522=LINE('',#59539,#6934);
#5523=LINE('',#59541,#6935);
#5524=LINE('',#59543,#6936);
#5525=LINE('',#59545,#6937);
#5526=LINE('',#59547,#6938);
#5527=LINE('',#59549,#6939);
#5528=LINE('',#59551,#6940);
#5529=LINE('',#59553,#6941);
#5530=LINE('',#59555,#6942);
#5531=LINE('',#59557,#6943);
#5532=LINE('',#59559,#6944);
#5533=LINE('',#59561,#6945);
#5534=LINE('',#59563,#6946);
#5535=LINE('',#59565,#6947);
#5536=LINE('',#59567,#6948);
#5537=LINE('',#59569,#6949);
#5538=LINE('',#59571,#6950);
#5539=LINE('',#59573,#6951);
#5540=LINE('',#59575,#6952);
#5541=LINE('',#59577,#6953);
#5542=LINE('',#59579,#6954);
#5543=LINE('',#59581,#6955);
#5544=LINE('',#59583,#6956);
#5545=LINE('',#59585,#6957);
#5546=LINE('',#59587,#6958);
#5547=LINE('',#59589,#6959);
#5548=LINE('',#59591,#6960);
#5549=LINE('',#59593,#6961);
#5550=LINE('',#59595,#6962);
#5551=LINE('',#59597,#6963);
#5552=LINE('',#59599,#6964);
#5553=LINE('',#59601,#6965);
#5554=LINE('',#59603,#6966);
#5555=LINE('',#59605,#6967);
#5556=LINE('',#59607,#6968);
#5557=LINE('',#59609,#6969);
#5558=LINE('',#59611,#6970);
#5559=LINE('',#59613,#6971);
#5560=LINE('',#59615,#6972);
#5561=LINE('',#59617,#6973);
#5562=LINE('',#59619,#6974);
#5563=LINE('',#59621,#6975);
#5564=LINE('',#59623,#6976);
#5565=LINE('',#59625,#6977);
#5566=LINE('',#59627,#6978);
#5567=LINE('',#59629,#6979);
#5568=LINE('',#59631,#6980);
#5569=LINE('',#59633,#6981);
#5570=LINE('',#59635,#6982);
#5571=LINE('',#59637,#6983);
#5572=LINE('',#59639,#6984);
#5573=LINE('',#59641,#6985);
#5574=LINE('',#59643,#6986);
#5575=LINE('',#59645,#6987);
#5576=LINE('',#59647,#6988);
#5577=LINE('',#59649,#6989);
#5578=LINE('',#59651,#6990);
#5579=LINE('',#59653,#6991);
#5580=LINE('',#59655,#6992);
#5581=LINE('',#59657,#6993);
#5582=LINE('',#59659,#6994);
#5583=LINE('',#59661,#6995);
#5584=LINE('',#59663,#6996);
#5585=LINE('',#59665,#6997);
#5586=LINE('',#59667,#6998);
#5587=LINE('',#59669,#6999);
#5588=LINE('',#59671,#7000);
#5589=LINE('',#59673,#7001);
#5590=LINE('',#59675,#7002);
#5591=LINE('',#59677,#7003);
#5592=LINE('',#59679,#7004);
#5593=LINE('',#59681,#7005);
#5594=LINE('',#59683,#7006);
#5595=LINE('',#59685,#7007);
#5596=LINE('',#59687,#7008);
#5597=LINE('',#59689,#7009);
#5598=LINE('',#59691,#7010);
#5599=LINE('',#59693,#7011);
#5600=LINE('',#59695,#7012);
#5601=LINE('',#59697,#7013);
#5602=LINE('',#59699,#7014);
#5603=LINE('',#59701,#7015);
#5604=LINE('',#59703,#7016);
#5605=LINE('',#59705,#7017);
#5606=LINE('',#59707,#7018);
#5607=LINE('',#59708,#7019);
#5608=LINE('',#59714,#7020);
#5609=LINE('',#59718,#7021);
#5610=LINE('',#59720,#7022);
#5611=LINE('',#59722,#7023);
#5612=LINE('',#59724,#7024);
#5613=LINE('',#59726,#7025);
#5614=LINE('',#59728,#7026);
#5615=LINE('',#59730,#7027);
#5616=LINE('',#59732,#7028);
#5617=LINE('',#59734,#7029);
#5618=LINE('',#59736,#7030);
#5619=LINE('',#59738,#7031);
#5620=LINE('',#59740,#7032);
#5621=LINE('',#59742,#7033);
#5622=LINE('',#59744,#7034);
#5623=LINE('',#59746,#7035);
#5624=LINE('',#59748,#7036);
#5625=LINE('',#59750,#7037);
#5626=LINE('',#59752,#7038);
#5627=LINE('',#59754,#7039);
#5628=LINE('',#59756,#7040);
#5629=LINE('',#59758,#7041);
#5630=LINE('',#59760,#7042);
#5631=LINE('',#59762,#7043);
#5632=LINE('',#59764,#7044);
#5633=LINE('',#59766,#7045);
#5634=LINE('',#59768,#7046);
#5635=LINE('',#59770,#7047);
#5636=LINE('',#59772,#7048);
#5637=LINE('',#59774,#7049);
#5638=LINE('',#59776,#7050);
#5639=LINE('',#59778,#7051);
#5640=LINE('',#59780,#7052);
#5641=LINE('',#59782,#7053);
#5642=LINE('',#59784,#7054);
#5643=LINE('',#59786,#7055);
#5644=LINE('',#59788,#7056);
#5645=LINE('',#59790,#7057);
#5646=LINE('',#59792,#7058);
#5647=LINE('',#59794,#7059);
#5648=LINE('',#59796,#7060);
#5649=LINE('',#59798,#7061);
#5650=LINE('',#59800,#7062);
#5651=LINE('',#59802,#7063);
#5652=LINE('',#59804,#7064);
#5653=LINE('',#59806,#7065);
#5654=LINE('',#59808,#7066);
#5655=LINE('',#59810,#7067);
#5656=LINE('',#59812,#7068);
#5657=LINE('',#59814,#7069);
#5658=LINE('',#59816,#7070);
#5659=LINE('',#59818,#7071);
#5660=LINE('',#59820,#7072);
#5661=LINE('',#59822,#7073);
#5662=LINE('',#59824,#7074);
#5663=LINE('',#59826,#7075);
#5664=LINE('',#59828,#7076);
#5665=LINE('',#59830,#7077);
#5666=LINE('',#59832,#7078);
#5667=LINE('',#59834,#7079);
#5668=LINE('',#59836,#7080);
#5669=LINE('',#59838,#7081);
#5670=LINE('',#59840,#7082);
#5671=LINE('',#59842,#7083);
#5672=LINE('',#59844,#7084);
#5673=LINE('',#59846,#7085);
#5674=LINE('',#59848,#7086);
#5675=LINE('',#59850,#7087);
#5676=LINE('',#59852,#7088);
#5677=LINE('',#59854,#7089);
#5678=LINE('',#59856,#7090);
#5679=LINE('',#59858,#7091);
#5680=LINE('',#59860,#7092);
#5681=LINE('',#59862,#7093);
#5682=LINE('',#59864,#7094);
#5683=LINE('',#59866,#7095);
#5684=LINE('',#59868,#7096);
#5685=LINE('',#59870,#7097);
#5686=LINE('',#59872,#7098);
#5687=LINE('',#59874,#7099);
#5688=LINE('',#59876,#7100);
#5689=LINE('',#59878,#7101);
#5690=LINE('',#59880,#7102);
#5691=LINE('',#59882,#7103);
#5692=LINE('',#59884,#7104);
#5693=LINE('',#59886,#7105);
#5694=LINE('',#59888,#7106);
#5695=LINE('',#59890,#7107);
#5696=LINE('',#59892,#7108);
#5697=LINE('',#59894,#7109);
#5698=LINE('',#59896,#7110);
#5699=LINE('',#59898,#7111);
#5700=LINE('',#59900,#7112);
#5701=LINE('',#59902,#7113);
#5702=LINE('',#59904,#7114);
#5703=LINE('',#59906,#7115);
#5704=LINE('',#59908,#7116);
#5705=LINE('',#59910,#7117);
#5706=LINE('',#59912,#7118);
#5707=LINE('',#59914,#7119);
#5708=LINE('',#59916,#7120);
#5709=LINE('',#59918,#7121);
#5710=LINE('',#59920,#7122);
#5711=LINE('',#59922,#7123);
#5712=LINE('',#59924,#7124);
#5713=LINE('',#59926,#7125);
#5714=LINE('',#59928,#7126);
#5715=LINE('',#59930,#7127);
#5716=LINE('',#59932,#7128);
#5717=LINE('',#59934,#7129);
#5718=LINE('',#59936,#7130);
#5719=LINE('',#59938,#7131);
#5720=LINE('',#59940,#7132);
#5721=LINE('',#59942,#7133);
#5722=LINE('',#59944,#7134);
#5723=LINE('',#59946,#7135);
#5724=LINE('',#59948,#7136);
#5725=LINE('',#59950,#7137);
#5726=LINE('',#59952,#7138);
#5727=LINE('',#59954,#7139);
#5728=LINE('',#59956,#7140);
#5729=LINE('',#59958,#7141);
#5730=LINE('',#59960,#7142);
#5731=LINE('',#59962,#7143);
#5732=LINE('',#59964,#7144);
#5733=LINE('',#59966,#7145);
#5734=LINE('',#59968,#7146);
#5735=LINE('',#59970,#7147);
#5736=LINE('',#59972,#7148);
#5737=LINE('',#59974,#7149);
#5738=LINE('',#59976,#7150);
#5739=LINE('',#59978,#7151);
#5740=LINE('',#59980,#7152);
#5741=LINE('',#59982,#7153);
#5742=LINE('',#59984,#7154);
#5743=LINE('',#59986,#7155);
#5744=LINE('',#59988,#7156);
#5745=LINE('',#59990,#7157);
#5746=LINE('',#59992,#7158);
#5747=LINE('',#59994,#7159);
#5748=LINE('',#59996,#7160);
#5749=LINE('',#59998,#7161);
#5750=LINE('',#60000,#7162);
#5751=LINE('',#60002,#7163);
#5752=LINE('',#60004,#7164);
#5753=LINE('',#60006,#7165);
#5754=LINE('',#60008,#7166);
#5755=LINE('',#60010,#7167);
#5756=LINE('',#60012,#7168);
#5757=LINE('',#60014,#7169);
#5758=LINE('',#60015,#7170);
#5759=LINE('',#60020,#7171);
#5760=LINE('',#60024,#7172);
#5761=LINE('',#60027,#7173);
#5762=LINE('',#60029,#7174);
#5763=LINE('',#60030,#7175);
#5764=LINE('',#60032,#7176);
#5765=LINE('',#60034,#7177);
#5766=LINE('',#60036,#7178);
#5767=LINE('',#60038,#7179);
#5768=LINE('',#60040,#7180);
#5769=LINE('',#60042,#7181);
#5770=LINE('',#60044,#7182);
#5771=LINE('',#60046,#7183);
#5772=LINE('',#60048,#7184);
#5773=LINE('',#60050,#7185);
#5774=LINE('',#60052,#7186);
#5775=LINE('',#60054,#7187);
#5776=LINE('',#60056,#7188);
#5777=LINE('',#60058,#7189);
#5778=LINE('',#60060,#7190);
#5779=LINE('',#60062,#7191);
#5780=LINE('',#60064,#7192);
#5781=LINE('',#60066,#7193);
#5782=LINE('',#60068,#7194);
#5783=LINE('',#60070,#7195);
#5784=LINE('',#60072,#7196);
#5785=LINE('',#60074,#7197);
#5786=LINE('',#60076,#7198);
#5787=LINE('',#60078,#7199);
#5788=LINE('',#60080,#7200);
#5789=LINE('',#60082,#7201);
#5790=LINE('',#60084,#7202);
#5791=LINE('',#60086,#7203);
#5792=LINE('',#60088,#7204);
#5793=LINE('',#60090,#7205);
#5794=LINE('',#60092,#7206);
#5795=LINE('',#60094,#7207);
#5796=LINE('',#60096,#7208);
#5797=LINE('',#60098,#7209);
#5798=LINE('',#60100,#7210);
#5799=LINE('',#60102,#7211);
#5800=LINE('',#60104,#7212);
#5801=LINE('',#60106,#7213);
#5802=LINE('',#60108,#7214);
#5803=LINE('',#60110,#7215);
#5804=LINE('',#60112,#7216);
#5805=LINE('',#60114,#7217);
#5806=LINE('',#60116,#7218);
#5807=LINE('',#60118,#7219);
#5808=LINE('',#60120,#7220);
#5809=LINE('',#60122,#7221);
#5810=LINE('',#60124,#7222);
#5811=LINE('',#60126,#7223);
#5812=LINE('',#60128,#7224);
#5813=LINE('',#60130,#7225);
#5814=LINE('',#60132,#7226);
#5815=LINE('',#60134,#7227);
#5816=LINE('',#60136,#7228);
#5817=LINE('',#60138,#7229);
#5818=LINE('',#60140,#7230);
#5819=LINE('',#60142,#7231);
#5820=LINE('',#60144,#7232);
#5821=LINE('',#60146,#7233);
#5822=LINE('',#60148,#7234);
#5823=LINE('',#60150,#7235);
#5824=LINE('',#60152,#7236);
#5825=LINE('',#60154,#7237);
#5826=LINE('',#60156,#7238);
#5827=LINE('',#60158,#7239);
#5828=LINE('',#60160,#7240);
#5829=LINE('',#60162,#7241);
#5830=LINE('',#60164,#7242);
#5831=LINE('',#60166,#7243);
#5832=LINE('',#60168,#7244);
#5833=LINE('',#60170,#7245);
#5834=LINE('',#60172,#7246);
#5835=LINE('',#60174,#7247);
#5836=LINE('',#60176,#7248);
#5837=LINE('',#60178,#7249);
#5838=LINE('',#60180,#7250);
#5839=LINE('',#60182,#7251);
#5840=LINE('',#60184,#7252);
#5841=LINE('',#60186,#7253);
#5842=LINE('',#60188,#7254);
#5843=LINE('',#60190,#7255);
#5844=LINE('',#60192,#7256);
#5845=LINE('',#60194,#7257);
#5846=LINE('',#60196,#7258);
#5847=LINE('',#60198,#7259);
#5848=LINE('',#60200,#7260);
#5849=LINE('',#60202,#7261);
#5850=LINE('',#60204,#7262);
#5851=LINE('',#60206,#7263);
#5852=LINE('',#60208,#7264);
#5853=LINE('',#60210,#7265);
#5854=LINE('',#60212,#7266);
#5855=LINE('',#60214,#7267);
#5856=LINE('',#60216,#7268);
#5857=LINE('',#60218,#7269);
#5858=LINE('',#60220,#7270);
#5859=LINE('',#60222,#7271);
#5860=LINE('',#60224,#7272);
#5861=LINE('',#60226,#7273);
#5862=LINE('',#60228,#7274);
#5863=LINE('',#60230,#7275);
#5864=LINE('',#60232,#7276);
#5865=LINE('',#60234,#7277);
#5866=LINE('',#60236,#7278);
#5867=LINE('',#60238,#7279);
#5868=LINE('',#60240,#7280);
#5869=LINE('',#60242,#7281);
#5870=LINE('',#60244,#7282);
#5871=LINE('',#60246,#7283);
#5872=LINE('',#60248,#7284);
#5873=LINE('',#60250,#7285);
#5874=LINE('',#60252,#7286);
#5875=LINE('',#60254,#7287);
#5876=LINE('',#60256,#7288);
#5877=LINE('',#60258,#7289);
#5878=LINE('',#60260,#7290);
#5879=LINE('',#60262,#7291);
#5880=LINE('',#60264,#7292);
#5881=LINE('',#60266,#7293);
#5882=LINE('',#60268,#7294);
#5883=LINE('',#60270,#7295);
#5884=LINE('',#60272,#7296);
#5885=LINE('',#60274,#7297);
#5886=LINE('',#60276,#7298);
#5887=LINE('',#60278,#7299);
#5888=LINE('',#60280,#7300);
#5889=LINE('',#60282,#7301);
#5890=LINE('',#60284,#7302);
#5891=LINE('',#60286,#7303);
#5892=LINE('',#60288,#7304);
#5893=LINE('',#60290,#7305);
#5894=LINE('',#60292,#7306);
#5895=LINE('',#60294,#7307);
#5896=LINE('',#60296,#7308);
#5897=LINE('',#60298,#7309);
#5898=LINE('',#60300,#7310);
#5899=LINE('',#60302,#7311);
#5900=LINE('',#60304,#7312);
#5901=LINE('',#60306,#7313);
#5902=LINE('',#60308,#7314);
#5903=LINE('',#60310,#7315);
#5904=LINE('',#60312,#7316);
#5905=LINE('',#60314,#7317);
#5906=LINE('',#60316,#7318);
#5907=LINE('',#60318,#7319);
#5908=LINE('',#60320,#7320);
#5909=LINE('',#60322,#7321);
#5910=LINE('',#60324,#7322);
#5911=LINE('',#60326,#7323);
#5912=VECTOR('',#19684,3.5);
#5913=VECTOR('',#19689,3.5);
#5914=VECTOR('',#19692,3.5);
#5915=VECTOR('',#19695,3.5);
#5916=VECTOR('',#19698,3.5);
#5917=VECTOR('',#19701,3.5);
#5918=VECTOR('',#19704,3.5);
#5919=VECTOR('',#19707,3.5);
#5920=VECTOR('',#19710,3.5);
#5921=VECTOR('',#19713,3.5);
#5922=VECTOR('',#19716,3.5);
#5923=VECTOR('',#19719,3.5);
#5924=VECTOR('',#19722,3.5);
#5925=VECTOR('',#19725,3.5);
#5926=VECTOR('',#19728,3.5);
#5927=VECTOR('',#19731,3.5);
#5928=VECTOR('',#19780,2.872);
#5929=VECTOR('',#19785,2.872);
#5930=VECTOR('',#19788,2.872);
#5931=VECTOR('',#19791,2.872);
#5932=VECTOR('',#19794,2.872);
#5933=VECTOR('',#19797,2.872);
#5934=VECTOR('',#19800,2.872);
#5935=VECTOR('',#19803,2.872);
#5936=VECTOR('',#19806,2.872);
#5937=VECTOR('',#19809,2.872);
#5938=VECTOR('',#19812,2.872);
#5939=VECTOR('',#19815,2.872);
#5940=VECTOR('',#19818,2.872);
#5941=VECTOR('',#19821,2.872);
#5942=VECTOR('',#19824,2.872);
#5943=VECTOR('',#19827,2.872);
#5944=VECTOR('',#19832,9.87862393885688);
#5945=VECTOR('',#19839,10.3);
#5946=VECTOR('',#19848,10.);
#5947=VECTOR('',#19849,10.);
#5948=VECTOR('',#19850,10.);
#5949=VECTOR('',#19851,10.);
#5950=VECTOR('',#19852,10.);
#5951=VECTOR('',#19855,10.);
#5952=VECTOR('',#19856,10.);
#5953=VECTOR('',#19857,10.);
#5954=VECTOR('',#19860,10.);
#5955=VECTOR('',#19861,10.);
#5956=VECTOR('',#19862,10.);
#5957=VECTOR('',#19865,10.);
#5958=VECTOR('',#19866,10.);
#5959=VECTOR('',#19867,10.);
#5960=VECTOR('',#19870,10.);
#5961=VECTOR('',#19871,10.);
#5962=VECTOR('',#19872,10.);
#5963=VECTOR('',#19873,10.);
#5964=VECTOR('',#19874,10.);
#5965=VECTOR('',#19877,10.);
#5966=VECTOR('',#19878,10.);
#5967=VECTOR('',#19879,10.);
#5968=VECTOR('',#19882,10.);
#5969=VECTOR('',#19883,10.);
#5970=VECTOR('',#19884,10.);
#5971=VECTOR('',#19887,10.);
#5972=VECTOR('',#19888,10.);
#5973=VECTOR('',#19891,10.);
#5974=VECTOR('',#19892,10.);
#5975=VECTOR('',#19893,10.);
#5976=VECTOR('',#19894,10.);
#5977=VECTOR('',#19895,10.);
#5978=VECTOR('',#19898,10.);
#5979=VECTOR('',#19899,10.);
#5980=VECTOR('',#19900,10.);
#5981=VECTOR('',#19903,10.);
#5982=VECTOR('',#19904,10.);
#5983=VECTOR('',#19905,10.);
#5984=VECTOR('',#19908,10.);
#5985=VECTOR('',#19909,10.);
#5986=VECTOR('',#19912,10.);
#5987=VECTOR('',#19913,10.);
#5988=VECTOR('',#19914,10.);
#5989=VECTOR('',#19915,10.);
#5990=VECTOR('',#19916,10.);
#5991=VECTOR('',#19919,10.);
#5992=VECTOR('',#19920,10.);
#5993=VECTOR('',#19921,10.);
#5994=VECTOR('',#19924,10.);
#5995=VECTOR('',#19925,10.);
#5996=VECTOR('',#19926,10.);
#5997=VECTOR('',#19929,10.);
#5998=VECTOR('',#19930,10.);
#5999=VECTOR('',#19933,10.);
#6000=VECTOR('',#19934,10.);
#6001=VECTOR('',#19935,10.);
#6002=VECTOR('',#19936,10.);
#6003=VECTOR('',#19937,10.);
#6004=VECTOR('',#19940,10.);
#6005=VECTOR('',#19941,10.);
#6006=VECTOR('',#19942,10.);
#6007=VECTOR('',#19945,10.);
#6008=VECTOR('',#19946,10.);
#6009=VECTOR('',#19947,10.);
#6010=VECTOR('',#19950,10.);
#6011=VECTOR('',#19951,10.);
#6012=VECTOR('',#19954,10.);
#6013=VECTOR('',#19955,10.);
#6014=VECTOR('',#19956,10.);
#6015=VECTOR('',#19957,10.);
#6016=VECTOR('',#19958,10.);
#6017=VECTOR('',#19961,10.);
#6018=VECTOR('',#19962,10.);
#6019=VECTOR('',#19963,10.);
#6020=VECTOR('',#19966,10.);
#6021=VECTOR('',#19967,10.);
#6022=VECTOR('',#19970,10.);
#6023=VECTOR('',#19971,10.);
#6024=VECTOR('',#19972,10.);
#6025=VECTOR('',#19975,10.);
#6026=VECTOR('',#19976,10.);
#6027=VECTOR('',#19977,10.);
#6028=VECTOR('',#19978,10.);
#6029=VECTOR('',#19979,10.);
#6030=VECTOR('',#19982,10.);
#6031=VECTOR('',#19983,10.);
#6032=VECTOR('',#19984,10.);
#6033=VECTOR('',#19987,10.);
#6034=VECTOR('',#19988,10.);
#6035=VECTOR('',#19991,10.);
#6036=VECTOR('',#19992,10.);
#6037=VECTOR('',#19993,10.);
#6038=VECTOR('',#19994,10.);
#6039=VECTOR('',#19995,10.);
#6040=VECTOR('',#19998,10.);
#6041=VECTOR('',#19999,10.);
#6042=VECTOR('',#20000,10.);
#6043=VECTOR('',#20003,10.);
#6044=VECTOR('',#20004,10.);
#6045=VECTOR('',#20005,10.);
#6046=VECTOR('',#20008,10.);
#6047=VECTOR('',#20009,10.);
#6048=VECTOR('',#20010,10.);
#6049=VECTOR('',#20013,10.);
#6050=VECTOR('',#20014,10.);
#6051=VECTOR('',#20015,10.);
#6052=VECTOR('',#20016,10.);
#6053=VECTOR('',#20017,10.);
#6054=VECTOR('',#20020,10.);
#6055=VECTOR('',#20021,10.);
#6056=VECTOR('',#20022,10.);
#6057=VECTOR('',#20025,10.);
#6058=VECTOR('',#20026,10.);
#6059=VECTOR('',#20029,10.);
#6060=VECTOR('',#20030,10.);
#6061=VECTOR('',#20031,10.);
#6062=VECTOR('',#20034,10.);
#6063=VECTOR('',#20035,10.);
#6064=VECTOR('',#20036,10.);
#6065=VECTOR('',#20037,10.);
#6066=VECTOR('',#20038,10.);
#6067=VECTOR('',#20041,10.);
#6068=VECTOR('',#20042,10.);
#6069=VECTOR('',#20043,10.);
#6070=VECTOR('',#20046,10.);
#6071=VECTOR('',#20047,10.);
#6072=VECTOR('',#20050,10.);
#6073=VECTOR('',#20051,10.);
#6074=VECTOR('',#20052,10.);
#6075=VECTOR('',#20055,10.);
#6076=VECTOR('',#20056,10.);
#6077=VECTOR('',#20057,10.);
#6078=VECTOR('',#20058,10.);
#6079=VECTOR('',#20059,10.);
#6080=VECTOR('',#20062,10.);
#6081=VECTOR('',#20063,10.);
#6082=VECTOR('',#20064,10.);
#6083=VECTOR('',#20067,10.);
#6084=VECTOR('',#20068,10.);
#6085=VECTOR('',#20071,10.);
#6086=VECTOR('',#20072,10.);
#6087=VECTOR('',#20073,10.);
#6088=VECTOR('',#20076,10.);
#6089=VECTOR('',#20077,10.);
#6090=VECTOR('',#20078,10.);
#6091=VECTOR('',#20079,10.);
#6092=VECTOR('',#20080,10.);
#6093=VECTOR('',#20083,10.);
#6094=VECTOR('',#20084,10.);
#6095=VECTOR('',#20085,10.);
#6096=VECTOR('',#20088,10.);
#6097=VECTOR('',#20089,10.);
#6098=VECTOR('',#20092,10.);
#6099=VECTOR('',#20093,10.);
#6100=VECTOR('',#20218,8.95);
#6101=VECTOR('',#20229,9.2);
#6102=VECTOR('',#20234,8.95);
#6103=VECTOR('',#20243,9.2);
#6104=VECTOR('',#20248,10.);
#6105=VECTOR('',#20249,10.);
#6106=VECTOR('',#20270,10.);
#6107=VECTOR('',#20273,10.);
#6108=VECTOR('',#20282,10.);
#6109=VECTOR('',#20283,10.);
#6110=VECTOR('',#20298,10.);
#6111=VECTOR('',#20301,10.);
#6112=VECTOR('',#20310,10.);
#6113=VECTOR('',#20311,10.);
#6114=VECTOR('',#20326,10.);
#6115=VECTOR('',#20329,10.);
#6116=VECTOR('',#20338,10.);
#6117=VECTOR('',#20339,10.);
#6118=VECTOR('',#20354,10.);
#6119=VECTOR('',#20357,10.);
#6120=VECTOR('',#20366,10.);
#6121=VECTOR('',#20367,10.);
#6122=VECTOR('',#20382,10.);
#6123=VECTOR('',#20385,10.);
#6124=VECTOR('',#20428,10.);
#6125=VECTOR('',#20429,10.);
#6126=VECTOR('',#20436,10.);
#6127=VECTOR('',#20441,10.);
#6128=VECTOR('',#20450,10.);
#6129=VECTOR('',#20453,10.);
#6130=VECTOR('',#20464,10.);
#6131=VECTOR('',#20465,10.);
#6132=VECTOR('',#20474,10.);
#6133=VECTOR('',#20477,10.);
#6134=VECTOR('',#20488,10.);
#6135=VECTOR('',#20489,10.);
#6136=VECTOR('',#20498,10.);
#6137=VECTOR('',#20501,10.);
#6138=VECTOR('',#20512,10.);
#6139=VECTOR('',#20513,10.);
#6140=VECTOR('',#20522,10.);
#6141=VECTOR('',#20525,10.);
#6142=VECTOR('',#20536,10.);
#6143=VECTOR('',#20537,10.);
#6144=VECTOR('',#20546,10.);
#6145=VECTOR('',#20549,10.);
#6146=VECTOR('',#20560,10.);
#6147=VECTOR('',#20561,10.);
#6148=VECTOR('',#20566,10.);
#6149=VECTOR('',#20583,10.);
#6150=VECTOR('',#20586,10.);
#6151=VECTOR('',#20593,10.);
#6152=VECTOR('',#20730,8.5);
#6153=VECTOR('',#20743,9.2);
#6154=VECTOR('',#20746,7.7);
#6155=VECTOR('',#20821,10.);
#6156=VECTOR('',#20822,10.);
#6157=VECTOR('',#20825,10.);
#6158=VECTOR('',#20828,10.);
#6159=VECTOR('',#20831,10.);
#6160=VECTOR('',#20834,10.);
#6161=VECTOR('',#20837,10.);
#6162=VECTOR('',#20840,10.);
#6163=VECTOR('',#20845,10.);
#6164=VECTOR('',#20848,10.);
#6165=VECTOR('',#20851,10.);
#6166=VECTOR('',#20854,10.);
#6167=VECTOR('',#20857,10.);
#6168=VECTOR('',#20860,10.);
#6169=VECTOR('',#20867,13.);
#6170=VECTOR('',#20870,11.3);
#6171=VECTOR('',#20873,9.);
#6172=VECTOR('',#20878,9.);
#6173=VECTOR('',#20887,6.7);
#6174=VECTOR('',#20892,5.85);
#6175=VECTOR('',#20897,5.5);
#6176=VECTOR('',#20902,5.35);
#6177=VECTOR('',#20911,3.3);
#6178=VECTOR('',#20916,3.4);
#6179=VECTOR('',#20921,3.5);
#6180=VECTOR('',#20926,3.2);
#6181=VECTOR('',#20931,2.9);
#6182=VECTOR('',#20934,3.2);
#6183=VECTOR('',#20943,3.25);
#6184=VECTOR('',#20950,10.);
#6185=VECTOR('',#20951,10.);
#6186=VECTOR('',#20952,10.);
#6187=VECTOR('',#20953,10.);
#6188=VECTOR('',#20954,10.);
#6189=VECTOR('',#20955,10.);
#6190=VECTOR('',#20958,10.);
#6191=VECTOR('',#20959,10.);
#6192=VECTOR('',#20970,8.4);
#6193=VECTOR('',#20977,8.5);
#6194=VECTOR('',#20982,8.35);
#6195=VECTOR('',#20989,3.6575);
#6196=VECTOR('',#20994,3.505);
#6197=VECTOR('',#20999,3.6575);
#6198=VECTOR('',#21008,10.);
#6199=VECTOR('',#21009,10.);
#6200=VECTOR('',#21010,10.);
#6201=VECTOR('',#21011,10.);
#6202=VECTOR('',#21014,10.);
#6203=VECTOR('',#21015,10.);
#6204=VECTOR('',#21016,10.);
#6205=VECTOR('',#21021,10.);
#6206=VECTOR('',#21022,10.);
#6207=VECTOR('',#21023,10.);
#6208=VECTOR('',#21026,10.);
#6209=VECTOR('',#21027,10.);
#6210=VECTOR('',#21036,10.);
#6211=VECTOR('',#21037,10.);
#6212=VECTOR('',#21038,10.);
#6213=VECTOR('',#21039,10.);
#6214=VECTOR('',#21040,10.);
#6215=VECTOR('',#21041,10.);
#6216=VECTOR('',#21042,10.);
#6217=VECTOR('',#21043,10.);
#6218=VECTOR('',#21044,10.);
#6219=VECTOR('',#21045,10.);
#6220=VECTOR('',#21046,10.);
#6221=VECTOR('',#21047,10.);
#6222=VECTOR('',#21048,10.);
#6223=VECTOR('',#21049,10.);
#6224=VECTOR('',#21050,10.);
#6225=VECTOR('',#21051,10.);
#6226=VECTOR('',#21052,10.);
#6227=VECTOR('',#21053,10.);
#6228=VECTOR('',#21054,10.);
#6229=VECTOR('',#21055,10.);
#6230=VECTOR('',#21056,10.);
#6231=VECTOR('',#21057,10.);
#6232=VECTOR('',#21058,10.);
#6233=VECTOR('',#21059,10.);
#6234=VECTOR('',#21060,10.);
#6235=VECTOR('',#21061,10.);
#6236=VECTOR('',#21062,10.);
#6237=VECTOR('',#21063,10.);
#6238=VECTOR('',#21064,10.);
#6239=VECTOR('',#21065,10.);
#6240=VECTOR('',#21066,10.);
#6241=VECTOR('',#21067,10.);
#6242=VECTOR('',#21068,10.);
#6243=VECTOR('',#21069,10.);
#6244=VECTOR('',#21070,10.);
#6245=VECTOR('',#21071,10.);
#6246=VECTOR('',#21072,10.);
#6247=VECTOR('',#21073,10.);
#6248=VECTOR('',#21074,10.);
#6249=VECTOR('',#21075,10.);
#6250=VECTOR('',#21076,10.);
#6251=VECTOR('',#21077,10.);
#6252=VECTOR('',#21078,10.);
#6253=VECTOR('',#21079,10.);
#6254=VECTOR('',#21080,10.);
#6255=VECTOR('',#21081,10.);
#6256=VECTOR('',#21082,10.);
#6257=VECTOR('',#21083,10.);
#6258=VECTOR('',#21084,10.);
#6259=VECTOR('',#21085,10.);
#6260=VECTOR('',#21086,10.);
#6261=VECTOR('',#21087,10.);
#6262=VECTOR('',#21088,10.);
#6263=VECTOR('',#21089,10.);
#6264=VECTOR('',#21090,10.);
#6265=VECTOR('',#21091,10.);
#6266=VECTOR('',#21092,10.);
#6267=VECTOR('',#21093,10.);
#6268=VECTOR('',#21094,10.);
#6269=VECTOR('',#21095,10.);
#6270=VECTOR('',#21096,10.);
#6271=VECTOR('',#21097,10.);
#6272=VECTOR('',#21098,10.);
#6273=VECTOR('',#21099,10.);
#6274=VECTOR('',#21100,10.);
#6275=VECTOR('',#21101,10.);
#6276=VECTOR('',#21102,10.);
#6277=VECTOR('',#21103,10.);
#6278=VECTOR('',#21104,10.);
#6279=VECTOR('',#21105,10.);
#6280=VECTOR('',#21106,10.);
#6281=VECTOR('',#21107,10.);
#6282=VECTOR('',#21108,10.);
#6283=VECTOR('',#21109,10.);
#6284=VECTOR('',#21110,10.);
#6285=VECTOR('',#21111,10.);
#6286=VECTOR('',#21112,10.);
#6287=VECTOR('',#21113,10.);
#6288=VECTOR('',#21114,10.);
#6289=VECTOR('',#21115,10.);
#6290=VECTOR('',#21116,10.);
#6291=VECTOR('',#21117,10.);
#6292=VECTOR('',#21118,10.);
#6293=VECTOR('',#21119,10.);
#6294=VECTOR('',#21128,10.);
#6295=VECTOR('',#21129,10.);
#6296=VECTOR('',#21138,10.);
#6297=VECTOR('',#21139,10.);
#6298=VECTOR('',#21142,10.);
#6299=VECTOR('',#21145,10.);
#6300=VECTOR('',#21152,10.);
#6301=VECTOR('',#21153,10.);
#6302=VECTOR('',#21154,10.);
#6303=VECTOR('',#21155,10.);
#6304=VECTOR('',#21156,10.);
#6305=VECTOR('',#21157,10.);
#6306=VECTOR('',#21158,10.);
#6307=VECTOR('',#21159,10.);
#6308=VECTOR('',#21160,10.);
#6309=VECTOR('',#21161,10.);
#6310=VECTOR('',#21162,10.);
#6311=VECTOR('',#21163,10.);
#6312=VECTOR('',#21164,10.);
#6313=VECTOR('',#21165,10.);
#6314=VECTOR('',#21166,10.);
#6315=VECTOR('',#21167,10.);
#6316=VECTOR('',#21168,10.);
#6317=VECTOR('',#21169,10.);
#6318=VECTOR('',#21170,10.);
#6319=VECTOR('',#21171,10.);
#6320=VECTOR('',#21172,10.);
#6321=VECTOR('',#21173,10.);
#6322=VECTOR('',#21174,10.);
#6323=VECTOR('',#21175,10.);
#6324=VECTOR('',#21176,10.);
#6325=VECTOR('',#21177,10.);
#6326=VECTOR('',#21178,10.);
#6327=VECTOR('',#21179,10.);
#6328=VECTOR('',#21180,10.);
#6329=VECTOR('',#21181,10.);
#6330=VECTOR('',#21182,10.);
#6331=VECTOR('',#21183,10.);
#6332=VECTOR('',#21184,10.);
#6333=VECTOR('',#21185,10.);
#6334=VECTOR('',#21186,10.);
#6335=VECTOR('',#21187,10.);
#6336=VECTOR('',#21188,10.);
#6337=VECTOR('',#21189,10.);
#6338=VECTOR('',#21190,10.);
#6339=VECTOR('',#21191,10.);
#6340=VECTOR('',#21192,10.);
#6341=VECTOR('',#21193,10.);
#6342=VECTOR('',#21194,10.);
#6343=VECTOR('',#21195,10.);
#6344=VECTOR('',#21196,10.);
#6345=VECTOR('',#21197,10.);
#6346=VECTOR('',#21198,10.);
#6347=VECTOR('',#21199,10.);
#6348=VECTOR('',#21200,10.);
#6349=VECTOR('',#21201,10.);
#6350=VECTOR('',#21202,10.);
#6351=VECTOR('',#21203,10.);
#6352=VECTOR('',#21204,10.);
#6353=VECTOR('',#21205,10.);
#6354=VECTOR('',#21206,10.);
#6355=VECTOR('',#21207,10.);
#6356=VECTOR('',#21208,10.);
#6357=VECTOR('',#21209,10.);
#6358=VECTOR('',#21210,10.);
#6359=VECTOR('',#21211,10.);
#6360=VECTOR('',#21212,10.);
#6361=VECTOR('',#21213,10.);
#6362=VECTOR('',#21214,10.);
#6363=VECTOR('',#21215,10.);
#6364=VECTOR('',#21216,10.);
#6365=VECTOR('',#21217,10.);
#6366=VECTOR('',#21218,10.);
#6367=VECTOR('',#21219,10.);
#6368=VECTOR('',#21220,10.);
#6369=VECTOR('',#21221,10.);
#6370=VECTOR('',#21222,10.);
#6371=VECTOR('',#21223,10.);
#6372=VECTOR('',#21224,10.);
#6373=VECTOR('',#21225,10.);
#6374=VECTOR('',#21226,10.);
#6375=VECTOR('',#21227,10.);
#6376=VECTOR('',#21228,10.);
#6377=VECTOR('',#21229,10.);
#6378=VECTOR('',#21230,10.);
#6379=VECTOR('',#21231,10.);
#6380=VECTOR('',#21232,10.);
#6381=VECTOR('',#21233,10.);
#6382=VECTOR('',#21234,10.);
#6383=VECTOR('',#21235,10.);
#6384=VECTOR('',#21242,2.75);
#6385=VECTOR('',#21247,2.65);
#6386=VECTOR('',#21252,2.75);
#6387=VECTOR('',#21255,2.75);
#6388=VECTOR('',#21260,2.65);
#6389=VECTOR('',#21265,2.75);
#6390=VECTOR('',#21268,2.75);
#6391=VECTOR('',#21273,2.65);
#6392=VECTOR('',#21278,2.75);
#6393=VECTOR('',#21281,1.1);
#6394=VECTOR('',#21286,1.);
#6395=VECTOR('',#21289,10.);
#6396=VECTOR('',#21290,10.);
#6397=VECTOR('',#21291,10.);
#6398=VECTOR('',#21294,10.);
#6399=VECTOR('',#21295,10.);
#6400=VECTOR('',#21298,10.);
#6401=VECTOR('',#21299,10.);
#6402=VECTOR('',#21302,10.);
#6403=VECTOR('',#21303,10.);
#6404=VECTOR('',#21306,10.);
#6405=VECTOR('',#21307,10.);
#6406=VECTOR('',#21310,10.);
#6407=VECTOR('',#21311,10.);
#6408=VECTOR('',#21314,10.);
#6409=VECTOR('',#21315,10.);
#6410=VECTOR('',#21318,10.);
#6411=VECTOR('',#21319,10.);
#6412=VECTOR('',#21322,10.);
#6413=VECTOR('',#21323,10.);
#6414=VECTOR('',#21326,10.);
#6415=VECTOR('',#21327,10.);
#6416=VECTOR('',#21330,10.);
#6417=VECTOR('',#21331,10.);
#6418=VECTOR('',#21334,10.);
#6419=VECTOR('',#21335,10.);
#6420=VECTOR('',#21338,10.);
#6421=VECTOR('',#21339,10.);
#6422=VECTOR('',#21342,10.);
#6423=VECTOR('',#21347,10.);
#6424=VECTOR('',#21348,10.);
#6425=VECTOR('',#21349,10.);
#6426=VECTOR('',#21352,10.);
#6427=VECTOR('',#21353,10.);
#6428=VECTOR('',#21356,10.);
#6429=VECTOR('',#21357,10.);
#6430=VECTOR('',#21360,10.);
#6431=VECTOR('',#21361,10.);
#6432=VECTOR('',#21364,10.);
#6433=VECTOR('',#21365,10.);
#6434=VECTOR('',#21368,10.);
#6435=VECTOR('',#21369,10.);
#6436=VECTOR('',#21372,10.);
#6437=VECTOR('',#21373,10.);
#6438=VECTOR('',#21376,10.);
#6439=VECTOR('',#21377,10.);
#6440=VECTOR('',#21380,10.);
#6441=VECTOR('',#21381,10.);
#6442=VECTOR('',#21384,10.);
#6443=VECTOR('',#21385,10.);
#6444=VECTOR('',#21388,10.);
#6445=VECTOR('',#21389,10.);
#6446=VECTOR('',#21392,10.);
#6447=VECTOR('',#21393,10.);
#6448=VECTOR('',#21396,10.);
#6449=VECTOR('',#21397,10.);
#6450=VECTOR('',#21400,10.);
#6451=VECTOR('',#21405,10.);
#6452=VECTOR('',#21406,10.);
#6453=VECTOR('',#21407,10.);
#6454=VECTOR('',#21410,10.);
#6455=VECTOR('',#21411,10.);
#6456=VECTOR('',#21414,10.);
#6457=VECTOR('',#21415,10.);
#6458=VECTOR('',#21418,10.);
#6459=VECTOR('',#21419,10.);
#6460=VECTOR('',#21422,10.);
#6461=VECTOR('',#21423,10.);
#6462=VECTOR('',#21426,10.);
#6463=VECTOR('',#21427,10.);
#6464=VECTOR('',#21430,10.);
#6465=VECTOR('',#21431,10.);
#6466=VECTOR('',#21434,10.);
#6467=VECTOR('',#21435,10.);
#6468=VECTOR('',#21438,10.);
#6469=VECTOR('',#21439,10.);
#6470=VECTOR('',#21442,10.);
#6471=VECTOR('',#21443,10.);
#6472=VECTOR('',#21446,10.);
#6473=VECTOR('',#21447,10.);
#6474=VECTOR('',#21450,10.);
#6475=VECTOR('',#21451,10.);
#6476=VECTOR('',#21454,10.);
#6477=VECTOR('',#21455,10.);
#6478=VECTOR('',#21458,10.);
#6479=VECTOR('',#21463,10.);
#6480=VECTOR('',#21464,10.);
#6481=VECTOR('',#21465,10.);
#6482=VECTOR('',#21468,10.);
#6483=VECTOR('',#21469,10.);
#6484=VECTOR('',#21472,10.);
#6485=VECTOR('',#21473,10.);
#6486=VECTOR('',#21476,10.);
#6487=VECTOR('',#21477,10.);
#6488=VECTOR('',#21480,10.);
#6489=VECTOR('',#21481,10.);
#6490=VECTOR('',#21484,10.);
#6491=VECTOR('',#21485,10.);
#6492=VECTOR('',#21488,10.);
#6493=VECTOR('',#21489,10.);
#6494=VECTOR('',#21492,10.);
#6495=VECTOR('',#21493,10.);
#6496=VECTOR('',#21496,10.);
#6497=VECTOR('',#21497,10.);
#6498=VECTOR('',#21500,10.);
#6499=VECTOR('',#21501,10.);
#6500=VECTOR('',#21504,10.);
#6501=VECTOR('',#21505,10.);
#6502=VECTOR('',#21508,10.);
#6503=VECTOR('',#21509,10.);
#6504=VECTOR('',#21512,10.);
#6505=VECTOR('',#21513,10.);
#6506=VECTOR('',#21516,10.);
#6507=VECTOR('',#21521,10.);
#6508=VECTOR('',#21522,10.);
#6509=VECTOR('',#21523,10.);
#6510=VECTOR('',#21526,10.);
#6511=VECTOR('',#21527,10.);
#6512=VECTOR('',#21530,10.);
#6513=VECTOR('',#21531,10.);
#6514=VECTOR('',#21534,10.);
#6515=VECTOR('',#21535,10.);
#6516=VECTOR('',#21538,10.);
#6517=VECTOR('',#21539,10.);
#6518=VECTOR('',#21542,10.);
#6519=VECTOR('',#21543,10.);
#6520=VECTOR('',#21546,10.);
#6521=VECTOR('',#21547,10.);
#6522=VECTOR('',#21550,10.);
#6523=VECTOR('',#21551,10.);
#6524=VECTOR('',#21554,10.);
#6525=VECTOR('',#21555,10.);
#6526=VECTOR('',#21558,10.);
#6527=VECTOR('',#21559,10.);
#6528=VECTOR('',#21562,10.);
#6529=VECTOR('',#21563,10.);
#6530=VECTOR('',#21566,10.);
#6531=VECTOR('',#21567,10.);
#6532=VECTOR('',#21570,10.);
#6533=VECTOR('',#21571,10.);
#6534=VECTOR('',#21574,10.);
#6535=VECTOR('',#21579,10.);
#6536=VECTOR('',#21580,10.);
#6537=VECTOR('',#21581,10.);
#6538=VECTOR('',#21584,10.);
#6539=VECTOR('',#21585,10.);
#6540=VECTOR('',#21588,10.);
#6541=VECTOR('',#21589,10.);
#6542=VECTOR('',#21592,10.);
#6543=VECTOR('',#21593,10.);
#6544=VECTOR('',#21596,10.);
#6545=VECTOR('',#21597,10.);
#6546=VECTOR('',#21600,10.);
#6547=VECTOR('',#21601,10.);
#6548=VECTOR('',#21604,10.);
#6549=VECTOR('',#21605,10.);
#6550=VECTOR('',#21608,10.);
#6551=VECTOR('',#21609,10.);
#6552=VECTOR('',#21612,10.);
#6553=VECTOR('',#21613,10.);
#6554=VECTOR('',#21616,10.);
#6555=VECTOR('',#21617,10.);
#6556=VECTOR('',#21620,10.);
#6557=VECTOR('',#21621,10.);
#6558=VECTOR('',#21624,10.);
#6559=VECTOR('',#21625,10.);
#6560=VECTOR('',#21628,10.);
#6561=VECTOR('',#21629,10.);
#6562=VECTOR('',#21632,10.);
#6563=VECTOR('',#21637,10.);
#6564=VECTOR('',#21638,10.);
#6565=VECTOR('',#21639,10.);
#6566=VECTOR('',#21642,10.);
#6567=VECTOR('',#21643,10.);
#6568=VECTOR('',#21646,10.);
#6569=VECTOR('',#21647,10.);
#6570=VECTOR('',#21650,10.);
#6571=VECTOR('',#21651,10.);
#6572=VECTOR('',#21654,10.);
#6573=VECTOR('',#21655,10.);
#6574=VECTOR('',#21658,10.);
#6575=VECTOR('',#21659,10.);
#6576=VECTOR('',#21662,10.);
#6577=VECTOR('',#21663,10.);
#6578=VECTOR('',#21666,10.);
#6579=VECTOR('',#21667,10.);
#6580=VECTOR('',#21670,10.);
#6581=VECTOR('',#21671,10.);
#6582=VECTOR('',#21674,10.);
#6583=VECTOR('',#21675,10.);
#6584=VECTOR('',#21678,10.);
#6585=VECTOR('',#21679,10.);
#6586=VECTOR('',#21682,10.);
#6587=VECTOR('',#21683,10.);
#6588=VECTOR('',#21686,10.);
#6589=VECTOR('',#21687,10.);
#6590=VECTOR('',#21690,10.);
#6591=VECTOR('',#21695,10.);
#6592=VECTOR('',#21696,10.);
#6593=VECTOR('',#21697,10.);
#6594=VECTOR('',#21700,10.);
#6595=VECTOR('',#21701,10.);
#6596=VECTOR('',#21704,10.);
#6597=VECTOR('',#21705,10.);
#6598=VECTOR('',#21708,10.);
#6599=VECTOR('',#21709,10.);
#6600=VECTOR('',#21712,10.);
#6601=VECTOR('',#21713,10.);
#6602=VECTOR('',#21716,10.);
#6603=VECTOR('',#21717,10.);
#6604=VECTOR('',#21720,10.);
#6605=VECTOR('',#21721,10.);
#6606=VECTOR('',#21724,10.);
#6607=VECTOR('',#21725,10.);
#6608=VECTOR('',#21728,10.);
#6609=VECTOR('',#21729,10.);
#6610=VECTOR('',#21732,10.);
#6611=VECTOR('',#21733,10.);
#6612=VECTOR('',#21736,10.);
#6613=VECTOR('',#21737,10.);
#6614=VECTOR('',#21740,10.);
#6615=VECTOR('',#21741,10.);
#6616=VECTOR('',#21744,10.);
#6617=VECTOR('',#21745,10.);
#6618=VECTOR('',#21748,10.);
#6619=VECTOR('',#21753,10.);
#6620=VECTOR('',#21754,10.);
#6621=VECTOR('',#21755,10.);
#6622=VECTOR('',#21758,10.);
#6623=VECTOR('',#21759,10.);
#6624=VECTOR('',#21762,10.);
#6625=VECTOR('',#21763,10.);
#6626=VECTOR('',#21766,10.);
#6627=VECTOR('',#21767,10.);
#6628=VECTOR('',#21770,10.);
#6629=VECTOR('',#21771,10.);
#6630=VECTOR('',#21774,10.);
#6631=VECTOR('',#21775,10.);
#6632=VECTOR('',#21778,10.);
#6633=VECTOR('',#21779,10.);
#6634=VECTOR('',#21782,10.);
#6635=VECTOR('',#21783,10.);
#6636=VECTOR('',#21786,10.);
#6637=VECTOR('',#21787,10.);
#6638=VECTOR('',#21790,10.);
#6639=VECTOR('',#21791,10.);
#6640=VECTOR('',#21794,10.);
#6641=VECTOR('',#21795,10.);
#6642=VECTOR('',#21798,10.);
#6643=VECTOR('',#21799,10.);
#6644=VECTOR('',#21802,10.);
#6645=VECTOR('',#21803,10.);
#6646=VECTOR('',#21806,10.);
#6647=VECTOR('',#21811,10.);
#6648=VECTOR('',#21812,10.);
#6649=VECTOR('',#21813,10.);
#6650=VECTOR('',#21816,10.);
#6651=VECTOR('',#21817,10.);
#6652=VECTOR('',#21820,10.);
#6653=VECTOR('',#21821,10.);
#6654=VECTOR('',#21824,10.);
#6655=VECTOR('',#21825,10.);
#6656=VECTOR('',#21828,10.);
#6657=VECTOR('',#21829,10.);
#6658=VECTOR('',#21832,10.);
#6659=VECTOR('',#21833,10.);
#6660=VECTOR('',#21836,10.);
#6661=VECTOR('',#21837,10.);
#6662=VECTOR('',#21840,10.);
#6663=VECTOR('',#21841,10.);
#6664=VECTOR('',#21844,10.);
#6665=VECTOR('',#21845,10.);
#6666=VECTOR('',#21848,10.);
#6667=VECTOR('',#21849,10.);
#6668=VECTOR('',#21852,10.);
#6669=VECTOR('',#21853,10.);
#6670=VECTOR('',#21856,10.);
#6671=VECTOR('',#21857,10.);
#6672=VECTOR('',#21860,10.);
#6673=VECTOR('',#21861,10.);
#6674=VECTOR('',#21864,10.);
#6675=VECTOR('',#21869,10.);
#6676=VECTOR('',#21870,10.);
#6677=VECTOR('',#21871,10.);
#6678=VECTOR('',#21874,10.);
#6679=VECTOR('',#21875,10.);
#6680=VECTOR('',#21878,10.);
#6681=VECTOR('',#21879,10.);
#6682=VECTOR('',#21882,10.);
#6683=VECTOR('',#21883,10.);
#6684=VECTOR('',#21886,10.);
#6685=VECTOR('',#21887,10.);
#6686=VECTOR('',#21890,10.);
#6687=VECTOR('',#21891,10.);
#6688=VECTOR('',#21894,10.);
#6689=VECTOR('',#21895,10.);
#6690=VECTOR('',#21898,10.);
#6691=VECTOR('',#21899,10.);
#6692=VECTOR('',#21902,10.);
#6693=VECTOR('',#21903,10.);
#6694=VECTOR('',#21906,10.);
#6695=VECTOR('',#21907,10.);
#6696=VECTOR('',#21910,10.);
#6697=VECTOR('',#21911,10.);
#6698=VECTOR('',#21914,10.);
#6699=VECTOR('',#21915,10.);
#6700=VECTOR('',#21918,10.);
#6701=VECTOR('',#21919,10.);
#6702=VECTOR('',#21922,10.);
#6703=VECTOR('',#21927,10.);
#6704=VECTOR('',#21928,10.);
#6705=VECTOR('',#21929,10.);
#6706=VECTOR('',#21932,10.);
#6707=VECTOR('',#21933,10.);
#6708=VECTOR('',#21936,10.);
#6709=VECTOR('',#21937,10.);
#6710=VECTOR('',#21940,10.);
#6711=VECTOR('',#21941,10.);
#6712=VECTOR('',#21944,10.);
#6713=VECTOR('',#21945,10.);
#6714=VECTOR('',#21948,10.);
#6715=VECTOR('',#21949,10.);
#6716=VECTOR('',#21952,10.);
#6717=VECTOR('',#21953,10.);
#6718=VECTOR('',#21956,10.);
#6719=VECTOR('',#21957,10.);
#6720=VECTOR('',#21960,10.);
#6721=VECTOR('',#21961,10.);
#6722=VECTOR('',#21964,10.);
#6723=VECTOR('',#21965,10.);
#6724=VECTOR('',#21968,10.);
#6725=VECTOR('',#21969,10.);
#6726=VECTOR('',#21972,10.);
#6727=VECTOR('',#21973,10.);
#6728=VECTOR('',#21976,10.);
#6729=VECTOR('',#21977,10.);
#6730=VECTOR('',#21980,10.);
#6731=VECTOR('',#21985,5.85);
#6732=VECTOR('',#21986,5.85);
#6733=VECTOR('',#21995,0.600000000000001);
#6734=VECTOR('',#22004,0.6);
#6735=VECTOR('',#22013,0.600000000000001);
#6736=VECTOR('',#22022,0.600000000000001);
#6737=VECTOR('',#22031,0.6);
#6738=VECTOR('',#22040,0.600000000000001);
#6739=VECTOR('',#22049,6.6);
#6740=VECTOR('',#22064,7.6);
#6741=VECTOR('',#22069,5.65);
#6742=VECTOR('',#22076,5.75);
#6743=VECTOR('',#22085,8.4);
#6744=VECTOR('',#22090,8.5);
#6745=VECTOR('',#22095,8.4);
#6746=VECTOR('',#22104,7.7);
#6747=VECTOR('',#22107,7.6);
#6748=VECTOR('',#22112,7.45);
#6749=VECTOR('',#22119,3.6575);
#6750=VECTOR('',#22124,3.505);
#6751=VECTOR('',#22129,3.6575);
#6752=VECTOR('',#22138,10.);
#6753=VECTOR('',#22139,10.);
#6754=VECTOR('',#22140,10.);
#6755=VECTOR('',#22141,10.);
#6756=VECTOR('',#22142,10.);
#6757=VECTOR('',#22143,10.);
#6758=VECTOR('',#22146,10.);
#6759=VECTOR('',#22147,10.);
#6760=VECTOR('',#22192,39.);
#6761=VECTOR('',#22281,3.675);
#6762=VECTOR('',#22292,3.525);
#6763=VECTOR('',#22299,3.675);
#6764=VECTOR('',#22418,38.75);
#6765=VECTOR('',#22425,8.95);
#6766=VECTOR('',#22430,8.7);
#6767=VECTOR('',#22433,8.4);
#6768=VECTOR('',#22438,10.);
#6769=VECTOR('',#22439,10.);
#6770=VECTOR('',#22440,10.);
#6771=VECTOR('',#22443,10.);
#6772=VECTOR('',#22444,10.);
#6773=VECTOR('',#22447,10.);
#6774=VECTOR('',#22448,10.);
#6775=VECTOR('',#22449,10.);
#6776=VECTOR('',#22452,10.);
#6777=VECTOR('',#22453,10.);
#6778=VECTOR('',#22456,10.);
#6779=VECTOR('',#22457,10.);
#6780=VECTOR('',#22458,10.);
#6781=VECTOR('',#22461,10.);
#6782=VECTOR('',#22462,10.);
#6783=VECTOR('',#22465,10.);
#6784=VECTOR('',#22466,10.);
#6785=VECTOR('',#22467,10.);
#6786=VECTOR('',#22470,10.);
#6787=VECTOR('',#22471,10.);
#6788=VECTOR('',#22478,10.);
#6789=VECTOR('',#22479,10.);
#6790=VECTOR('',#22480,10.);
#6791=VECTOR('',#22483,10.);
#6792=VECTOR('',#22484,10.);
#6793=VECTOR('',#22487,10.);
#6794=VECTOR('',#22488,10.);
#6795=VECTOR('',#22489,10.);
#6796=VECTOR('',#22492,10.);
#6797=VECTOR('',#22493,10.);
#6798=VECTOR('',#22496,10.);
#6799=VECTOR('',#22497,10.);
#6800=VECTOR('',#22498,10.);
#6801=VECTOR('',#22501,10.);
#6802=VECTOR('',#22502,10.);
#6803=VECTOR('',#22505,10.);
#6804=VECTOR('',#22506,10.);
#6805=VECTOR('',#22507,10.);
#6806=VECTOR('',#22510,10.);
#6807=VECTOR('',#22511,10.);
#6808=VECTOR('',#22514,10.);
#6809=VECTOR('',#22515,10.);
#6810=VECTOR('',#22516,10.);
#6811=VECTOR('',#22519,10.);
#6812=VECTOR('',#22520,10.);
#6813=VECTOR('',#22523,10.);
#6814=VECTOR('',#22524,10.);
#6815=VECTOR('',#22525,10.);
#6816=VECTOR('',#22528,10.);
#6817=VECTOR('',#22529,10.);
#6818=VECTOR('',#22532,10.);
#6819=VECTOR('',#22533,10.);
#6820=VECTOR('',#22534,10.);
#6821=VECTOR('',#22537,10.);
#6822=VECTOR('',#22538,10.);
#6823=VECTOR('',#22541,10.);
#6824=VECTOR('',#22542,10.);
#6825=VECTOR('',#22543,10.);
#6826=VECTOR('',#22546,10.);
#6827=VECTOR('',#22547,10.);
#6828=VECTOR('',#22550,10.);
#6829=VECTOR('',#22553,10.);
#6830=VECTOR('',#22556,10.);
#6831=VECTOR('',#22559,10.);
#6832=VECTOR('',#22600,3.8);
#6833=VECTOR('',#22605,3.8);
#6834=VECTOR('',#22610,10.);
#6835=VECTOR('',#22613,10.);
#6836=VECTOR('',#22616,10.);
#6837=VECTOR('',#22619,10.);
#6838=VECTOR('',#22622,10.);
#6839=VECTOR('',#22625,10.);
#6840=VECTOR('',#22628,10.);
#6841=VECTOR('',#22631,10.);
#6842=VECTOR('',#22634,3.55);
#6843=VECTOR('',#22643,6.35);
#6844=VECTOR('',#22648,6.5);
#6845=VECTOR('',#22653,6.25);
#6846=VECTOR('',#22666,10.);
#6847=VECTOR('',#22669,10.);
#6848=VECTOR('',#22682,10.);
#6849=VECTOR('',#22685,10.);
#6850=VECTOR('',#22698,10.);
#6851=VECTOR('',#22701,10.);
#6852=VECTOR('',#22714,10.);
#6853=VECTOR('',#22717,10.);
#6854=VECTOR('',#22724,1.1);
#6855=VECTOR('',#22727,1.1);
#6856=VECTOR('',#22730,1.1);
#6857=VECTOR('',#22733,1.1);
#6858=VECTOR('',#22738,8.45);
#6859=VECTOR('',#22739,8.45);
#6860=VECTOR('',#22754,8.8);
#6861=VECTOR('',#22759,8.6);
#6862=VECTOR('',#22764,8.8);
#6863=VECTOR('',#22769,8.6);
#6864=VECTOR('',#22776,5.67);
#6865=VECTOR('',#22781,5.52);
#6866=VECTOR('',#22782,5.52);
#6867=VECTOR('',#22787,5.67);
#6868=VECTOR('',#22798,0.650000000000001);
#6869=VECTOR('',#22803,0.55);
#6870=VECTOR('',#22808,10.);
#6871=VECTOR('',#22809,10.);
#6872=VECTOR('',#22810,10.);
#6873=VECTOR('',#22811,10.);
#6874=VECTOR('',#22812,10.);
#6875=VECTOR('',#22813,10.);
#6876=VECTOR('',#22814,10.);
#6877=VECTOR('',#22815,10.);
#6878=VECTOR('',#22816,10.);
#6879=VECTOR('',#22817,10.);
#6880=VECTOR('',#22818,10.);
#6881=VECTOR('',#22819,10.);
#6882=VECTOR('',#22820,10.);
#6883=VECTOR('',#22821,10.);
#6884=VECTOR('',#22822,10.);
#6885=VECTOR('',#22823,10.);
#6886=VECTOR('',#22824,10.);
#6887=VECTOR('',#22825,10.);
#6888=VECTOR('',#22826,10.);
#6889=VECTOR('',#22827,10.);
#6890=VECTOR('',#22828,10.);
#6891=VECTOR('',#22829,10.);
#6892=VECTOR('',#22830,10.);
#6893=VECTOR('',#22831,10.);
#6894=VECTOR('',#22832,10.);
#6895=VECTOR('',#22833,10.);
#6896=VECTOR('',#22834,10.);
#6897=VECTOR('',#22835,10.);
#6898=VECTOR('',#22836,10.);
#6899=VECTOR('',#22837,10.);
#6900=VECTOR('',#22838,10.);
#6901=VECTOR('',#22839,10.);
#6902=VECTOR('',#22840,10.);
#6903=VECTOR('',#22841,10.);
#6904=VECTOR('',#22842,10.);
#6905=VECTOR('',#22843,10.);
#6906=VECTOR('',#22844,10.);
#6907=VECTOR('',#22845,10.);
#6908=VECTOR('',#22846,10.);
#6909=VECTOR('',#22847,10.);
#6910=VECTOR('',#22848,10.);
#6911=VECTOR('',#22849,10.);
#6912=VECTOR('',#22850,10.);
#6913=VECTOR('',#22851,10.);
#6914=VECTOR('',#22852,10.);
#6915=VECTOR('',#22853,10.);
#6916=VECTOR('',#22854,10.);
#6917=VECTOR('',#22855,10.);
#6918=VECTOR('',#22856,10.);
#6919=VECTOR('',#22857,10.);
#6920=VECTOR('',#22858,10.);
#6921=VECTOR('',#22859,10.);
#6922=VECTOR('',#22860,10.);
#6923=VECTOR('',#22861,10.);
#6924=VECTOR('',#22862,10.);
#6925=VECTOR('',#22863,10.);
#6926=VECTOR('',#22864,10.);
#6927=VECTOR('',#22865,10.);
#6928=VECTOR('',#22866,10.);
#6929=VECTOR('',#22867,10.);
#6930=VECTOR('',#22868,10.);
#6931=VECTOR('',#22869,10.);
#6932=VECTOR('',#22870,10.);
#6933=VECTOR('',#22871,10.);
#6934=VECTOR('',#22872,10.);
#6935=VECTOR('',#22873,10.);
#6936=VECTOR('',#22874,10.);
#6937=VECTOR('',#22875,10.);
#6938=VECTOR('',#22876,10.);
#6939=VECTOR('',#22877,10.);
#6940=VECTOR('',#22878,10.);
#6941=VECTOR('',#22879,10.);
#6942=VECTOR('',#22880,10.);
#6943=VECTOR('',#22881,10.);
#6944=VECTOR('',#22882,10.);
#6945=VECTOR('',#22883,10.);
#6946=VECTOR('',#22884,10.);
#6947=VECTOR('',#22885,10.);
#6948=VECTOR('',#22886,10.);
#6949=VECTOR('',#22887,10.);
#6950=VECTOR('',#22888,10.);
#6951=VECTOR('',#22889,10.);
#6952=VECTOR('',#22890,10.);
#6953=VECTOR('',#22891,10.);
#6954=VECTOR('',#22892,10.);
#6955=VECTOR('',#22893,10.);
#6956=VECTOR('',#22894,10.);
#6957=VECTOR('',#22895,10.);
#6958=VECTOR('',#22896,10.);
#6959=VECTOR('',#22897,10.);
#6960=VECTOR('',#22898,10.);
#6961=VECTOR('',#22899,10.);
#6962=VECTOR('',#22900,10.);
#6963=VECTOR('',#22901,10.);
#6964=VECTOR('',#22902,10.);
#6965=VECTOR('',#22903,10.);
#6966=VECTOR('',#22904,10.);
#6967=VECTOR('',#22905,10.);
#6968=VECTOR('',#22906,10.);
#6969=VECTOR('',#22907,10.);
#6970=VECTOR('',#22908,10.);
#6971=VECTOR('',#22909,10.);
#6972=VECTOR('',#22910,10.);
#6973=VECTOR('',#22911,10.);
#6974=VECTOR('',#22912,10.);
#6975=VECTOR('',#22913,10.);
#6976=VECTOR('',#22914,10.);
#6977=VECTOR('',#22915,10.);
#6978=VECTOR('',#22916,10.);
#6979=VECTOR('',#22917,10.);
#6980=VECTOR('',#22918,10.);
#6981=VECTOR('',#22919,10.);
#6982=VECTOR('',#22920,10.);
#6983=VECTOR('',#22921,10.);
#6984=VECTOR('',#22922,10.);
#6985=VECTOR('',#22923,10.);
#6986=VECTOR('',#22924,10.);
#6987=VECTOR('',#22925,10.);
#6988=VECTOR('',#22926,10.);
#6989=VECTOR('',#22927,10.);
#6990=VECTOR('',#22928,10.);
#6991=VECTOR('',#22929,10.);
#6992=VECTOR('',#22930,10.);
#6993=VECTOR('',#22931,10.);
#6994=VECTOR('',#22932,10.);
#6995=VECTOR('',#22933,10.);
#6996=VECTOR('',#22934,10.);
#6997=VECTOR('',#22935,10.);
#6998=VECTOR('',#22936,10.);
#6999=VECTOR('',#22937,10.);
#7000=VECTOR('',#22938,10.);
#7001=VECTOR('',#22939,10.);
#7002=VECTOR('',#22940,10.);
#7003=VECTOR('',#22941,10.);
#7004=VECTOR('',#22942,10.);
#7005=VECTOR('',#22943,10.);
#7006=VECTOR('',#22944,10.);
#7007=VECTOR('',#22945,10.);
#7008=VECTOR('',#22946,10.);
#7009=VECTOR('',#22947,10.);
#7010=VECTOR('',#22948,10.);
#7011=VECTOR('',#22949,10.);
#7012=VECTOR('',#22950,10.);
#7013=VECTOR('',#22951,10.);
#7014=VECTOR('',#22952,10.);
#7015=VECTOR('',#22953,10.);
#7016=VECTOR('',#22954,10.);
#7017=VECTOR('',#22955,10.);
#7018=VECTOR('',#22956,10.);
#7019=VECTOR('',#22957,10.);
#7020=VECTOR('',#22964,0.650000000000001);
#7021=VECTOR('',#22967,10.);
#7022=VECTOR('',#22968,10.);
#7023=VECTOR('',#22969,10.);
#7024=VECTOR('',#22970,10.);
#7025=VECTOR('',#22971,10.);
#7026=VECTOR('',#22972,10.);
#7027=VECTOR('',#22973,10.);
#7028=VECTOR('',#22974,10.);
#7029=VECTOR('',#22975,10.);
#7030=VECTOR('',#22976,10.);
#7031=VECTOR('',#22977,10.);
#7032=VECTOR('',#22978,10.);
#7033=VECTOR('',#22979,10.);
#7034=VECTOR('',#22980,10.);
#7035=VECTOR('',#22981,10.);
#7036=VECTOR('',#22982,10.);
#7037=VECTOR('',#22983,10.);
#7038=VECTOR('',#22984,10.);
#7039=VECTOR('',#22985,10.);
#7040=VECTOR('',#22986,10.);
#7041=VECTOR('',#22987,10.);
#7042=VECTOR('',#22988,10.);
#7043=VECTOR('',#22989,10.);
#7044=VECTOR('',#22990,10.);
#7045=VECTOR('',#22991,10.);
#7046=VECTOR('',#22992,10.);
#7047=VECTOR('',#22993,10.);
#7048=VECTOR('',#22994,10.);
#7049=VECTOR('',#22995,10.);
#7050=VECTOR('',#22996,10.);
#7051=VECTOR('',#22997,10.);
#7052=VECTOR('',#22998,10.);
#7053=VECTOR('',#22999,10.);
#7054=VECTOR('',#23000,10.);
#7055=VECTOR('',#23001,10.);
#7056=VECTOR('',#23002,10.);
#7057=VECTOR('',#23003,10.);
#7058=VECTOR('',#23004,10.);
#7059=VECTOR('',#23005,10.);
#7060=VECTOR('',#23006,10.);
#7061=VECTOR('',#23007,10.);
#7062=VECTOR('',#23008,10.);
#7063=VECTOR('',#23009,10.);
#7064=VECTOR('',#23010,10.);
#7065=VECTOR('',#23011,10.);
#7066=VECTOR('',#23012,10.);
#7067=VECTOR('',#23013,10.);
#7068=VECTOR('',#23014,10.);
#7069=VECTOR('',#23015,10.);
#7070=VECTOR('',#23016,10.);
#7071=VECTOR('',#23017,10.);
#7072=VECTOR('',#23018,10.);
#7073=VECTOR('',#23019,10.);
#7074=VECTOR('',#23020,10.);
#7075=VECTOR('',#23021,10.);
#7076=VECTOR('',#23022,10.);
#7077=VECTOR('',#23023,10.);
#7078=VECTOR('',#23024,10.);
#7079=VECTOR('',#23025,10.);
#7080=VECTOR('',#23026,10.);
#7081=VECTOR('',#23027,10.);
#7082=VECTOR('',#23028,10.);
#7083=VECTOR('',#23029,10.);
#7084=VECTOR('',#23030,10.);
#7085=VECTOR('',#23031,10.);
#7086=VECTOR('',#23032,10.);
#7087=VECTOR('',#23033,10.);
#7088=VECTOR('',#23034,10.);
#7089=VECTOR('',#23035,10.);
#7090=VECTOR('',#23036,10.);
#7091=VECTOR('',#23037,10.);
#7092=VECTOR('',#23038,10.);
#7093=VECTOR('',#23039,10.);
#7094=VECTOR('',#23040,10.);
#7095=VECTOR('',#23041,10.);
#7096=VECTOR('',#23042,10.);
#7097=VECTOR('',#23043,10.);
#7098=VECTOR('',#23044,10.);
#7099=VECTOR('',#23045,10.);
#7100=VECTOR('',#23046,10.);
#7101=VECTOR('',#23047,10.);
#7102=VECTOR('',#23048,10.);
#7103=VECTOR('',#23049,10.);
#7104=VECTOR('',#23050,10.);
#7105=VECTOR('',#23051,10.);
#7106=VECTOR('',#23052,10.);
#7107=VECTOR('',#23053,10.);
#7108=VECTOR('',#23054,10.);
#7109=VECTOR('',#23055,10.);
#7110=VECTOR('',#23056,10.);
#7111=VECTOR('',#23057,10.);
#7112=VECTOR('',#23058,10.);
#7113=VECTOR('',#23059,10.);
#7114=VECTOR('',#23060,10.);
#7115=VECTOR('',#23061,10.);
#7116=VECTOR('',#23062,10.);
#7117=VECTOR('',#23063,10.);
#7118=VECTOR('',#23064,10.);
#7119=VECTOR('',#23065,10.);
#7120=VECTOR('',#23066,10.);
#7121=VECTOR('',#23067,10.);
#7122=VECTOR('',#23068,10.);
#7123=VECTOR('',#23069,10.);
#7124=VECTOR('',#23070,10.);
#7125=VECTOR('',#23071,10.);
#7126=VECTOR('',#23072,10.);
#7127=VECTOR('',#23073,10.);
#7128=VECTOR('',#23074,10.);
#7129=VECTOR('',#23075,10.);
#7130=VECTOR('',#23076,10.);
#7131=VECTOR('',#23077,10.);
#7132=VECTOR('',#23078,10.);
#7133=VECTOR('',#23079,10.);
#7134=VECTOR('',#23080,10.);
#7135=VECTOR('',#23081,10.);
#7136=VECTOR('',#23082,10.);
#7137=VECTOR('',#23083,10.);
#7138=VECTOR('',#23084,10.);
#7139=VECTOR('',#23085,10.);
#7140=VECTOR('',#23086,10.);
#7141=VECTOR('',#23087,10.);
#7142=VECTOR('',#23088,10.);
#7143=VECTOR('',#23089,10.);
#7144=VECTOR('',#23090,10.);
#7145=VECTOR('',#23091,10.);
#7146=VECTOR('',#23092,10.);
#7147=VECTOR('',#23093,10.);
#7148=VECTOR('',#23094,10.);
#7149=VECTOR('',#23095,10.);
#7150=VECTOR('',#23096,10.);
#7151=VECTOR('',#23097,10.);
#7152=VECTOR('',#23098,10.);
#7153=VECTOR('',#23099,10.);
#7154=VECTOR('',#23100,10.);
#7155=VECTOR('',#23101,10.);
#7156=VECTOR('',#23102,10.);
#7157=VECTOR('',#23103,10.);
#7158=VECTOR('',#23104,10.);
#7159=VECTOR('',#23105,10.);
#7160=VECTOR('',#23106,10.);
#7161=VECTOR('',#23107,10.);
#7162=VECTOR('',#23108,10.);
#7163=VECTOR('',#23109,10.);
#7164=VECTOR('',#23110,10.);
#7165=VECTOR('',#23111,10.);
#7166=VECTOR('',#23112,10.);
#7167=VECTOR('',#23113,10.);
#7168=VECTOR('',#23114,10.);
#7169=VECTOR('',#23115,10.);
#7170=VECTOR('',#23116,10.);
#7171=VECTOR('',#23121,0.650000000000001);
#7172=VECTOR('',#23126,0.55);
#7173=VECTOR('',#23131,0.650000000000001);
#7174=VECTOR('',#23134,10.);
#7175=VECTOR('',#23135,10.);
#7176=VECTOR('',#23138,10.);
#7177=VECTOR('',#23141,10.);
#7178=VECTOR('',#23144,10.);
#7179=VECTOR('',#23147,10.);
#7180=VECTOR('',#23150,10.);
#7181=VECTOR('',#23153,10.);
#7182=VECTOR('',#23156,10.);
#7183=VECTOR('',#23159,10.);
#7184=VECTOR('',#23162,10.);
#7185=VECTOR('',#23165,10.);
#7186=VECTOR('',#23168,10.);
#7187=VECTOR('',#23171,10.);
#7188=VECTOR('',#23174,10.);
#7189=VECTOR('',#23177,10.);
#7190=VECTOR('',#23180,10.);
#7191=VECTOR('',#23183,10.);
#7192=VECTOR('',#23186,10.);
#7193=VECTOR('',#23189,10.);
#7194=VECTOR('',#23192,10.);
#7195=VECTOR('',#23195,10.);
#7196=VECTOR('',#23198,10.);
#7197=VECTOR('',#23201,10.);
#7198=VECTOR('',#23204,10.);
#7199=VECTOR('',#23207,10.);
#7200=VECTOR('',#23210,10.);
#7201=VECTOR('',#23213,10.);
#7202=VECTOR('',#23216,10.);
#7203=VECTOR('',#23219,10.);
#7204=VECTOR('',#23222,10.);
#7205=VECTOR('',#23225,10.);
#7206=VECTOR('',#23228,10.);
#7207=VECTOR('',#23231,10.);
#7208=VECTOR('',#23234,10.);
#7209=VECTOR('',#23237,10.);
#7210=VECTOR('',#23240,10.);
#7211=VECTOR('',#23243,10.);
#7212=VECTOR('',#23246,10.);
#7213=VECTOR('',#23249,10.);
#7214=VECTOR('',#23252,10.);
#7215=VECTOR('',#23255,10.);
#7216=VECTOR('',#23258,10.);
#7217=VECTOR('',#23261,10.);
#7218=VECTOR('',#23264,10.);
#7219=VECTOR('',#23267,10.);
#7220=VECTOR('',#23270,10.);
#7221=VECTOR('',#23273,10.);
#7222=VECTOR('',#23276,10.);
#7223=VECTOR('',#23279,10.);
#7224=VECTOR('',#23282,10.);
#7225=VECTOR('',#23285,10.);
#7226=VECTOR('',#23288,10.);
#7227=VECTOR('',#23291,10.);
#7228=VECTOR('',#23294,10.);
#7229=VECTOR('',#23297,10.);
#7230=VECTOR('',#23300,10.);
#7231=VECTOR('',#23303,10.);
#7232=VECTOR('',#23306,10.);
#7233=VECTOR('',#23309,10.);
#7234=VECTOR('',#23312,10.);
#7235=VECTOR('',#23315,10.);
#7236=VECTOR('',#23318,10.);
#7237=VECTOR('',#23321,10.);
#7238=VECTOR('',#23324,10.);
#7239=VECTOR('',#23327,10.);
#7240=VECTOR('',#23330,10.);
#7241=VECTOR('',#23333,10.);
#7242=VECTOR('',#23336,10.);
#7243=VECTOR('',#23339,10.);
#7244=VECTOR('',#23342,10.);
#7245=VECTOR('',#23345,10.);
#7246=VECTOR('',#23348,10.);
#7247=VECTOR('',#23351,10.);
#7248=VECTOR('',#23354,10.);
#7249=VECTOR('',#23357,10.);
#7250=VECTOR('',#23360,10.);
#7251=VECTOR('',#23363,10.);
#7252=VECTOR('',#23366,10.);
#7253=VECTOR('',#23369,10.);
#7254=VECTOR('',#23372,10.);
#7255=VECTOR('',#23375,10.);
#7256=VECTOR('',#23378,10.);
#7257=VECTOR('',#23381,10.);
#7258=VECTOR('',#23384,10.);
#7259=VECTOR('',#23387,10.);
#7260=VECTOR('',#23390,10.);
#7261=VECTOR('',#23393,10.);
#7262=VECTOR('',#23396,10.);
#7263=VECTOR('',#23399,10.);
#7264=VECTOR('',#23402,10.);
#7265=VECTOR('',#23405,10.);
#7266=VECTOR('',#23408,10.);
#7267=VECTOR('',#23411,10.);
#7268=VECTOR('',#23414,10.);
#7269=VECTOR('',#23417,10.);
#7270=VECTOR('',#23420,10.);
#7271=VECTOR('',#23423,10.);
#7272=VECTOR('',#23426,10.);
#7273=VECTOR('',#23429,10.);
#7274=VECTOR('',#23432,10.);
#7275=VECTOR('',#23435,10.);
#7276=VECTOR('',#23438,10.);
#7277=VECTOR('',#23441,10.);
#7278=VECTOR('',#23444,10.);
#7279=VECTOR('',#23447,10.);
#7280=VECTOR('',#23450,10.);
#7281=VECTOR('',#23453,10.);
#7282=VECTOR('',#23456,10.);
#7283=VECTOR('',#23459,10.);
#7284=VECTOR('',#23462,10.);
#7285=VECTOR('',#23465,10.);
#7286=VECTOR('',#23468,10.);
#7287=VECTOR('',#23471,10.);
#7288=VECTOR('',#23474,10.);
#7289=VECTOR('',#23477,10.);
#7290=VECTOR('',#23480,10.);
#7291=VECTOR('',#23483,10.);
#7292=VECTOR('',#23486,10.);
#7293=VECTOR('',#23489,10.);
#7294=VECTOR('',#23492,10.);
#7295=VECTOR('',#23495,10.);
#7296=VECTOR('',#23498,10.);
#7297=VECTOR('',#23501,10.);
#7298=VECTOR('',#23504,10.);
#7299=VECTOR('',#23507,10.);
#7300=VECTOR('',#23510,10.);
#7301=VECTOR('',#23513,10.);
#7302=VECTOR('',#23516,10.);
#7303=VECTOR('',#23519,10.);
#7304=VECTOR('',#23522,10.);
#7305=VECTOR('',#23525,10.);
#7306=VECTOR('',#23528,10.);
#7307=VECTOR('',#23531,10.);
#7308=VECTOR('',#23534,10.);
#7309=VECTOR('',#23537,10.);
#7310=VECTOR('',#23540,10.);
#7311=VECTOR('',#23543,10.);
#7312=VECTOR('',#23546,10.);
#7313=VECTOR('',#23549,10.);
#7314=VECTOR('',#23552,10.);
#7315=VECTOR('',#23555,10.);
#7316=VECTOR('',#23558,10.);
#7317=VECTOR('',#23561,10.);
#7318=VECTOR('',#23564,10.);
#7319=VECTOR('',#23567,10.);
#7320=VECTOR('',#23570,10.);
#7321=VECTOR('',#23573,10.);
#7322=VECTOR('',#23576,10.);
#7323=VECTOR('',#23579,10.);
#7324=VERTEX_POINT('',#23613);
#7325=VERTEX_POINT('',#23614);
#7326=VERTEX_POINT('',#23616);
#7327=VERTEX_POINT('',#23627);
#7328=VERTEX_POINT('',#23637);
#7329=VERTEX_POINT('',#23638);
#7330=VERTEX_POINT('',#23685);
#7331=VERTEX_POINT('',#23686);
#7332=VERTEX_POINT('',#23733);
#7333=VERTEX_POINT('',#23734);
#7334=VERTEX_POINT('',#23787);
#7335=VERTEX_POINT('',#23788);
#7336=VERTEX_POINT('',#23835);
#7337=VERTEX_POINT('',#23836);
#7338=VERTEX_POINT('',#23883);
#7339=VERTEX_POINT('',#23884);
#7340=VERTEX_POINT('',#23937);
#7341=VERTEX_POINT('',#23938);
#7342=VERTEX_POINT('',#23985);
#7343=VERTEX_POINT('',#23986);
#7344=VERTEX_POINT('',#24033);
#7345=VERTEX_POINT('',#24034);
#7346=VERTEX_POINT('',#24087);
#7347=VERTEX_POINT('',#24088);
#7348=VERTEX_POINT('',#24135);
#7349=VERTEX_POINT('',#24136);
#7350=VERTEX_POINT('',#24183);
#7351=VERTEX_POINT('',#24184);
#7352=VERTEX_POINT('',#24237);
#7353=VERTEX_POINT('',#24238);
#7354=VERTEX_POINT('',#24285);
#7355=VERTEX_POINT('',#24286);
#7356=VERTEX_POINT('',#24333);
#7357=VERTEX_POINT('',#24334);
#7358=VERTEX_POINT('',#24656);
#7359=VERTEX_POINT('',#24657);
#7360=VERTEX_POINT('',#24669);
#7361=VERTEX_POINT('',#24683);
#7362=VERTEX_POINT('',#24690);
#7363=VERTEX_POINT('',#24695);
#7364=VERTEX_POINT('',#24703);
#7365=VERTEX_POINT('',#24771);
#7366=VERTEX_POINT('',#24773);
#7367=VERTEX_POINT('',#24778);
#7368=VERTEX_POINT('',#24785);
#7369=VERTEX_POINT('',#24790);
#7370=VERTEX_POINT('',#24792);
#7371=VERTEX_POINT('',#24866);
#7372=VERTEX_POINT('',#24873);
#7373=VERTEX_POINT('',#24941);
#7374=VERTEX_POINT('',#24943);
#7375=VERTEX_POINT('',#24948);
#7376=VERTEX_POINT('',#24953);
#7377=VERTEX_POINT('',#24958);
#7378=VERTEX_POINT('',#24960);
#7379=VERTEX_POINT('',#25034);
#7380=VERTEX_POINT('',#25041);
#7381=VERTEX_POINT('',#25109);
#7382=VERTEX_POINT('',#25111);
#7383=VERTEX_POINT('',#25116);
#7384=VERTEX_POINT('',#25123);
#7385=VERTEX_POINT('',#25128);
#7386=VERTEX_POINT('',#25130);
#7387=VERTEX_POINT('',#25204);
#7388=VERTEX_POINT('',#25211);
#7389=VERTEX_POINT('',#25279);
#7390=VERTEX_POINT('',#25281);
#7391=VERTEX_POINT('',#25286);
#7392=VERTEX_POINT('',#25293);
#7393=VERTEX_POINT('',#25298);
#7394=VERTEX_POINT('',#25300);
#7395=VERTEX_POINT('',#25374);
#7396=VERTEX_POINT('',#25381);
#7397=VERTEX_POINT('',#25449);
#7398=VERTEX_POINT('',#25451);
#7399=VERTEX_POINT('',#25456);
#7400=VERTEX_POINT('',#25461);
#7401=VERTEX_POINT('',#25466);
#7402=VERTEX_POINT('',#25468);
#7403=VERTEX_POINT('',#25542);
#7404=VERTEX_POINT('',#25549);
#7405=VERTEX_POINT('',#25617);
#7406=VERTEX_POINT('',#25619);
#7407=VERTEX_POINT('',#25624);
#7408=VERTEX_POINT('',#25631);
#7409=VERTEX_POINT('',#25636);
#7410=VERTEX_POINT('',#25638);
#7411=VERTEX_POINT('',#25712);
#7412=VERTEX_POINT('',#25719);
#7413=VERTEX_POINT('',#25787);
#7414=VERTEX_POINT('',#25789);
#7415=VERTEX_POINT('',#25794);
#7416=VERTEX_POINT('',#25801);
#7417=VERTEX_POINT('',#25806);
#7418=VERTEX_POINT('',#25808);
#7419=VERTEX_POINT('',#25882);
#7420=VERTEX_POINT('',#25889);
#7421=VERTEX_POINT('',#25957);
#7422=VERTEX_POINT('',#25959);
#7423=VERTEX_POINT('',#25964);
#7424=VERTEX_POINT('',#25969);
#7425=VERTEX_POINT('',#25974);
#7426=VERTEX_POINT('',#25976);
#7427=VERTEX_POINT('',#26050);
#7428=VERTEX_POINT('',#26057);
#7429=VERTEX_POINT('',#26125);
#7430=VERTEX_POINT('',#26127);
#7431=VERTEX_POINT('',#26132);
#7432=VERTEX_POINT('',#26139);
#7433=VERTEX_POINT('',#26144);
#7434=VERTEX_POINT('',#26146);
#7435=VERTEX_POINT('',#26220);
#7436=VERTEX_POINT('',#26227);
#7437=VERTEX_POINT('',#26295);
#7438=VERTEX_POINT('',#26297);
#7439=VERTEX_POINT('',#26302);
#7440=VERTEX_POINT('',#26309);
#7441=VERTEX_POINT('',#26314);
#7442=VERTEX_POINT('',#26316);
#7443=VERTEX_POINT('',#26390);
#7444=VERTEX_POINT('',#26397);
#7445=VERTEX_POINT('',#26465);
#7446=VERTEX_POINT('',#26467);
#7447=VERTEX_POINT('',#26472);
#7448=VERTEX_POINT('',#26477);
#7449=VERTEX_POINT('',#26482);
#7450=VERTEX_POINT('',#26484);
#7451=VERTEX_POINT('',#26558);
#7452=VERTEX_POINT('',#26591);
#7453=VERTEX_POINT('',#26592);
#7454=VERTEX_POINT('',#26594);
#7455=VERTEX_POINT('',#26601);
#7456=VERTEX_POINT('',#26609);
#7457=VERTEX_POINT('',#26610);
#7458=VERTEX_POINT('',#26634);
#7459=VERTEX_POINT('',#26635);
#7460=VERTEX_POINT('',#26659);
#7461=VERTEX_POINT('',#26660);
#7462=VERTEX_POINT('',#26683);
#7463=VERTEX_POINT('',#26684);
#7464=VERTEX_POINT('',#26708);
#7465=VERTEX_POINT('',#26709);
#7466=VERTEX_POINT('',#26733);
#7467=VERTEX_POINT('',#26734);
#7468=VERTEX_POINT('',#26757);
#7469=VERTEX_POINT('',#26758);
#7470=VERTEX_POINT('',#26782);
#7471=VERTEX_POINT('',#26783);
#7472=VERTEX_POINT('',#26807);
#7473=VERTEX_POINT('',#26808);
#7474=VERTEX_POINT('',#26831);
#7475=VERTEX_POINT('',#26832);
#7476=VERTEX_POINT('',#26856);
#7477=VERTEX_POINT('',#26857);
#7478=VERTEX_POINT('',#26881);
#7479=VERTEX_POINT('',#26882);
#7480=VERTEX_POINT('',#26905);
#7481=VERTEX_POINT('',#26906);
#7482=VERTEX_POINT('',#26930);
#7483=VERTEX_POINT('',#26931);
#7484=VERTEX_POINT('',#26955);
#7485=VERTEX_POINT('',#26956);
#7486=VERTEX_POINT('',#26979);
#7487=VERTEX_POINT('',#26981);
#7488=VERTEX_POINT('',#26983);
#7489=VERTEX_POINT('',#26987);
#7490=VERTEX_POINT('',#26991);
#7491=VERTEX_POINT('',#26994);
#7492=VERTEX_POINT('',#26995);
#7493=VERTEX_POINT('',#26997);
#7494=VERTEX_POINT('',#26999);
#7495=VERTEX_POINT('',#27001);
#7496=VERTEX_POINT('',#27005);
#7497=VERTEX_POINT('',#27007);
#7498=VERTEX_POINT('',#27011);
#7499=VERTEX_POINT('',#27013);
#7500=VERTEX_POINT('',#27017);
#7501=VERTEX_POINT('',#27019);
#7502=VERTEX_POINT('',#27023);
#7503=VERTEX_POINT('',#27024);
#7504=VERTEX_POINT('',#27026);
#7505=VERTEX_POINT('',#27028);
#7506=VERTEX_POINT('',#27030);
#7507=VERTEX_POINT('',#27034);
#7508=VERTEX_POINT('',#27036);
#7509=VERTEX_POINT('',#27040);
#7510=VERTEX_POINT('',#27042);
#7511=VERTEX_POINT('',#27049);
#7512=VERTEX_POINT('',#27050);
#7513=VERTEX_POINT('',#27052);
#7514=VERTEX_POINT('',#27054);
#7515=VERTEX_POINT('',#27056);
#7516=VERTEX_POINT('',#27060);
#7517=VERTEX_POINT('',#27062);
#7518=VERTEX_POINT('',#27066);
#7519=VERTEX_POINT('',#27068);
#7520=VERTEX_POINT('',#27075);
#7521=VERTEX_POINT('',#27076);
#7522=VERTEX_POINT('',#27078);
#7523=VERTEX_POINT('',#27080);
#7524=VERTEX_POINT('',#27082);
#7525=VERTEX_POINT('',#27086);
#7526=VERTEX_POINT('',#27088);
#7527=VERTEX_POINT('',#27092);
#7528=VERTEX_POINT('',#27094);
#7529=VERTEX_POINT('',#27101);
#7530=VERTEX_POINT('',#27102);
#7531=VERTEX_POINT('',#27104);
#7532=VERTEX_POINT('',#27106);
#7533=VERTEX_POINT('',#27108);
#7534=VERTEX_POINT('',#27112);
#7535=VERTEX_POINT('',#27114);
#7536=VERTEX_POINT('',#27118);
#7537=VERTEX_POINT('',#27120);
#7538=VERTEX_POINT('',#27127);
#7539=VERTEX_POINT('',#27128);
#7540=VERTEX_POINT('',#27130);
#7541=VERTEX_POINT('',#27132);
#7542=VERTEX_POINT('',#27134);
#7543=VERTEX_POINT('',#27139);
#7544=VERTEX_POINT('',#27143);
#7545=VERTEX_POINT('',#27147);
#7546=VERTEX_POINT('',#27149);
#7547=VERTEX_POINT('',#27153);
#7548=VERTEX_POINT('',#27154);
#7549=VERTEX_POINT('',#27156);
#7550=VERTEX_POINT('',#27158);
#7551=VERTEX_POINT('',#27160);
#7552=VERTEX_POINT('',#27165);
#7553=VERTEX_POINT('',#27169);
#7554=VERTEX_POINT('',#27173);
#7555=VERTEX_POINT('',#27174);
#7556=VERTEX_POINT('',#27176);
#7557=VERTEX_POINT('',#27178);
#7558=VERTEX_POINT('',#27180);
#7559=VERTEX_POINT('',#27184);
#7560=VERTEX_POINT('',#27186);
#7561=VERTEX_POINT('',#27190);
#7562=VERTEX_POINT('',#27192);
#7563=VERTEX_POINT('',#27196);
#7564=VERTEX_POINT('',#27198);
#7565=VERTEX_POINT('',#27202);
#7566=VERTEX_POINT('',#27203);
#7567=VERTEX_POINT('',#27205);
#7568=VERTEX_POINT('',#27207);
#7569=VERTEX_POINT('',#27209);
#7570=VERTEX_POINT('',#27214);
#7571=VERTEX_POINT('',#27218);
#7572=VERTEX_POINT('',#27222);
#7573=VERTEX_POINT('',#27224);
#7574=VERTEX_POINT('',#27228);
#7575=VERTEX_POINT('',#27229);
#7576=VERTEX_POINT('',#27231);
#7577=VERTEX_POINT('',#27233);
#7578=VERTEX_POINT('',#27235);
#7579=VERTEX_POINT('',#27240);
#7580=VERTEX_POINT('',#27244);
#7581=VERTEX_POINT('',#27248);
#7582=VERTEX_POINT('',#27250);
#7583=VERTEX_POINT('',#27254);
#7584=VERTEX_POINT('',#27255);
#7585=VERTEX_POINT('',#27257);
#7586=VERTEX_POINT('',#27259);
#7587=VERTEX_POINT('',#27261);
#7588=VERTEX_POINT('',#27266);
#7589=VERTEX_POINT('',#27270);
#7590=VERTEX_POINT('',#27274);
#7591=VERTEX_POINT('',#27276);
#7592=VERTEX_POINT('',#27280);
#7593=VERTEX_POINT('',#27281);
#7594=VERTEX_POINT('',#27283);
#7595=VERTEX_POINT('',#27285);
#7596=VERTEX_POINT('',#27287);
#7597=VERTEX_POINT('',#27292);
#7598=VERTEX_POINT('',#27296);
#7599=VERTEX_POINT('',#27303);
#7600=VERTEX_POINT('',#27304);
#7601=VERTEX_POINT('',#27309);
#7602=VERTEX_POINT('',#27311);
#7603=VERTEX_POINT('',#27318);
#7604=VERTEX_POINT('',#27416);
#7605=VERTEX_POINT('',#27692);
#7606=VERTEX_POINT('',#27697);
#7607=VERTEX_POINT('',#27702);
#7608=VERTEX_POINT('',#27753);
#7609=VERTEX_POINT('',#27760);
#7610=VERTEX_POINT('',#27812);
#7611=VERTEX_POINT('',#27813);
#7612=VERTEX_POINT('',#27818);
#7613=VERTEX_POINT('',#27820);
#7614=VERTEX_POINT('',#27827);
#7615=VERTEX_POINT('',#27919);
#7616=VERTEX_POINT('',#28175);
#7617=VERTEX_POINT('',#28180);
#7618=VERTEX_POINT('',#28189);
#7619=VERTEX_POINT('',#28196);
#7620=VERTEX_POINT('',#28248);
#7621=VERTEX_POINT('',#28249);
#7622=VERTEX_POINT('',#28254);
#7623=VERTEX_POINT('',#28256);
#7624=VERTEX_POINT('',#28263);
#7625=VERTEX_POINT('',#28361);
#7626=VERTEX_POINT('',#28647);
#7627=VERTEX_POINT('',#28652);
#7628=VERTEX_POINT('',#28661);
#7629=VERTEX_POINT('',#28668);
#7630=VERTEX_POINT('',#28720);
#7631=VERTEX_POINT('',#28721);
#7632=VERTEX_POINT('',#28726);
#7633=VERTEX_POINT('',#28728);
#7634=VERTEX_POINT('',#28735);
#7635=VERTEX_POINT('',#28833);
#7636=VERTEX_POINT('',#29109);
#7637=VERTEX_POINT('',#29114);
#7638=VERTEX_POINT('',#29123);
#7639=VERTEX_POINT('',#29130);
#7640=VERTEX_POINT('',#29182);
#7641=VERTEX_POINT('',#29183);
#7642=VERTEX_POINT('',#29188);
#7643=VERTEX_POINT('',#29190);
#7644=VERTEX_POINT('',#29197);
#7645=VERTEX_POINT('',#29289);
#7646=VERTEX_POINT('',#29545);
#7647=VERTEX_POINT('',#29550);
#7648=VERTEX_POINT('',#29559);
#7649=VERTEX_POINT('',#29566);
#7650=VERTEX_POINT('',#29618);
#7651=VERTEX_POINT('',#29619);
#7652=VERTEX_POINT('',#29624);
#7653=VERTEX_POINT('',#29626);
#7654=VERTEX_POINT('',#29633);
#7655=VERTEX_POINT('',#29731);
#7656=VERTEX_POINT('',#30017);
#7657=VERTEX_POINT('',#30022);
#7658=VERTEX_POINT('',#30031);
#7659=VERTEX_POINT('',#30038);
#7660=VERTEX_POINT('',#30090);
#7661=VERTEX_POINT('',#30091);
#7662=VERTEX_POINT('',#30096);
#7663=VERTEX_POINT('',#30098);
#7664=VERTEX_POINT('',#30105);
#7665=VERTEX_POINT('',#30203);
#7666=VERTEX_POINT('',#30479);
#7667=VERTEX_POINT('',#30484);
#7668=VERTEX_POINT('',#30493);
#7669=VERTEX_POINT('',#30500);
#7670=VERTEX_POINT('',#30552);
#7671=VERTEX_POINT('',#30553);
#7672=VERTEX_POINT('',#30558);
#7673=VERTEX_POINT('',#30560);
#7674=VERTEX_POINT('',#30567);
#7675=VERTEX_POINT('',#30659);
#7676=VERTEX_POINT('',#30915);
#7677=VERTEX_POINT('',#30920);
#7678=VERTEX_POINT('',#30929);
#7679=VERTEX_POINT('',#30936);
#7680=VERTEX_POINT('',#30988);
#7681=VERTEX_POINT('',#30989);
#7682=VERTEX_POINT('',#30994);
#7683=VERTEX_POINT('',#30996);
#7684=VERTEX_POINT('',#31003);
#7685=VERTEX_POINT('',#31101);
#7686=VERTEX_POINT('',#31387);
#7687=VERTEX_POINT('',#31392);
#7688=VERTEX_POINT('',#31401);
#7689=VERTEX_POINT('',#31408);
#7690=VERTEX_POINT('',#31460);
#7691=VERTEX_POINT('',#31461);
#7692=VERTEX_POINT('',#31466);
#7693=VERTEX_POINT('',#31468);
#7694=VERTEX_POINT('',#31475);
#7695=VERTEX_POINT('',#31573);
#7696=VERTEX_POINT('',#31849);
#7697=VERTEX_POINT('',#31854);
#7698=VERTEX_POINT('',#31863);
#7699=VERTEX_POINT('',#31870);
#7700=VERTEX_POINT('',#31922);
#7701=VERTEX_POINT('',#31923);
#7702=VERTEX_POINT('',#31928);
#7703=VERTEX_POINT('',#31930);
#7704=VERTEX_POINT('',#31937);
#7705=VERTEX_POINT('',#32029);
#7706=VERTEX_POINT('',#32285);
#7707=VERTEX_POINT('',#32290);
#7708=VERTEX_POINT('',#32299);
#7709=VERTEX_POINT('',#32306);
#7710=VERTEX_POINT('',#32358);
#7711=VERTEX_POINT('',#32359);
#7712=VERTEX_POINT('',#32364);
#7713=VERTEX_POINT('',#32366);
#7714=VERTEX_POINT('',#32373);
#7715=VERTEX_POINT('',#32471);
#7716=VERTEX_POINT('',#32757);
#7717=VERTEX_POINT('',#32762);
#7718=VERTEX_POINT('',#32771);
#7719=VERTEX_POINT('',#32778);
#7720=VERTEX_POINT('',#32830);
#7721=VERTEX_POINT('',#32832);
#7722=VERTEX_POINT('',#32836);
#7723=VERTEX_POINT('',#32839);
#7724=VERTEX_POINT('',#32843);
#7725=VERTEX_POINT('',#32845);
#7726=VERTEX_POINT('',#32849);
#7727=VERTEX_POINT('',#32852);
#7728=VERTEX_POINT('',#32856);
#7729=VERTEX_POINT('',#32857);
#7730=VERTEX_POINT('',#32861);
#7731=VERTEX_POINT('',#32863);
#7732=VERTEX_POINT('',#32867);
#7733=VERTEX_POINT('',#32873);
#7734=VERTEX_POINT('',#32878);
#7735=VERTEX_POINT('',#32880);
#7736=VERTEX_POINT('',#32885);
#7737=VERTEX_POINT('',#32891);
#7738=VERTEX_POINT('',#32893);
#7739=VERTEX_POINT('',#32897);
#7740=VERTEX_POINT('',#32905);
#7741=VERTEX_POINT('',#32907);
#7742=VERTEX_POINT('',#32912);
#7743=VERTEX_POINT('',#32916);
#7744=VERTEX_POINT('',#32920);
#7745=VERTEX_POINT('',#32926);
#7746=VERTEX_POINT('',#32928);
#7747=VERTEX_POINT('',#32932);
#7748=VERTEX_POINT('',#32939);
#7749=VERTEX_POINT('',#32940);
#7750=VERTEX_POINT('',#32944);
#7751=VERTEX_POINT('',#32951);
#7752=VERTEX_POINT('',#32953);
#7753=VERTEX_POINT('',#32957);
#7754=VERTEX_POINT('',#32965);
#7755=VERTEX_POINT('',#32967);
#7756=VERTEX_POINT('',#32972);
#7757=VERTEX_POINT('',#32976);
#7758=VERTEX_POINT('',#32980);
#7759=VERTEX_POINT('',#32986);
#7760=VERTEX_POINT('',#32988);
#7761=VERTEX_POINT('',#32992);
#7762=VERTEX_POINT('',#32999);
#7763=VERTEX_POINT('',#33000);
#7764=VERTEX_POINT('',#33004);
#7765=VERTEX_POINT('',#33011);
#7766=VERTEX_POINT('',#33013);
#7767=VERTEX_POINT('',#33017);
#7768=VERTEX_POINT('',#33025);
#7769=VERTEX_POINT('',#33027);
#7770=VERTEX_POINT('',#33032);
#7771=VERTEX_POINT('',#33036);
#7772=VERTEX_POINT('',#33040);
#7773=VERTEX_POINT('',#33046);
#7774=VERTEX_POINT('',#33048);
#7775=VERTEX_POINT('',#33052);
#7776=VERTEX_POINT('',#33059);
#7777=VERTEX_POINT('',#33060);
#7778=VERTEX_POINT('',#33064);
#7779=VERTEX_POINT('',#33071);
#7780=VERTEX_POINT('',#33073);
#7781=VERTEX_POINT('',#33077);
#7782=VERTEX_POINT('',#33085);
#7783=VERTEX_POINT('',#33087);
#7784=VERTEX_POINT('',#33092);
#7785=VERTEX_POINT('',#33096);
#7786=VERTEX_POINT('',#33100);
#7787=VERTEX_POINT('',#33106);
#7788=VERTEX_POINT('',#33108);
#7789=VERTEX_POINT('',#33112);
#7790=VERTEX_POINT('',#33119);
#7791=VERTEX_POINT('',#33120);
#7792=VERTEX_POINT('',#33124);
#7793=VERTEX_POINT('',#33131);
#7794=VERTEX_POINT('',#33133);
#7795=VERTEX_POINT('',#33137);
#7796=VERTEX_POINT('',#33145);
#7797=VERTEX_POINT('',#33147);
#7798=VERTEX_POINT('',#33152);
#7799=VERTEX_POINT('',#33156);
#7800=VERTEX_POINT('',#33160);
#7801=VERTEX_POINT('',#33166);
#7802=VERTEX_POINT('',#33168);
#7803=VERTEX_POINT('',#33172);
#7804=VERTEX_POINT('',#33179);
#7805=VERTEX_POINT('',#33181);
#7806=VERTEX_POINT('',#33183);
#7807=VERTEX_POINT('',#33185);
#7808=VERTEX_POINT('',#33187);
#7809=VERTEX_POINT('',#33189);
#7810=VERTEX_POINT('',#33191);
#7811=VERTEX_POINT('',#33193);
#7812=VERTEX_POINT('',#33195);
#7813=VERTEX_POINT('',#33197);
#7814=VERTEX_POINT('',#33199);
#7815=VERTEX_POINT('',#33201);
#7816=VERTEX_POINT('',#33204);
#7817=VERTEX_POINT('',#33207);
#7818=VERTEX_POINT('',#33211);
#7819=VERTEX_POINT('',#33213);
#7820=VERTEX_POINT('',#33222);
#7821=VERTEX_POINT('',#33224);
#7822=VERTEX_POINT('',#33244);
#7823=VERTEX_POINT('',#33260);
#7824=VERTEX_POINT('',#33264);
#7825=VERTEX_POINT('',#33271);
#7826=VERTEX_POINT('',#33273);
#7827=VERTEX_POINT('',#33278);
#7828=VERTEX_POINT('',#33282);
#7829=VERTEX_POINT('',#33286);
#7830=VERTEX_POINT('',#33292);
#7831=VERTEX_POINT('',#33294);
#7832=VERTEX_POINT('',#33303);
#7833=VERTEX_POINT('',#33307);
#7834=VERTEX_POINT('',#33309);
#7835=VERTEX_POINT('',#33318);
#7836=VERTEX_POINT('',#33320);
#7837=VERTEX_POINT('',#33327);
#7838=VERTEX_POINT('',#33329);
#7839=VERTEX_POINT('',#33334);
#7840=VERTEX_POINT('',#33338);
#7841=VERTEX_POINT('',#33342);
#7842=VERTEX_POINT('',#33348);
#7843=VERTEX_POINT('',#33350);
#7844=VERTEX_POINT('',#33359);
#7845=VERTEX_POINT('',#33363);
#7846=VERTEX_POINT('',#33365);
#7847=VERTEX_POINT('',#33374);
#7848=VERTEX_POINT('',#33376);
#7849=VERTEX_POINT('',#33383);
#7850=VERTEX_POINT('',#33385);
#7851=VERTEX_POINT('',#33390);
#7852=VERTEX_POINT('',#33394);
#7853=VERTEX_POINT('',#33398);
#7854=VERTEX_POINT('',#33404);
#7855=VERTEX_POINT('',#33406);
#7856=VERTEX_POINT('',#33415);
#7857=VERTEX_POINT('',#33419);
#7858=VERTEX_POINT('',#33421);
#7859=VERTEX_POINT('',#33430);
#7860=VERTEX_POINT('',#33432);
#7861=VERTEX_POINT('',#33439);
#7862=VERTEX_POINT('',#33441);
#7863=VERTEX_POINT('',#33446);
#7864=VERTEX_POINT('',#33450);
#7865=VERTEX_POINT('',#33454);
#7866=VERTEX_POINT('',#33460);
#7867=VERTEX_POINT('',#33462);
#7868=VERTEX_POINT('',#33471);
#7869=VERTEX_POINT('',#33475);
#7870=VERTEX_POINT('',#33477);
#7871=VERTEX_POINT('',#33486);
#7872=VERTEX_POINT('',#33488);
#7873=VERTEX_POINT('',#33495);
#7874=VERTEX_POINT('',#33497);
#7875=VERTEX_POINT('',#33502);
#7876=VERTEX_POINT('',#33506);
#7877=VERTEX_POINT('',#33510);
#7878=VERTEX_POINT('',#33516);
#7879=VERTEX_POINT('',#33518);
#7880=VERTEX_POINT('',#33527);
#7881=VERTEX_POINT('',#33531);
#7882=VERTEX_POINT('',#33533);
#7883=VERTEX_POINT('',#33542);
#7884=VERTEX_POINT('',#33544);
#7885=VERTEX_POINT('',#33550);
#7886=VERTEX_POINT('',#33552);
#7887=VERTEX_POINT('',#33555);
#7888=VERTEX_POINT('',#33557);
#7889=VERTEX_POINT('',#33564);
#7890=VERTEX_POINT('',#33574);
#7891=VERTEX_POINT('',#33576);
#7892=VERTEX_POINT('',#33581);
#7893=VERTEX_POINT('',#33585);
#7894=VERTEX_POINT('',#33589);
#7895=VERTEX_POINT('',#33595);
#7896=VERTEX_POINT('',#33601);
#7897=VERTEX_POINT('',#33607);
#7898=VERTEX_POINT('',#33616);
#7899=VERTEX_POINT('',#33623);
#7900=VERTEX_POINT('',#33628);
#7901=VERTEX_POINT('',#33635);
#7902=VERTEX_POINT('',#33730);
#7903=VERTEX_POINT('',#33732);
#7904=VERTEX_POINT('',#34278);
#7905=VERTEX_POINT('',#34383);
#7906=VERTEX_POINT('',#34386);
#7907=VERTEX_POINT('',#35215);
#7908=VERTEX_POINT('',#35490);
#7909=VERTEX_POINT('',#35492);
#7910=VERTEX_POINT('',#35497);
#7911=VERTEX_POINT('',#35500);
#7912=VERTEX_POINT('',#35506);
#7913=VERTEX_POINT('',#36015);
#7914=VERTEX_POINT('',#36534);
#7915=VERTEX_POINT('',#37033);
#7916=VERTEX_POINT('',#37542);
#7917=VERTEX_POINT('',#38061);
#7918=VERTEX_POINT('',#38560);
#7919=VERTEX_POINT('',#39069);
#7920=VERTEX_POINT('',#39588);
#7921=VERTEX_POINT('',#40097);
#7922=VERTEX_POINT('',#40606);
#7923=VERTEX_POINT('',#41125);
#7924=VERTEX_POINT('',#41653);
#7925=VERTEX_POINT('',#41661);
#7926=VERTEX_POINT('',#41665);
#7927=VERTEX_POINT('',#41668);
#7928=VERTEX_POINT('',#41672);
#7929=VERTEX_POINT('',#41676);
#7930=VERTEX_POINT('',#41680);
#7931=VERTEX_POINT('',#41684);
#7932=VERTEX_POINT('',#41687);
#7933=VERTEX_POINT('',#41691);
#7934=VERTEX_POINT('',#41695);
#7935=VERTEX_POINT('',#41699);
#7936=VERTEX_POINT('',#41703);
#7937=VERTEX_POINT('',#41711);
#7938=VERTEX_POINT('',#41784);
#7939=VERTEX_POINT('',#41785);
#7940=VERTEX_POINT('',#41790);
#7941=VERTEX_POINT('',#41808);
#7942=VERTEX_POINT('',#41831);
#7943=VERTEX_POINT('',#41833);
#7944=VERTEX_POINT('',#41838);
#7945=VERTEX_POINT('',#41840);
#7946=VERTEX_POINT('',#41847);
#7947=VERTEX_POINT('',#41849);
#7948=VERTEX_POINT('',#42587);
#7949=VERTEX_POINT('',#42674);
#7950=VERTEX_POINT('',#42840);
#7951=VERTEX_POINT('',#42841);
#7952=VERTEX_POINT('',#43613);
#7953=VERTEX_POINT('',#43700);
#7954=VERTEX_POINT('',#43729);
#7955=VERTEX_POINT('',#43731);
#7956=VERTEX_POINT('',#43735);
#7957=VERTEX_POINT('',#43739);
#7958=VERTEX_POINT('',#43743);
#7959=VERTEX_POINT('',#43746);
#7960=VERTEX_POINT('',#43750);
#7961=VERTEX_POINT('',#43754);
#7962=VERTEX_POINT('',#43760);
#7963=VERTEX_POINT('',#43761);
#7964=VERTEX_POINT('',#43763);
#7965=VERTEX_POINT('',#43765);
#7966=VERTEX_POINT('',#43769);
#7967=VERTEX_POINT('',#43771);
#7968=VERTEX_POINT('',#43774);
#7969=VERTEX_POINT('',#43777);
#7970=VERTEX_POINT('',#43779);
#7971=VERTEX_POINT('',#43783);
#7972=VERTEX_POINT('',#43785);
#7973=VERTEX_POINT('',#43788);
#7974=VERTEX_POINT('',#43790);
#7975=VERTEX_POINT('',#43792);
#7976=VERTEX_POINT('',#43794);
#7977=VERTEX_POINT('',#43795);
#7978=VERTEX_POINT('',#43797);
#7979=VERTEX_POINT('',#43799);
#7980=VERTEX_POINT('',#43801);
#7981=VERTEX_POINT('',#43803);
#7982=VERTEX_POINT('',#43805);
#7983=VERTEX_POINT('',#43807);
#7984=VERTEX_POINT('',#43809);
#7985=VERTEX_POINT('',#43811);
#7986=VERTEX_POINT('',#43813);
#7987=VERTEX_POINT('',#43815);
#7988=VERTEX_POINT('',#43817);
#7989=VERTEX_POINT('',#43819);
#7990=VERTEX_POINT('',#43822);
#7991=VERTEX_POINT('',#43823);
#7992=VERTEX_POINT('',#43825);
#7993=VERTEX_POINT('',#43827);
#7994=VERTEX_POINT('',#43829);
#7995=VERTEX_POINT('',#43831);
#7996=VERTEX_POINT('',#43833);
#7997=VERTEX_POINT('',#43835);
#7998=VERTEX_POINT('',#43837);
#7999=VERTEX_POINT('',#43839);
#8000=VERTEX_POINT('',#43841);
#8001=VERTEX_POINT('',#43843);
#8002=VERTEX_POINT('',#43845);
#8003=VERTEX_POINT('',#43847);
#8004=VERTEX_POINT('',#43850);
#8005=VERTEX_POINT('',#43851);
#8006=VERTEX_POINT('',#43853);
#8007=VERTEX_POINT('',#43855);
#8008=VERTEX_POINT('',#43857);
#8009=VERTEX_POINT('',#43859);
#8010=VERTEX_POINT('',#43861);
#8011=VERTEX_POINT('',#43863);
#8012=VERTEX_POINT('',#43865);
#8013=VERTEX_POINT('',#43867);
#8014=VERTEX_POINT('',#43869);
#8015=VERTEX_POINT('',#43871);
#8016=VERTEX_POINT('',#43873);
#8017=VERTEX_POINT('',#43875);
#8018=VERTEX_POINT('',#43878);
#8019=VERTEX_POINT('',#43879);
#8020=VERTEX_POINT('',#43881);
#8021=VERTEX_POINT('',#43883);
#8022=VERTEX_POINT('',#43885);
#8023=VERTEX_POINT('',#43887);
#8024=VERTEX_POINT('',#43889);
#8025=VERTEX_POINT('',#43891);
#8026=VERTEX_POINT('',#43893);
#8027=VERTEX_POINT('',#43895);
#8028=VERTEX_POINT('',#43897);
#8029=VERTEX_POINT('',#43899);
#8030=VERTEX_POINT('',#43901);
#8031=VERTEX_POINT('',#43903);
#8032=VERTEX_POINT('',#43906);
#8033=VERTEX_POINT('',#43907);
#8034=VERTEX_POINT('',#43909);
#8035=VERTEX_POINT('',#43911);
#8036=VERTEX_POINT('',#43913);
#8037=VERTEX_POINT('',#43915);
#8038=VERTEX_POINT('',#43917);
#8039=VERTEX_POINT('',#43919);
#8040=VERTEX_POINT('',#43921);
#8041=VERTEX_POINT('',#43923);
#8042=VERTEX_POINT('',#43925);
#8043=VERTEX_POINT('',#43927);
#8044=VERTEX_POINT('',#43929);
#8045=VERTEX_POINT('',#43931);
#8046=VERTEX_POINT('',#43934);
#8047=VERTEX_POINT('',#43935);
#8048=VERTEX_POINT('',#43937);
#8049=VERTEX_POINT('',#43939);
#8050=VERTEX_POINT('',#43941);
#8051=VERTEX_POINT('',#43943);
#8052=VERTEX_POINT('',#43945);
#8053=VERTEX_POINT('',#43947);
#8054=VERTEX_POINT('',#43949);
#8055=VERTEX_POINT('',#43951);
#8056=VERTEX_POINT('',#43953);
#8057=VERTEX_POINT('',#43955);
#8058=VERTEX_POINT('',#43957);
#8059=VERTEX_POINT('',#43959);
#8060=VERTEX_POINT('',#43962);
#8061=VERTEX_POINT('',#43965);
#8062=VERTEX_POINT('',#43969);
#8063=VERTEX_POINT('',#43974);
#8064=VERTEX_POINT('',#43976);
#8065=VERTEX_POINT('',#43985);
#8066=VERTEX_POINT('',#43987);
#8067=VERTEX_POINT('',#43994);
#8068=VERTEX_POINT('',#43996);
#8069=VERTEX_POINT('',#44000);
#8070=VERTEX_POINT('',#44002);
#8071=VERTEX_POINT('',#44017);
#8072=VERTEX_POINT('',#44019);
#8073=VERTEX_POINT('',#44021);
#8074=VERTEX_POINT('',#44023);
#8075=VERTEX_POINT('',#44024);
#8076=VERTEX_POINT('',#44026);
#8077=VERTEX_POINT('',#44028);
#8078=VERTEX_POINT('',#44030);
#8079=VERTEX_POINT('',#44032);
#8080=VERTEX_POINT('',#44034);
#8081=VERTEX_POINT('',#44036);
#8082=VERTEX_POINT('',#44038);
#8083=VERTEX_POINT('',#44040);
#8084=VERTEX_POINT('',#44042);
#8085=VERTEX_POINT('',#44044);
#8086=VERTEX_POINT('',#44046);
#8087=VERTEX_POINT('',#44048);
#8088=VERTEX_POINT('',#44051);
#8089=VERTEX_POINT('',#44052);
#8090=VERTEX_POINT('',#44054);
#8091=VERTEX_POINT('',#44056);
#8092=VERTEX_POINT('',#44058);
#8093=VERTEX_POINT('',#44060);
#8094=VERTEX_POINT('',#44062);
#8095=VERTEX_POINT('',#44064);
#8096=VERTEX_POINT('',#44066);
#8097=VERTEX_POINT('',#44068);
#8098=VERTEX_POINT('',#44070);
#8099=VERTEX_POINT('',#44072);
#8100=VERTEX_POINT('',#44074);
#8101=VERTEX_POINT('',#44076);
#8102=VERTEX_POINT('',#44079);
#8103=VERTEX_POINT('',#44080);
#8104=VERTEX_POINT('',#44082);
#8105=VERTEX_POINT('',#44084);
#8106=VERTEX_POINT('',#44086);
#8107=VERTEX_POINT('',#44088);
#8108=VERTEX_POINT('',#44090);
#8109=VERTEX_POINT('',#44092);
#8110=VERTEX_POINT('',#44094);
#8111=VERTEX_POINT('',#44096);
#8112=VERTEX_POINT('',#44098);
#8113=VERTEX_POINT('',#44100);
#8114=VERTEX_POINT('',#44102);
#8115=VERTEX_POINT('',#44104);
#8116=VERTEX_POINT('',#44107);
#8117=VERTEX_POINT('',#44108);
#8118=VERTEX_POINT('',#44110);
#8119=VERTEX_POINT('',#44112);
#8120=VERTEX_POINT('',#44114);
#8121=VERTEX_POINT('',#44116);
#8122=VERTEX_POINT('',#44118);
#8123=VERTEX_POINT('',#44120);
#8124=VERTEX_POINT('',#44122);
#8125=VERTEX_POINT('',#44124);
#8126=VERTEX_POINT('',#44126);
#8127=VERTEX_POINT('',#44128);
#8128=VERTEX_POINT('',#44130);
#8129=VERTEX_POINT('',#44132);
#8130=VERTEX_POINT('',#44135);
#8131=VERTEX_POINT('',#44136);
#8132=VERTEX_POINT('',#44138);
#8133=VERTEX_POINT('',#44140);
#8134=VERTEX_POINT('',#44142);
#8135=VERTEX_POINT('',#44144);
#8136=VERTEX_POINT('',#44146);
#8137=VERTEX_POINT('',#44148);
#8138=VERTEX_POINT('',#44150);
#8139=VERTEX_POINT('',#44152);
#8140=VERTEX_POINT('',#44154);
#8141=VERTEX_POINT('',#44156);
#8142=VERTEX_POINT('',#44158);
#8143=VERTEX_POINT('',#44160);
#8144=VERTEX_POINT('',#44163);
#8145=VERTEX_POINT('',#44164);
#8146=VERTEX_POINT('',#44166);
#8147=VERTEX_POINT('',#44168);
#8148=VERTEX_POINT('',#44170);
#8149=VERTEX_POINT('',#44172);
#8150=VERTEX_POINT('',#44174);
#8151=VERTEX_POINT('',#44176);
#8152=VERTEX_POINT('',#44178);
#8153=VERTEX_POINT('',#44180);
#8154=VERTEX_POINT('',#44182);
#8155=VERTEX_POINT('',#44184);
#8156=VERTEX_POINT('',#44186);
#8157=VERTEX_POINT('',#44188);
#8158=VERTEX_POINT('',#44191);
#8159=VERTEX_POINT('',#44195);
#8160=VERTEX_POINT('',#44199);
#8161=VERTEX_POINT('',#44205);
#8162=VERTEX_POINT('',#44209);
#8163=VERTEX_POINT('',#44215);
#8164=VERTEX_POINT('',#44219);
#8165=VERTEX_POINT('',#44225);
#8166=VERTEX_POINT('',#44229);
#8167=VERTEX_POINT('',#44231);
#8168=VERTEX_POINT('',#44242);
#8169=VERTEX_POINT('',#44272);
#8170=VERTEX_POINT('',#44274);
#8171=VERTEX_POINT('',#44278);
#8172=VERTEX_POINT('',#44282);
#8173=VERTEX_POINT('',#44286);
#8174=VERTEX_POINT('',#44290);
#8175=VERTEX_POINT('',#44294);
#8176=VERTEX_POINT('',#44298);
#8177=VERTEX_POINT('',#44302);
#8178=VERTEX_POINT('',#44306);
#8179=VERTEX_POINT('',#44310);
#8180=VERTEX_POINT('',#44314);
#8181=VERTEX_POINT('',#44318);
#8182=VERTEX_POINT('',#44322);
#8183=VERTEX_POINT('',#44329);
#8184=VERTEX_POINT('',#44331);
#8185=VERTEX_POINT('',#44335);
#8186=VERTEX_POINT('',#44339);
#8187=VERTEX_POINT('',#44343);
#8188=VERTEX_POINT('',#44347);
#8189=VERTEX_POINT('',#44351);
#8190=VERTEX_POINT('',#44355);
#8191=VERTEX_POINT('',#44359);
#8192=VERTEX_POINT('',#44363);
#8193=VERTEX_POINT('',#44367);
#8194=VERTEX_POINT('',#44371);
#8195=VERTEX_POINT('',#44375);
#8196=VERTEX_POINT('',#44379);
#8197=VERTEX_POINT('',#44386);
#8198=VERTEX_POINT('',#44388);
#8199=VERTEX_POINT('',#44392);
#8200=VERTEX_POINT('',#44396);
#8201=VERTEX_POINT('',#44400);
#8202=VERTEX_POINT('',#44404);
#8203=VERTEX_POINT('',#44408);
#8204=VERTEX_POINT('',#44412);
#8205=VERTEX_POINT('',#44416);
#8206=VERTEX_POINT('',#44420);
#8207=VERTEX_POINT('',#44424);
#8208=VERTEX_POINT('',#44428);
#8209=VERTEX_POINT('',#44432);
#8210=VERTEX_POINT('',#44436);
#8211=VERTEX_POINT('',#44443);
#8212=VERTEX_POINT('',#44445);
#8213=VERTEX_POINT('',#44449);
#8214=VERTEX_POINT('',#44453);
#8215=VERTEX_POINT('',#44457);
#8216=VERTEX_POINT('',#44461);
#8217=VERTEX_POINT('',#44465);
#8218=VERTEX_POINT('',#44469);
#8219=VERTEX_POINT('',#44473);
#8220=VERTEX_POINT('',#44477);
#8221=VERTEX_POINT('',#44481);
#8222=VERTEX_POINT('',#44485);
#8223=VERTEX_POINT('',#44489);
#8224=VERTEX_POINT('',#44493);
#8225=VERTEX_POINT('',#44500);
#8226=VERTEX_POINT('',#44502);
#8227=VERTEX_POINT('',#44506);
#8228=VERTEX_POINT('',#44510);
#8229=VERTEX_POINT('',#44514);
#8230=VERTEX_POINT('',#44518);
#8231=VERTEX_POINT('',#44522);
#8232=VERTEX_POINT('',#44526);
#8233=VERTEX_POINT('',#44530);
#8234=VERTEX_POINT('',#44534);
#8235=VERTEX_POINT('',#44538);
#8236=VERTEX_POINT('',#44542);
#8237=VERTEX_POINT('',#44546);
#8238=VERTEX_POINT('',#44550);
#8239=VERTEX_POINT('',#44557);
#8240=VERTEX_POINT('',#44559);
#8241=VERTEX_POINT('',#44563);
#8242=VERTEX_POINT('',#44567);
#8243=VERTEX_POINT('',#44571);
#8244=VERTEX_POINT('',#44575);
#8245=VERTEX_POINT('',#44579);
#8246=VERTEX_POINT('',#44583);
#8247=VERTEX_POINT('',#44587);
#8248=VERTEX_POINT('',#44591);
#8249=VERTEX_POINT('',#44595);
#8250=VERTEX_POINT('',#44599);
#8251=VERTEX_POINT('',#44603);
#8252=VERTEX_POINT('',#44607);
#8253=VERTEX_POINT('',#44614);
#8254=VERTEX_POINT('',#44616);
#8255=VERTEX_POINT('',#44620);
#8256=VERTEX_POINT('',#44624);
#8257=VERTEX_POINT('',#44628);
#8258=VERTEX_POINT('',#44632);
#8259=VERTEX_POINT('',#44636);
#8260=VERTEX_POINT('',#44640);
#8261=VERTEX_POINT('',#44644);
#8262=VERTEX_POINT('',#44648);
#8263=VERTEX_POINT('',#44652);
#8264=VERTEX_POINT('',#44656);
#8265=VERTEX_POINT('',#44660);
#8266=VERTEX_POINT('',#44664);
#8267=VERTEX_POINT('',#44671);
#8268=VERTEX_POINT('',#44673);
#8269=VERTEX_POINT('',#44677);
#8270=VERTEX_POINT('',#44681);
#8271=VERTEX_POINT('',#44685);
#8272=VERTEX_POINT('',#44689);
#8273=VERTEX_POINT('',#44693);
#8274=VERTEX_POINT('',#44697);
#8275=VERTEX_POINT('',#44701);
#8276=VERTEX_POINT('',#44705);
#8277=VERTEX_POINT('',#44709);
#8278=VERTEX_POINT('',#44713);
#8279=VERTEX_POINT('',#44717);
#8280=VERTEX_POINT('',#44721);
#8281=VERTEX_POINT('',#44728);
#8282=VERTEX_POINT('',#44730);
#8283=VERTEX_POINT('',#44734);
#8284=VERTEX_POINT('',#44738);
#8285=VERTEX_POINT('',#44742);
#8286=VERTEX_POINT('',#44746);
#8287=VERTEX_POINT('',#44750);
#8288=VERTEX_POINT('',#44754);
#8289=VERTEX_POINT('',#44758);
#8290=VERTEX_POINT('',#44762);
#8291=VERTEX_POINT('',#44766);
#8292=VERTEX_POINT('',#44770);
#8293=VERTEX_POINT('',#44774);
#8294=VERTEX_POINT('',#44778);
#8295=VERTEX_POINT('',#44785);
#8296=VERTEX_POINT('',#44787);
#8297=VERTEX_POINT('',#44791);
#8298=VERTEX_POINT('',#44795);
#8299=VERTEX_POINT('',#44799);
#8300=VERTEX_POINT('',#44803);
#8301=VERTEX_POINT('',#44807);
#8302=VERTEX_POINT('',#44811);
#8303=VERTEX_POINT('',#44815);
#8304=VERTEX_POINT('',#44819);
#8305=VERTEX_POINT('',#44823);
#8306=VERTEX_POINT('',#44827);
#8307=VERTEX_POINT('',#44831);
#8308=VERTEX_POINT('',#44835);
#8309=VERTEX_POINT('',#44842);
#8310=VERTEX_POINT('',#44844);
#8311=VERTEX_POINT('',#44848);
#8312=VERTEX_POINT('',#44852);
#8313=VERTEX_POINT('',#44856);
#8314=VERTEX_POINT('',#44860);
#8315=VERTEX_POINT('',#44864);
#8316=VERTEX_POINT('',#44868);
#8317=VERTEX_POINT('',#44872);
#8318=VERTEX_POINT('',#44876);
#8319=VERTEX_POINT('',#44880);
#8320=VERTEX_POINT('',#44884);
#8321=VERTEX_POINT('',#44888);
#8322=VERTEX_POINT('',#44892);
#8323=VERTEX_POINT('',#44899);
#8324=VERTEX_POINT('',#44901);
#8325=VERTEX_POINT('',#44905);
#8326=VERTEX_POINT('',#44909);
#8327=VERTEX_POINT('',#44913);
#8328=VERTEX_POINT('',#44917);
#8329=VERTEX_POINT('',#44921);
#8330=VERTEX_POINT('',#44925);
#8331=VERTEX_POINT('',#44929);
#8332=VERTEX_POINT('',#44933);
#8333=VERTEX_POINT('',#44937);
#8334=VERTEX_POINT('',#44941);
#8335=VERTEX_POINT('',#44945);
#8336=VERTEX_POINT('',#44949);
#8337=VERTEX_POINT('',#44961);
#8338=VERTEX_POINT('',#44963);
#8339=VERTEX_POINT('',#44968);
#8340=VERTEX_POINT('',#44970);
#8341=VERTEX_POINT('',#44975);
#8342=VERTEX_POINT('',#44977);
#8343=VERTEX_POINT('',#44982);
#8344=VERTEX_POINT('',#44984);
#8345=VERTEX_POINT('',#44989);
#8346=VERTEX_POINT('',#44991);
#8347=VERTEX_POINT('',#44996);
#8348=VERTEX_POINT('',#44998);
#8349=VERTEX_POINT('',#45003);
#8350=VERTEX_POINT('',#45005);
#8351=VERTEX_POINT('',#45009);
#8352=VERTEX_POINT('',#45012);
#8353=VERTEX_POINT('',#45015);
#8354=VERTEX_POINT('',#45019);
#8355=VERTEX_POINT('',#45021);
#8356=VERTEX_POINT('',#45025);
#8357=VERTEX_POINT('',#45029);
#8358=VERTEX_POINT('',#45032);
#8359=VERTEX_POINT('',#45036);
#8360=VERTEX_POINT('',#45040);
#8361=VERTEX_POINT('',#45044);
#8362=VERTEX_POINT('',#45047);
#8363=VERTEX_POINT('',#45053);
#8364=VERTEX_POINT('',#45057);
#8365=VERTEX_POINT('',#45060);
#8366=VERTEX_POINT('',#45064);
#8367=VERTEX_POINT('',#45068);
#8368=VERTEX_POINT('',#45129);
#8369=VERTEX_POINT('',#45130);
#8370=VERTEX_POINT('',#45135);
#8371=VERTEX_POINT('',#45150);
#8372=VERTEX_POINT('',#45170);
#8373=VERTEX_POINT('',#45172);
#8374=VERTEX_POINT('',#45177);
#8375=VERTEX_POINT('',#45179);
#8376=VERTEX_POINT('',#45186);
#8377=VERTEX_POINT('',#45188);
#8378=VERTEX_POINT('',#45926);
#8379=VERTEX_POINT('',#45998);
#8380=VERTEX_POINT('',#46121);
#8381=VERTEX_POINT('',#46122);
#8382=VERTEX_POINT('',#46909);
#8383=VERTEX_POINT('',#47031);
#8384=VERTEX_POINT('',#47336);
#8385=VERTEX_POINT('',#47337);
#8386=VERTEX_POINT('',#47355);
#8387=VERTEX_POINT('',#47375);
#8388=VERTEX_POINT('',#47377);
#8389=VERTEX_POINT('',#47392);
#8390=VERTEX_POINT('',#47397);
#8391=VERTEX_POINT('',#47426);
#8392=VERTEX_POINT('',#47481);
#8393=VERTEX_POINT('',#47482);
#8394=VERTEX_POINT('',#47487);
#8395=VERTEX_POINT('',#47489);
#8396=VERTEX_POINT('',#47496);
#8397=VERTEX_POINT('',#47501);
#8398=VERTEX_POINT('',#47506);
#8399=VERTEX_POINT('',#47513);
#8400=VERTEX_POINT('',#47515);
#8401=VERTEX_POINT('',#47522);
#8402=VERTEX_POINT('',#47527);
#8403=VERTEX_POINT('',#47529);
#8404=VERTEX_POINT('',#47534);
#8405=VERTEX_POINT('',#47541);
#8406=VERTEX_POINT('',#47543);
#8407=VERTEX_POINT('',#47550);
#8408=VERTEX_POINT('',#47555);
#8409=VERTEX_POINT('',#47557);
#8410=VERTEX_POINT('',#47562);
#8411=VERTEX_POINT('',#47569);
#8412=VERTEX_POINT('',#47571);
#8413=VERTEX_POINT('',#47578);
#8414=VERTEX_POINT('',#47583);
#8415=VERTEX_POINT('',#47585);
#8416=VERTEX_POINT('',#47590);
#8417=VERTEX_POINT('',#47597);
#8418=VERTEX_POINT('',#47599);
#8419=VERTEX_POINT('',#47606);
#8420=VERTEX_POINT('',#47611);
#8421=VERTEX_POINT('',#47613);
#8422=VERTEX_POINT('',#47618);
#8423=VERTEX_POINT('',#47625);
#8424=VERTEX_POINT('',#47627);
#8425=VERTEX_POINT('',#47634);
#8426=VERTEX_POINT('',#47639);
#8427=VERTEX_POINT('',#47641);
#8428=VERTEX_POINT('',#47646);
#8429=VERTEX_POINT('',#47653);
#8430=VERTEX_POINT('',#47655);
#8431=VERTEX_POINT('',#47662);
#8432=VERTEX_POINT('',#47667);
#8433=VERTEX_POINT('',#47669);
#8434=VERTEX_POINT('',#47674);
#8435=VERTEX_POINT('',#47681);
#8436=VERTEX_POINT('',#47683);
#8437=VERTEX_POINT('',#47686);
#8438=VERTEX_POINT('',#47688);
#8439=VERTEX_POINT('',#47695);
#8440=VERTEX_POINT('',#47700);
#8441=VERTEX_POINT('',#47702);
#8442=VERTEX_POINT('',#47707);
#8443=VERTEX_POINT('',#47714);
#8444=VERTEX_POINT('',#47716);
#8445=VERTEX_POINT('',#47723);
#8446=VERTEX_POINT('',#47728);
#8447=VERTEX_POINT('',#47730);
#8448=VERTEX_POINT('',#47735);
#8449=VERTEX_POINT('',#47742);
#8450=VERTEX_POINT('',#47744);
#8451=VERTEX_POINT('',#47751);
#8452=VERTEX_POINT('',#47756);
#8453=VERTEX_POINT('',#47758);
#8454=VERTEX_POINT('',#47763);
#8455=VERTEX_POINT('',#47770);
#8456=VERTEX_POINT('',#47772);
#8457=VERTEX_POINT('',#47779);
#8458=VERTEX_POINT('',#47784);
#8459=VERTEX_POINT('',#47786);
#8460=VERTEX_POINT('',#47791);
#8461=VERTEX_POINT('',#47798);
#8462=VERTEX_POINT('',#47800);
#8463=VERTEX_POINT('',#47807);
#8464=VERTEX_POINT('',#47812);
#8465=VERTEX_POINT('',#47814);
#8466=VERTEX_POINT('',#47819);
#8467=VERTEX_POINT('',#47826);
#8468=VERTEX_POINT('',#47828);
#8469=VERTEX_POINT('',#47835);
#8470=VERTEX_POINT('',#47840);
#8471=VERTEX_POINT('',#47842);
#8472=VERTEX_POINT('',#47847);
#8473=VERTEX_POINT('',#47854);
#8474=VERTEX_POINT('',#47856);
#8475=VERTEX_POINT('',#47863);
#8476=VERTEX_POINT('',#47868);
#8477=VERTEX_POINT('',#47870);
#8478=VERTEX_POINT('',#47875);
#8479=VERTEX_POINT('',#47882);
#8480=VERTEX_POINT('',#47891);
#8481=VERTEX_POINT('',#47896);
#8482=VERTEX_POINT('',#47903);
#8483=VERTEX_POINT('',#47908);
#8484=VERTEX_POINT('',#47915);
#8485=VERTEX_POINT('',#47920);
#8486=VERTEX_POINT('',#47927);
#8487=VERTEX_POINT('',#47932);
#8488=VERTEX_POINT('',#47939);
#8489=VERTEX_POINT('',#47944);
#8490=VERTEX_POINT('',#47951);
#8491=VERTEX_POINT('',#47956);
#8492=VERTEX_POINT('',#47963);
#8493=VERTEX_POINT('',#47968);
#8494=VERTEX_POINT('',#47975);
#8495=VERTEX_POINT('',#47980);
#8496=VERTEX_POINT('',#47987);
#8497=VERTEX_POINT('',#47992);
#8498=VERTEX_POINT('',#47999);
#8499=VERTEX_POINT('',#48004);
#8500=VERTEX_POINT('',#48011);
#8501=VERTEX_POINT('',#48016);
#8502=VERTEX_POINT('',#48023);
#8503=VERTEX_POINT('',#48028);
#8504=VERTEX_POINT('',#48035);
#8505=VERTEX_POINT('',#48040);
#8506=VERTEX_POINT('',#48047);
#8507=VERTEX_POINT('',#48049);
#8508=VERTEX_POINT('',#48051);
#8509=VERTEX_POINT('',#48055);
#8510=VERTEX_POINT('',#48056);
#8511=VERTEX_POINT('',#48061);
#8512=VERTEX_POINT('',#48064);
#8513=VERTEX_POINT('',#48068);
#8514=VERTEX_POINT('',#48178);
#8515=VERTEX_POINT('',#48183);
#8516=VERTEX_POINT('',#48212);
#8517=VERTEX_POINT('',#48246);
#8518=VERTEX_POINT('',#48251);
#8519=VERTEX_POINT('',#48514);
#8520=VERTEX_POINT('',#48534);
#8521=VERTEX_POINT('',#48648);
#8522=VERTEX_POINT('',#48653);
#8523=VERTEX_POINT('',#48682);
#8524=VERTEX_POINT('',#48716);
#8525=VERTEX_POINT('',#48721);
#8526=VERTEX_POINT('',#48984);
#8527=VERTEX_POINT('',#49004);
#8528=VERTEX_POINT('',#49118);
#8529=VERTEX_POINT('',#49123);
#8530=VERTEX_POINT('',#49152);
#8531=VERTEX_POINT('',#49186);
#8532=VERTEX_POINT('',#49191);
#8533=VERTEX_POINT('',#49454);
#8534=VERTEX_POINT('',#49474);
#8535=VERTEX_POINT('',#49588);
#8536=VERTEX_POINT('',#49593);
#8537=VERTEX_POINT('',#49622);
#8538=VERTEX_POINT('',#49656);
#8539=VERTEX_POINT('',#49663);
#8540=VERTEX_POINT('',#49926);
#8541=VERTEX_POINT('',#49946);
#8542=VERTEX_POINT('',#50060);
#8543=VERTEX_POINT('',#50065);
#8544=VERTEX_POINT('',#50094);
#8545=VERTEX_POINT('',#50128);
#8546=VERTEX_POINT('',#50135);
#8547=VERTEX_POINT('',#50398);
#8548=VERTEX_POINT('',#50418);
#8549=VERTEX_POINT('',#50532);
#8550=VERTEX_POINT('',#50537);
#8551=VERTEX_POINT('',#50566);
#8552=VERTEX_POINT('',#50600);
#8553=VERTEX_POINT('',#50605);
#8554=VERTEX_POINT('',#50868);
#8555=VERTEX_POINT('',#50888);
#8556=VERTEX_POINT('',#51006);
#8557=VERTEX_POINT('',#51040);
#8558=VERTEX_POINT('',#51487);
#8559=VERTEX_POINT('',#51534);
#8560=VERTEX_POINT('',#51541);
#8561=VERTEX_POINT('',#51561);
#8562=VERTEX_POINT('',#51568);
#8563=VERTEX_POINT('',#52075);
#8564=VERTEX_POINT('',#52309);
#8565=VERTEX_POINT('',#52356);
#8566=VERTEX_POINT('',#52363);
#8567=VERTEX_POINT('',#52383);
#8568=VERTEX_POINT('',#52390);
#8569=VERTEX_POINT('',#52927);
#8570=VERTEX_POINT('',#53166);
#8571=VERTEX_POINT('',#53213);
#8572=VERTEX_POINT('',#53220);
#8573=VERTEX_POINT('',#53240);
#8574=VERTEX_POINT('',#53247);
#8575=VERTEX_POINT('',#53749);
#8576=VERTEX_POINT('',#53983);
#8577=VERTEX_POINT('',#54030);
#8578=VERTEX_POINT('',#54037);
#8579=VERTEX_POINT('',#54057);
#8580=VERTEX_POINT('',#54064);
#8581=VERTEX_POINT('',#54601);
#8582=VERTEX_POINT('',#54835);
#8583=VERTEX_POINT('',#54882);
#8584=VERTEX_POINT('',#54889);
#8585=VERTEX_POINT('',#54909);
#8586=VERTEX_POINT('',#54916);
#8587=VERTEX_POINT('',#55418);
#8588=VERTEX_POINT('',#55652);
#8589=VERTEX_POINT('',#55699);
#8590=VERTEX_POINT('',#55706);
#8591=VERTEX_POINT('',#55726);
#8592=VERTEX_POINT('',#55733);
#8593=VERTEX_POINT('',#55738);
#8594=VERTEX_POINT('',#56524);
#8595=VERTEX_POINT('',#56533);
#8596=VERTEX_POINT('',#56536);
#8597=VERTEX_POINT('',#56538);
#8598=VERTEX_POINT('',#56591);
#8599=VERTEX_POINT('',#56801);
#8600=VERTEX_POINT('',#56808);
#8601=VERTEX_POINT('',#56828);
#8602=VERTEX_POINT('',#57373);
#8603=VERTEX_POINT('',#57377);
#8604=VERTEX_POINT('',#57384);
#8605=VERTEX_POINT('',#57385);
#8606=VERTEX_POINT('',#57393);
#8607=VERTEX_POINT('',#57395);
#8608=VERTEX_POINT('',#57397);
#8609=VERTEX_POINT('',#57406);
#8610=VERTEX_POINT('',#57411);
#8611=VERTEX_POINT('',#57430);
#8612=VERTEX_POINT('',#57435);
#8613=VERTEX_POINT('',#57440);
#8614=VERTEX_POINT('',#57450);
#8615=VERTEX_POINT('',#57451);
#8616=VERTEX_POINT('',#57459);
#8617=VERTEX_POINT('',#57461);
#8618=VERTEX_POINT('',#57463);
#8619=VERTEX_POINT('',#57472);
#8620=VERTEX_POINT('',#57477);
#8621=VERTEX_POINT('',#57496);
#8622=VERTEX_POINT('',#57501);
#8623=VERTEX_POINT('',#57506);
#8624=VERTEX_POINT('',#57516);
#8625=VERTEX_POINT('',#57517);
#8626=VERTEX_POINT('',#57525);
#8627=VERTEX_POINT('',#57527);
#8628=VERTEX_POINT('',#57529);
#8629=VERTEX_POINT('',#57538);
#8630=VERTEX_POINT('',#57543);
#8631=VERTEX_POINT('',#57562);
#8632=VERTEX_POINT('',#57567);
#8633=VERTEX_POINT('',#57572);
#8634=VERTEX_POINT('',#57582);
#8635=VERTEX_POINT('',#57583);
#8636=VERTEX_POINT('',#57587);
#8637=VERTEX_POINT('',#57589);
#8638=VERTEX_POINT('',#57593);
#8639=VERTEX_POINT('',#57597);
#8640=VERTEX_POINT('',#57601);
#8641=VERTEX_POINT('',#57608);
#8642=VERTEX_POINT('',#57612);
#8643=VERTEX_POINT('',#57616);
#8644=VERTEX_POINT('',#57620);
#8645=VERTEX_POINT('',#57624);
#8646=VERTEX_POINT('',#57628);
#8647=VERTEX_POINT('',#57632);
#8648=VERTEX_POINT('',#57637);
#8649=VERTEX_POINT('',#57642);
#8650=VERTEX_POINT('',#57647);
#8651=VERTEX_POINT('',#57658);
#8652=VERTEX_POINT('',#57660);
#8653=VERTEX_POINT('',#57664);
#8654=VERTEX_POINT('',#57668);
#8655=VERTEX_POINT('',#57669);
#8656=VERTEX_POINT('',#57677);
#8657=VERTEX_POINT('',#57679);
#8658=VERTEX_POINT('',#57681);
#8659=VERTEX_POINT('',#57690);
#8660=VERTEX_POINT('',#57695);
#8661=VERTEX_POINT('',#57714);
#8662=VERTEX_POINT('',#57719);
#8663=VERTEX_POINT('',#57724);
#8664=VERTEX_POINT('',#57749);
#8665=VERTEX_POINT('',#57754);
#8666=VERTEX_POINT('',#57759);
#8667=VERTEX_POINT('',#57769);
#8668=VERTEX_POINT('',#57770);
#8669=VERTEX_POINT('',#57778);
#8670=VERTEX_POINT('',#57780);
#8671=VERTEX_POINT('',#57782);
#8672=VERTEX_POINT('',#57795);
#8673=VERTEX_POINT('',#57814);
#8674=VERTEX_POINT('',#57819);
#8675=VERTEX_POINT('',#57844);
#8676=VERTEX_POINT('',#57849);
#8677=VERTEX_POINT('',#57854);
#8678=VERTEX_POINT('',#57864);
#8679=VERTEX_POINT('',#57865);
#8680=VERTEX_POINT('',#57873);
#8681=VERTEX_POINT('',#57875);
#8682=VERTEX_POINT('',#57877);
#8683=VERTEX_POINT('',#57890);
#8684=VERTEX_POINT('',#57909);
#8685=VERTEX_POINT('',#57914);
#8686=VERTEX_POINT('',#57924);
#8687=VERTEX_POINT('',#57925);
#8688=VERTEX_POINT('',#57933);
#8689=VERTEX_POINT('',#57935);
#8690=VERTEX_POINT('',#57937);
#8691=VERTEX_POINT('',#57946);
#8692=VERTEX_POINT('',#57951);
#8693=VERTEX_POINT('',#57996);
#8694=VERTEX_POINT('',#58001);
#8695=VERTEX_POINT('',#58011);
#8696=VERTEX_POINT('',#58012);
#8697=VERTEX_POINT('',#58020);
#8698=VERTEX_POINT('',#58022);
#8699=VERTEX_POINT('',#58024);
#8700=VERTEX_POINT('',#58037);
#8701=VERTEX_POINT('',#58056);
#8702=VERTEX_POINT('',#58061);
#8703=VERTEX_POINT('',#58086);
#8704=VERTEX_POINT('',#58091);
#8705=VERTEX_POINT('',#58096);
#8706=VERTEX_POINT('',#58106);
#8707=VERTEX_POINT('',#58107);
#8708=VERTEX_POINT('',#58115);
#8709=VERTEX_POINT('',#58117);
#8710=VERTEX_POINT('',#58119);
#8711=VERTEX_POINT('',#58132);
#8712=VERTEX_POINT('',#58151);
#8713=VERTEX_POINT('',#58156);
#8714=VERTEX_POINT('',#58181);
#8715=VERTEX_POINT('',#58186);
#8716=VERTEX_POINT('',#58191);
#8717=VERTEX_POINT('',#58201);
#8718=VERTEX_POINT('',#58202);
#8719=VERTEX_POINT('',#58210);
#8720=VERTEX_POINT('',#58212);
#8721=VERTEX_POINT('',#58214);
#8722=VERTEX_POINT('',#58227);
#8723=VERTEX_POINT('',#58246);
#8724=VERTEX_POINT('',#58251);
#8725=VERTEX_POINT('',#58280);
#8726=VERTEX_POINT('',#58305);
#8727=VERTEX_POINT('',#58310);
#8728=VERTEX_POINT('',#58338);
#8729=VERTEX_POINT('',#58343);
#8730=VERTEX_POINT('',#58371);
#8731=VERTEX_POINT('',#58376);
#8732=VERTEX_POINT('',#58404);
#8733=VERTEX_POINT('',#58409);
#8734=VERTEX_POINT('',#58437);
#8735=VERTEX_POINT('',#58442);
#8736=VERTEX_POINT('',#58470);
#8737=VERTEX_POINT('',#58475);
#8738=VERTEX_POINT('',#58507);
#8739=VERTEX_POINT('',#58532);
#8740=VERTEX_POINT('',#58537);
#8741=VERTEX_POINT('',#58569);
#8742=VERTEX_POINT('',#58594);
#8743=VERTEX_POINT('',#58599);
#8744=VERTEX_POINT('',#58631);
#8745=VERTEX_POINT('',#58656);
#8746=VERTEX_POINT('',#58704);
#8747=VERTEX_POINT('',#58729);
#8748=VERTEX_POINT('',#58754);
#8749=VERTEX_POINT('',#58799);
#8750=VERTEX_POINT('',#58824);
#8751=VERTEX_POINT('',#58849);
#8752=VERTEX_POINT('',#58874);
#8753=VERTEX_POINT('',#58899);
#8754=VERTEX_POINT('',#58925);
#8755=VERTEX_POINT('',#58936);
#8756=VERTEX_POINT('',#58940);
#8757=VERTEX_POINT('',#58942);
#8758=VERTEX_POINT('',#58964);
#8759=VERTEX_POINT('',#58967);
#8760=VERTEX_POINT('',#58971);
#8761=VERTEX_POINT('',#58975);
#8762=VERTEX_POINT('',#58981);
#8763=VERTEX_POINT('',#58982);
#8764=VERTEX_POINT('',#58986);
#8765=VERTEX_POINT('',#58988);
#8766=VERTEX_POINT('',#58994);
#8767=VERTEX_POINT('',#58995);
#8768=VERTEX_POINT('',#58999);
#8769=VERTEX_POINT('',#59001);
#8770=VERTEX_POINT('',#59007);
#8771=VERTEX_POINT('',#59008);
#8772=VERTEX_POINT('',#59012);
#8773=VERTEX_POINT('',#59014);
#8774=VERTEX_POINT('',#59020);
#8775=VERTEX_POINT('',#59021);
#8776=VERTEX_POINT('',#59025);
#8777=VERTEX_POINT('',#59027);
#8778=VERTEX_POINT('',#59033);
#8779=VERTEX_POINT('',#59034);
#8780=VERTEX_POINT('',#59072);
#8781=VERTEX_POINT('',#59074);
#8782=VERTEX_POINT('',#59112);
#8783=VERTEX_POINT('',#59113);
#8784=VERTEX_POINT('',#59151);
#8785=VERTEX_POINT('',#59153);
#8786=VERTEX_POINT('',#59191);
#8787=VERTEX_POINT('',#59192);
#8788=VERTEX_POINT('',#59230);
#8789=VERTEX_POINT('',#59232);
#8790=VERTEX_POINT('',#59243);
#8791=VERTEX_POINT('',#59273);
#8792=VERTEX_POINT('',#59274);
#8793=VERTEX_POINT('',#59312);
#8794=VERTEX_POINT('',#59314);
#8795=VERTEX_POINT('',#59352);
#8796=VERTEX_POINT('',#59355);
#8797=VERTEX_POINT('',#59359);
#8798=VERTEX_POINT('',#59362);
#8799=VERTEX_POINT('',#59365);
#8800=VERTEX_POINT('',#59369);
#8801=VERTEX_POINT('',#59371);
#8802=VERTEX_POINT('',#59377);
#8803=VERTEX_POINT('',#59381);
#8804=VERTEX_POINT('',#59384);
#8805=VERTEX_POINT('',#59389);
#8806=VERTEX_POINT('',#59393);
#8807=VERTEX_POINT('',#59399);
#8808=VERTEX_POINT('',#59401);
#8809=VERTEX_POINT('',#59405);
#8810=VERTEX_POINT('',#59409);
#8811=VERTEX_POINT('',#59410);
#8812=VERTEX_POINT('',#59412);
#8813=VERTEX_POINT('',#59414);
#8814=VERTEX_POINT('',#59416);
#8815=VERTEX_POINT('',#59418);
#8816=VERTEX_POINT('',#59420);
#8817=VERTEX_POINT('',#59422);
#8818=VERTEX_POINT('',#59424);
#8819=VERTEX_POINT('',#59426);
#8820=VERTEX_POINT('',#59428);
#8821=VERTEX_POINT('',#59430);
#8822=VERTEX_POINT('',#59432);
#8823=VERTEX_POINT('',#59434);
#8824=VERTEX_POINT('',#59436);
#8825=VERTEX_POINT('',#59438);
#8826=VERTEX_POINT('',#59440);
#8827=VERTEX_POINT('',#59442);
#8828=VERTEX_POINT('',#59444);
#8829=VERTEX_POINT('',#59446);
#8830=VERTEX_POINT('',#59448);
#8831=VERTEX_POINT('',#59450);
#8832=VERTEX_POINT('',#59452);
#8833=VERTEX_POINT('',#59454);
#8834=VERTEX_POINT('',#59456);
#8835=VERTEX_POINT('',#59458);
#8836=VERTEX_POINT('',#59460);
#8837=VERTEX_POINT('',#59462);
#8838=VERTEX_POINT('',#59464);
#8839=VERTEX_POINT('',#59466);
#8840=VERTEX_POINT('',#59468);
#8841=VERTEX_POINT('',#59470);
#8842=VERTEX_POINT('',#59472);
#8843=VERTEX_POINT('',#59474);
#8844=VERTEX_POINT('',#59476);
#8845=VERTEX_POINT('',#59478);
#8846=VERTEX_POINT('',#59480);
#8847=VERTEX_POINT('',#59482);
#8848=VERTEX_POINT('',#59484);
#8849=VERTEX_POINT('',#59486);
#8850=VERTEX_POINT('',#59488);
#8851=VERTEX_POINT('',#59490);
#8852=VERTEX_POINT('',#59492);
#8853=VERTEX_POINT('',#59494);
#8854=VERTEX_POINT('',#59496);
#8855=VERTEX_POINT('',#59498);
#8856=VERTEX_POINT('',#59500);
#8857=VERTEX_POINT('',#59502);
#8858=VERTEX_POINT('',#59504);
#8859=VERTEX_POINT('',#59506);
#8860=VERTEX_POINT('',#59508);
#8861=VERTEX_POINT('',#59510);
#8862=VERTEX_POINT('',#59512);
#8863=VERTEX_POINT('',#59514);
#8864=VERTEX_POINT('',#59516);
#8865=VERTEX_POINT('',#59518);
#8866=VERTEX_POINT('',#59520);
#8867=VERTEX_POINT('',#59522);
#8868=VERTEX_POINT('',#59524);
#8869=VERTEX_POINT('',#59526);
#8870=VERTEX_POINT('',#59528);
#8871=VERTEX_POINT('',#59530);
#8872=VERTEX_POINT('',#59532);
#8873=VERTEX_POINT('',#59534);
#8874=VERTEX_POINT('',#59536);
#8875=VERTEX_POINT('',#59538);
#8876=VERTEX_POINT('',#59540);
#8877=VERTEX_POINT('',#59542);
#8878=VERTEX_POINT('',#59544);
#8879=VERTEX_POINT('',#59546);
#8880=VERTEX_POINT('',#59548);
#8881=VERTEX_POINT('',#59550);
#8882=VERTEX_POINT('',#59552);
#8883=VERTEX_POINT('',#59554);
#8884=VERTEX_POINT('',#59556);
#8885=VERTEX_POINT('',#59558);
#8886=VERTEX_POINT('',#59560);
#8887=VERTEX_POINT('',#59562);
#8888=VERTEX_POINT('',#59564);
#8889=VERTEX_POINT('',#59566);
#8890=VERTEX_POINT('',#59568);
#8891=VERTEX_POINT('',#59570);
#8892=VERTEX_POINT('',#59572);
#8893=VERTEX_POINT('',#59574);
#8894=VERTEX_POINT('',#59576);
#8895=VERTEX_POINT('',#59578);
#8896=VERTEX_POINT('',#59580);
#8897=VERTEX_POINT('',#59582);
#8898=VERTEX_POINT('',#59584);
#8899=VERTEX_POINT('',#59586);
#8900=VERTEX_POINT('',#59588);
#8901=VERTEX_POINT('',#59590);
#8902=VERTEX_POINT('',#59592);
#8903=VERTEX_POINT('',#59594);
#8904=VERTEX_POINT('',#59596);
#8905=VERTEX_POINT('',#59598);
#8906=VERTEX_POINT('',#59600);
#8907=VERTEX_POINT('',#59602);
#8908=VERTEX_POINT('',#59604);
#8909=VERTEX_POINT('',#59606);
#8910=VERTEX_POINT('',#59608);
#8911=VERTEX_POINT('',#59610);
#8912=VERTEX_POINT('',#59612);
#8913=VERTEX_POINT('',#59614);
#8914=VERTEX_POINT('',#59616);
#8915=VERTEX_POINT('',#59618);
#8916=VERTEX_POINT('',#59620);
#8917=VERTEX_POINT('',#59622);
#8918=VERTEX_POINT('',#59624);
#8919=VERTEX_POINT('',#59626);
#8920=VERTEX_POINT('',#59628);
#8921=VERTEX_POINT('',#59630);
#8922=VERTEX_POINT('',#59632);
#8923=VERTEX_POINT('',#59634);
#8924=VERTEX_POINT('',#59636);
#8925=VERTEX_POINT('',#59638);
#8926=VERTEX_POINT('',#59640);
#8927=VERTEX_POINT('',#59642);
#8928=VERTEX_POINT('',#59644);
#8929=VERTEX_POINT('',#59646);
#8930=VERTEX_POINT('',#59648);
#8931=VERTEX_POINT('',#59650);
#8932=VERTEX_POINT('',#59652);
#8933=VERTEX_POINT('',#59654);
#8934=VERTEX_POINT('',#59656);
#8935=VERTEX_POINT('',#59658);
#8936=VERTEX_POINT('',#59660);
#8937=VERTEX_POINT('',#59662);
#8938=VERTEX_POINT('',#59664);
#8939=VERTEX_POINT('',#59666);
#8940=VERTEX_POINT('',#59668);
#8941=VERTEX_POINT('',#59670);
#8942=VERTEX_POINT('',#59672);
#8943=VERTEX_POINT('',#59674);
#8944=VERTEX_POINT('',#59676);
#8945=VERTEX_POINT('',#59678);
#8946=VERTEX_POINT('',#59680);
#8947=VERTEX_POINT('',#59682);
#8948=VERTEX_POINT('',#59684);
#8949=VERTEX_POINT('',#59686);
#8950=VERTEX_POINT('',#59688);
#8951=VERTEX_POINT('',#59690);
#8952=VERTEX_POINT('',#59692);
#8953=VERTEX_POINT('',#59694);
#8954=VERTEX_POINT('',#59696);
#8955=VERTEX_POINT('',#59698);
#8956=VERTEX_POINT('',#59700);
#8957=VERTEX_POINT('',#59702);
#8958=VERTEX_POINT('',#59704);
#8959=VERTEX_POINT('',#59706);
#8960=VERTEX_POINT('',#59709);
#8961=VERTEX_POINT('',#59712);
#8962=VERTEX_POINT('',#59716);
#8963=VERTEX_POINT('',#59717);
#8964=VERTEX_POINT('',#59719);
#8965=VERTEX_POINT('',#59721);
#8966=VERTEX_POINT('',#59723);
#8967=VERTEX_POINT('',#59725);
#8968=VERTEX_POINT('',#59727);
#8969=VERTEX_POINT('',#59729);
#8970=VERTEX_POINT('',#59731);
#8971=VERTEX_POINT('',#59733);
#8972=VERTEX_POINT('',#59735);
#8973=VERTEX_POINT('',#59737);
#8974=VERTEX_POINT('',#59739);
#8975=VERTEX_POINT('',#59741);
#8976=VERTEX_POINT('',#59743);
#8977=VERTEX_POINT('',#59745);
#8978=VERTEX_POINT('',#59747);
#8979=VERTEX_POINT('',#59749);
#8980=VERTEX_POINT('',#59751);
#8981=VERTEX_POINT('',#59753);
#8982=VERTEX_POINT('',#59755);
#8983=VERTEX_POINT('',#59757);
#8984=VERTEX_POINT('',#59759);
#8985=VERTEX_POINT('',#59761);
#8986=VERTEX_POINT('',#59763);
#8987=VERTEX_POINT('',#59765);
#8988=VERTEX_POINT('',#59767);
#8989=VERTEX_POINT('',#59769);
#8990=VERTEX_POINT('',#59771);
#8991=VERTEX_POINT('',#59773);
#8992=VERTEX_POINT('',#59775);
#8993=VERTEX_POINT('',#59777);
#8994=VERTEX_POINT('',#59779);
#8995=VERTEX_POINT('',#59781);
#8996=VERTEX_POINT('',#59783);
#8997=VERTEX_POINT('',#59785);
#8998=VERTEX_POINT('',#59787);
#8999=VERTEX_POINT('',#59789);
#9000=VERTEX_POINT('',#59791);
#9001=VERTEX_POINT('',#59793);
#9002=VERTEX_POINT('',#59795);
#9003=VERTEX_POINT('',#59797);
#9004=VERTEX_POINT('',#59799);
#9005=VERTEX_POINT('',#59801);
#9006=VERTEX_POINT('',#59803);
#9007=VERTEX_POINT('',#59805);
#9008=VERTEX_POINT('',#59807);
#9009=VERTEX_POINT('',#59809);
#9010=VERTEX_POINT('',#59811);
#9011=VERTEX_POINT('',#59813);
#9012=VERTEX_POINT('',#59815);
#9013=VERTEX_POINT('',#59817);
#9014=VERTEX_POINT('',#59819);
#9015=VERTEX_POINT('',#59821);
#9016=VERTEX_POINT('',#59823);
#9017=VERTEX_POINT('',#59825);
#9018=VERTEX_POINT('',#59827);
#9019=VERTEX_POINT('',#59829);
#9020=VERTEX_POINT('',#59831);
#9021=VERTEX_POINT('',#59833);
#9022=VERTEX_POINT('',#59835);
#9023=VERTEX_POINT('',#59837);
#9024=VERTEX_POINT('',#59839);
#9025=VERTEX_POINT('',#59841);
#9026=VERTEX_POINT('',#59843);
#9027=VERTEX_POINT('',#59845);
#9028=VERTEX_POINT('',#59847);
#9029=VERTEX_POINT('',#59849);
#9030=VERTEX_POINT('',#59851);
#9031=VERTEX_POINT('',#59853);
#9032=VERTEX_POINT('',#59855);
#9033=VERTEX_POINT('',#59857);
#9034=VERTEX_POINT('',#59859);
#9035=VERTEX_POINT('',#59861);
#9036=VERTEX_POINT('',#59863);
#9037=VERTEX_POINT('',#59865);
#9038=VERTEX_POINT('',#59867);
#9039=VERTEX_POINT('',#59869);
#9040=VERTEX_POINT('',#59871);
#9041=VERTEX_POINT('',#59873);
#9042=VERTEX_POINT('',#59875);
#9043=VERTEX_POINT('',#59877);
#9044=VERTEX_POINT('',#59879);
#9045=VERTEX_POINT('',#59881);
#9046=VERTEX_POINT('',#59883);
#9047=VERTEX_POINT('',#59885);
#9048=VERTEX_POINT('',#59887);
#9049=VERTEX_POINT('',#59889);
#9050=VERTEX_POINT('',#59891);
#9051=VERTEX_POINT('',#59893);
#9052=VERTEX_POINT('',#59895);
#9053=VERTEX_POINT('',#59897);
#9054=VERTEX_POINT('',#59899);
#9055=VERTEX_POINT('',#59901);
#9056=VERTEX_POINT('',#59903);
#9057=VERTEX_POINT('',#59905);
#9058=VERTEX_POINT('',#59907);
#9059=VERTEX_POINT('',#59909);
#9060=VERTEX_POINT('',#59911);
#9061=VERTEX_POINT('',#59913);
#9062=VERTEX_POINT('',#59915);
#9063=VERTEX_POINT('',#59917);
#9064=VERTEX_POINT('',#59919);
#9065=VERTEX_POINT('',#59921);
#9066=VERTEX_POINT('',#59923);
#9067=VERTEX_POINT('',#59925);
#9068=VERTEX_POINT('',#59927);
#9069=VERTEX_POINT('',#59929);
#9070=VERTEX_POINT('',#59931);
#9071=VERTEX_POINT('',#59933);
#9072=VERTEX_POINT('',#59935);
#9073=VERTEX_POINT('',#59937);
#9074=VERTEX_POINT('',#59939);
#9075=VERTEX_POINT('',#59941);
#9076=VERTEX_POINT('',#59943);
#9077=VERTEX_POINT('',#59945);
#9078=VERTEX_POINT('',#59947);
#9079=VERTEX_POINT('',#59949);
#9080=VERTEX_POINT('',#59951);
#9081=VERTEX_POINT('',#59953);
#9082=VERTEX_POINT('',#59955);
#9083=VERTEX_POINT('',#59957);
#9084=VERTEX_POINT('',#59959);
#9085=VERTEX_POINT('',#59961);
#9086=VERTEX_POINT('',#59963);
#9087=VERTEX_POINT('',#59965);
#9088=VERTEX_POINT('',#59967);
#9089=VERTEX_POINT('',#59969);
#9090=VERTEX_POINT('',#59971);
#9091=VERTEX_POINT('',#59973);
#9092=VERTEX_POINT('',#59975);
#9093=VERTEX_POINT('',#59977);
#9094=VERTEX_POINT('',#59979);
#9095=VERTEX_POINT('',#59981);
#9096=VERTEX_POINT('',#59983);
#9097=VERTEX_POINT('',#59985);
#9098=VERTEX_POINT('',#59987);
#9099=VERTEX_POINT('',#59989);
#9100=VERTEX_POINT('',#59991);
#9101=VERTEX_POINT('',#59993);
#9102=VERTEX_POINT('',#59995);
#9103=VERTEX_POINT('',#59997);
#9104=VERTEX_POINT('',#59999);
#9105=VERTEX_POINT('',#60001);
#9106=VERTEX_POINT('',#60003);
#9107=VERTEX_POINT('',#60005);
#9108=VERTEX_POINT('',#60007);
#9109=VERTEX_POINT('',#60009);
#9110=VERTEX_POINT('',#60011);
#9111=VERTEX_POINT('',#60013);
#9112=VERTEX_POINT('',#60016);
#9113=VERTEX_POINT('',#60019);
#9114=VERTEX_POINT('',#60023);
#9115=EDGE_CURVE('',#7324,#7325,#4500,.T.);
#9116=EDGE_CURVE('',#7324,#7326,#3705,.T.);
#9117=EDGE_CURVE('',#7326,#7327,#3300,.T.);
#9118=EDGE_CURVE('',#7327,#7325,#3706,.T.);
#9119=EDGE_CURVE('',#7328,#7329,#4501,.T.);
#9120=EDGE_CURVE('',#7328,#7324,#3707,.T.);
#9121=EDGE_CURVE('',#7325,#7329,#3708,.T.);
#9122=EDGE_CURVE('',#7330,#7331,#4502,.T.);
#9123=EDGE_CURVE('',#7330,#7328,#3709,.T.);
#9124=EDGE_CURVE('',#7329,#7331,#3710,.T.);
#9125=EDGE_CURVE('',#7332,#7333,#4503,.T.);
#9126=EDGE_CURVE('',#7332,#7330,#3711,.T.);
#9127=EDGE_CURVE('',#7331,#7333,#3712,.T.);
#9128=EDGE_CURVE('',#7334,#7335,#4504,.T.);
#9129=EDGE_CURVE('',#7334,#7332,#3713,.T.);
#9130=EDGE_CURVE('',#7333,#7335,#3714,.T.);
#9131=EDGE_CURVE('',#7336,#7337,#4505,.T.);
#9132=EDGE_CURVE('',#7336,#7334,#3715,.T.);
#9133=EDGE_CURVE('',#7335,#7337,#3716,.T.);
#9134=EDGE_CURVE('',#7338,#7339,#4506,.T.);
#9135=EDGE_CURVE('',#7338,#7336,#3717,.T.);
#9136=EDGE_CURVE('',#7337,#7339,#3718,.T.);
#9137=EDGE_CURVE('',#7340,#7341,#4507,.T.);
#9138=EDGE_CURVE('',#7340,#7338,#3719,.T.);
#9139=EDGE_CURVE('',#7339,#7341,#3720,.T.);
#9140=EDGE_CURVE('',#7342,#7343,#4508,.T.);
#9141=EDGE_CURVE('',#7342,#7340,#3721,.T.);
#9142=EDGE_CURVE('',#7341,#7343,#3722,.T.);
#9143=EDGE_CURVE('',#7344,#7345,#4509,.T.);
#9144=EDGE_CURVE('',#7344,#7342,#3723,.T.);
#9145=EDGE_CURVE('',#7343,#7345,#3724,.T.);
#9146=EDGE_CURVE('',#7346,#7347,#4510,.T.);
#9147=EDGE_CURVE('',#7346,#7344,#3725,.T.);
#9148=EDGE_CURVE('',#7345,#7347,#3726,.T.);
#9149=EDGE_CURVE('',#7348,#7349,#4511,.T.);
#9150=EDGE_CURVE('',#7348,#7346,#3727,.T.);
#9151=EDGE_CURVE('',#7347,#7349,#3728,.T.);
#9152=EDGE_CURVE('',#7350,#7351,#4512,.T.);
#9153=EDGE_CURVE('',#7350,#7348,#3729,.T.);
#9154=EDGE_CURVE('',#7349,#7351,#3730,.T.);
#9155=EDGE_CURVE('',#7352,#7353,#4513,.T.);
#9156=EDGE_CURVE('',#7352,#7350,#3731,.T.);
#9157=EDGE_CURVE('',#7351,#7353,#3732,.T.);
#9158=EDGE_CURVE('',#7354,#7355,#4514,.T.);
#9159=EDGE_CURVE('',#7354,#7352,#3733,.T.);
#9160=EDGE_CURVE('',#7353,#7355,#3734,.T.);
#9161=EDGE_CURVE('',#7356,#7357,#4515,.T.);
#9162=EDGE_CURVE('',#7356,#7354,#3735,.T.);
#9163=EDGE_CURVE('',#7355,#7357,#3736,.T.);
#9164=EDGE_CURVE('',#7358,#7359,#976,.T.);
#9165=EDGE_CURVE('',#7358,#7360,#3737,.T.);
#9166=EDGE_CURVE('',#7360,#7361,#3738,.T.);
#9167=EDGE_CURVE('',#7361,#7362,#3739,.T.);
#9168=EDGE_CURVE('',#7363,#7362,#977,.T.);
#9169=EDGE_CURVE('',#7363,#7363,#3301,.T.);
#9170=EDGE_CURVE('',#7362,#7364,#3740,.T.);
#9171=EDGE_CURVE('',#7365,#7364,#3302,.T.);
#9172=EDGE_CURVE('',#7365,#7366,#3741,.T.);
#9173=EDGE_CURVE('',#7366,#7367,#3742,.T.);
#9174=EDGE_CURVE('',#7367,#7368,#3743,.T.);
#9175=EDGE_CURVE('',#7369,#7368,#3303,.T.);
#9176=EDGE_CURVE('',#7369,#7370,#3744,.T.);
#9177=EDGE_CURVE('',#7370,#7371,#3745,.T.);
#9178=EDGE_CURVE('',#7371,#7372,#3746,.T.);
#9179=EDGE_CURVE('',#7373,#7372,#3304,.T.);
#9180=EDGE_CURVE('',#7373,#7374,#3747,.T.);
#9181=EDGE_CURVE('',#7374,#7375,#3748,.T.);
#9182=EDGE_CURVE('',#7375,#7376,#3749,.T.);
#9183=EDGE_CURVE('',#7377,#7376,#3305,.T.);
#9184=EDGE_CURVE('',#7377,#7378,#3750,.T.);
#9185=EDGE_CURVE('',#7378,#7379,#3751,.T.);
#9186=EDGE_CURVE('',#7379,#7380,#3752,.T.);
#9187=EDGE_CURVE('',#7381,#7380,#3306,.T.);
#9188=EDGE_CURVE('',#7381,#7382,#3753,.T.);
#9189=EDGE_CURVE('',#7382,#7383,#3754,.T.);
#9190=EDGE_CURVE('',#7383,#7384,#3755,.T.);
#9191=EDGE_CURVE('',#7385,#7384,#3307,.T.);
#9192=EDGE_CURVE('',#7385,#7386,#3756,.T.);
#9193=EDGE_CURVE('',#7386,#7387,#3757,.T.);
#9194=EDGE_CURVE('',#7387,#7388,#3758,.T.);
#9195=EDGE_CURVE('',#7389,#7388,#3308,.T.);
#9196=EDGE_CURVE('',#7389,#7390,#3759,.T.);
#9197=EDGE_CURVE('',#7390,#7391,#3760,.T.);
#9198=EDGE_CURVE('',#7391,#7392,#3761,.T.);
#9199=EDGE_CURVE('',#7393,#7392,#3309,.T.);
#9200=EDGE_CURVE('',#7393,#7394,#3762,.T.);
#9201=EDGE_CURVE('',#7394,#7395,#3763,.T.);
#9202=EDGE_CURVE('',#7395,#7396,#3764,.T.);
#9203=EDGE_CURVE('',#7397,#7396,#3310,.T.);
#9204=EDGE_CURVE('',#7397,#7398,#3765,.T.);
#9205=EDGE_CURVE('',#7398,#7399,#3766,.T.);
#9206=EDGE_CURVE('',#7399,#7400,#3767,.T.);
#9207=EDGE_CURVE('',#7401,#7400,#3311,.T.);
#9208=EDGE_CURVE('',#7401,#7402,#3768,.T.);
#9209=EDGE_CURVE('',#7402,#7403,#3769,.T.);
#9210=EDGE_CURVE('',#7403,#7404,#3770,.T.);
#9211=EDGE_CURVE('',#7405,#7404,#3312,.T.);
#9212=EDGE_CURVE('',#7405,#7406,#3771,.T.);
#9213=EDGE_CURVE('',#7406,#7407,#3772,.T.);
#9214=EDGE_CURVE('',#7407,#7408,#3773,.T.);
#9215=EDGE_CURVE('',#7409,#7408,#3313,.T.);
#9216=EDGE_CURVE('',#7409,#7410,#3774,.T.);
#9217=EDGE_CURVE('',#7410,#7411,#3775,.T.);
#9218=EDGE_CURVE('',#7411,#7412,#3776,.T.);
#9219=EDGE_CURVE('',#7413,#7412,#3314,.T.);
#9220=EDGE_CURVE('',#7413,#7414,#3777,.T.);
#9221=EDGE_CURVE('',#7414,#7415,#3778,.T.);
#9222=EDGE_CURVE('',#7415,#7416,#3779,.T.);
#9223=EDGE_CURVE('',#7417,#7416,#3315,.T.);
#9224=EDGE_CURVE('',#7417,#7418,#3780,.T.);
#9225=EDGE_CURVE('',#7418,#7419,#3781,.T.);
#9226=EDGE_CURVE('',#7419,#7420,#3782,.T.);
#9227=EDGE_CURVE('',#7421,#7420,#3316,.T.);
#9228=EDGE_CURVE('',#7421,#7422,#3783,.T.);
#9229=EDGE_CURVE('',#7422,#7423,#3784,.T.);
#9230=EDGE_CURVE('',#7423,#7424,#3785,.T.);
#9231=EDGE_CURVE('',#7425,#7424,#3317,.T.);
#9232=EDGE_CURVE('',#7425,#7426,#3786,.T.);
#9233=EDGE_CURVE('',#7426,#7427,#3787,.T.);
#9234=EDGE_CURVE('',#7427,#7428,#3788,.T.);
#9235=EDGE_CURVE('',#7429,#7428,#3318,.T.);
#9236=EDGE_CURVE('',#7429,#7430,#3789,.T.);
#9237=EDGE_CURVE('',#7430,#7431,#3790,.T.);
#9238=EDGE_CURVE('',#7431,#7432,#3791,.T.);
#9239=EDGE_CURVE('',#7433,#7432,#3319,.T.);
#9240=EDGE_CURVE('',#7433,#7434,#3792,.T.);
#9241=EDGE_CURVE('',#7434,#7435,#3793,.T.);
#9242=EDGE_CURVE('',#7435,#7436,#3794,.T.);
#9243=EDGE_CURVE('',#7437,#7436,#3320,.T.);
#9244=EDGE_CURVE('',#7437,#7438,#3795,.T.);
#9245=EDGE_CURVE('',#7438,#7439,#3796,.T.);
#9246=EDGE_CURVE('',#7439,#7440,#3797,.T.);
#9247=EDGE_CURVE('',#7441,#7440,#3321,.T.);
#9248=EDGE_CURVE('',#7441,#7442,#3798,.T.);
#9249=EDGE_CURVE('',#7442,#7443,#3799,.T.);
#9250=EDGE_CURVE('',#7443,#7444,#3800,.T.);
#9251=EDGE_CURVE('',#7445,#7444,#3322,.T.);
#9252=EDGE_CURVE('',#7445,#7446,#3801,.T.);
#9253=EDGE_CURVE('',#7446,#7447,#3802,.T.);
#9254=EDGE_CURVE('',#7447,#7448,#3803,.T.);
#9255=EDGE_CURVE('',#7449,#7448,#3323,.T.);
#9256=EDGE_CURVE('',#7449,#7450,#3804,.T.);
#9257=EDGE_CURVE('',#7450,#7451,#3805,.T.);
#9258=EDGE_CURVE('',#7451,#7359,#3806,.T.);
#9259=EDGE_CURVE('',#7452,#7453,#4516,.T.);
#9260=EDGE_CURVE('',#7452,#7454,#3807,.T.);
#9261=EDGE_CURVE('',#7455,#7454,#3324,.T.);
#9262=EDGE_CURVE('',#7453,#7455,#3808,.T.);
#9263=EDGE_CURVE('',#7456,#7457,#4517,.T.);
#9264=EDGE_CURVE('',#7456,#7452,#3809,.T.);
#9265=EDGE_CURVE('',#7457,#7453,#3810,.T.);
#9266=EDGE_CURVE('',#7458,#7459,#4518,.T.);
#9267=EDGE_CURVE('',#7458,#7456,#3811,.T.);
#9268=EDGE_CURVE('',#7459,#7457,#3812,.T.);
#9269=EDGE_CURVE('',#7460,#7461,#4519,.T.);
#9270=EDGE_CURVE('',#7460,#7458,#3813,.T.);
#9271=EDGE_CURVE('',#7461,#7459,#3814,.T.);
#9272=EDGE_CURVE('',#7462,#7463,#4520,.T.);
#9273=EDGE_CURVE('',#7462,#7460,#3815,.T.);
#9274=EDGE_CURVE('',#7463,#7461,#3816,.T.);
#9275=EDGE_CURVE('',#7464,#7465,#4521,.T.);
#9276=EDGE_CURVE('',#7464,#7462,#3817,.T.);
#9277=EDGE_CURVE('',#7465,#7463,#3818,.T.);
#9278=EDGE_CURVE('',#7466,#7467,#4522,.T.);
#9279=EDGE_CURVE('',#7466,#7464,#3819,.T.);
#9280=EDGE_CURVE('',#7467,#7465,#3820,.T.);
#9281=EDGE_CURVE('',#7468,#7469,#4523,.T.);
#9282=EDGE_CURVE('',#7468,#7466,#3821,.T.);
#9283=EDGE_CURVE('',#7469,#7467,#3822,.T.);
#9284=EDGE_CURVE('',#7470,#7471,#4524,.T.);
#9285=EDGE_CURVE('',#7470,#7468,#3823,.T.);
#9286=EDGE_CURVE('',#7471,#7469,#3824,.T.);
#9287=EDGE_CURVE('',#7472,#7473,#4525,.T.);
#9288=EDGE_CURVE('',#7472,#7470,#3825,.T.);
#9289=EDGE_CURVE('',#7473,#7471,#3826,.T.);
#9290=EDGE_CURVE('',#7474,#7475,#4526,.T.);
#9291=EDGE_CURVE('',#7474,#7472,#3827,.T.);
#9292=EDGE_CURVE('',#7475,#7473,#3828,.T.);
#9293=EDGE_CURVE('',#7476,#7477,#4527,.T.);
#9294=EDGE_CURVE('',#7476,#7474,#3829,.T.);
#9295=EDGE_CURVE('',#7477,#7475,#3830,.T.);
#9296=EDGE_CURVE('',#7478,#7479,#4528,.T.);
#9297=EDGE_CURVE('',#7478,#7476,#3831,.T.);
#9298=EDGE_CURVE('',#7479,#7477,#3832,.T.);
#9299=EDGE_CURVE('',#7480,#7481,#4529,.T.);
#9300=EDGE_CURVE('',#7480,#7478,#3833,.T.);
#9301=EDGE_CURVE('',#7481,#7479,#3834,.T.);
#9302=EDGE_CURVE('',#7482,#7483,#4530,.T.);
#9303=EDGE_CURVE('',#7482,#7480,#3835,.T.);
#9304=EDGE_CURVE('',#7483,#7481,#3836,.T.);
#9305=EDGE_CURVE('',#7484,#7485,#4531,.T.);
#9306=EDGE_CURVE('',#7484,#7482,#3837,.T.);
#9307=EDGE_CURVE('',#7485,#7483,#3838,.T.);
#9308=EDGE_CURVE('',#7486,#7486,#3325,.T.);
#9309=EDGE_CURVE('',#7486,#7487,#4532,.T.);
#9310=EDGE_CURVE('',#7487,#7488,#3326,.T.);
#9311=EDGE_CURVE('',#7488,#7487,#3327,.T.);
#9312=EDGE_CURVE('',#7488,#7489,#4533,.T.);
#9313=EDGE_CURVE('',#7489,#7489,#3328,.T.);
#9314=EDGE_CURVE('',#7490,#7490,#3329,.T.);
#9315=EDGE_CURVE('',#7491,#7492,#4534,.T.);
#9316=EDGE_CURVE('',#7492,#7493,#4535,.T.);
#9317=EDGE_CURVE('',#7493,#7494,#4536,.F.);
#9318=EDGE_CURVE('',#7494,#7495,#4537,.T.);
#9319=EDGE_CURVE('',#7495,#7491,#4538,.T.);
#9320=EDGE_CURVE('',#7496,#7492,#4539,.T.);
#9321=EDGE_CURVE('',#7496,#7497,#4540,.T.);
#9322=EDGE_CURVE('',#7493,#7497,#4541,.T.);
#9323=EDGE_CURVE('',#7498,#7491,#4542,.T.);
#9324=EDGE_CURVE('',#7498,#7499,#4543,.T.);
#9325=EDGE_CURVE('',#7499,#7496,#4544,.T.);
#9326=EDGE_CURVE('',#7495,#7500,#4545,.T.);
#9327=EDGE_CURVE('',#7501,#7500,#4546,.T.);
#9328=EDGE_CURVE('',#7501,#7498,#4547,.T.);
#9329=EDGE_CURVE('',#7502,#7503,#4548,.T.);
#9330=EDGE_CURVE('',#7503,#7504,#4549,.T.);
#9331=EDGE_CURVE('',#7504,#7505,#4550,.F.);
#9332=EDGE_CURVE('',#7505,#7506,#4551,.T.);
#9333=EDGE_CURVE('',#7506,#7502,#4552,.T.);
#9334=EDGE_CURVE('',#7507,#7503,#4553,.T.);
#9335=EDGE_CURVE('',#7507,#7508,#4554,.T.);
#9336=EDGE_CURVE('',#7504,#7508,#4555,.T.);
#9337=EDGE_CURVE('',#7509,#7502,#4556,.T.);
#9338=EDGE_CURVE('',#7509,#7510,#4557,.T.);
#9339=EDGE_CURVE('',#7510,#7507,#4558,.T.);
#9340=EDGE_CURVE('',#7506,#7496,#4559,.T.);
#9341=EDGE_CURVE('',#7499,#7509,#4560,.T.);
#9342=EDGE_CURVE('',#7511,#7512,#4561,.T.);
#9343=EDGE_CURVE('',#7512,#7513,#4562,.T.);
#9344=EDGE_CURVE('',#7513,#7514,#4563,.F.);
#9345=EDGE_CURVE('',#7514,#7515,#4564,.T.);
#9346=EDGE_CURVE('',#7515,#7511,#4565,.T.);
#9347=EDGE_CURVE('',#7516,#7512,#4566,.T.);
#9348=EDGE_CURVE('',#7516,#7517,#4567,.T.);
#9349=EDGE_CURVE('',#7513,#7517,#4568,.T.);
#9350=EDGE_CURVE('',#7518,#7511,#4569,.T.);
#9351=EDGE_CURVE('',#7518,#7519,#4570,.T.);
#9352=EDGE_CURVE('',#7519,#7516,#4571,.T.);
#9353=EDGE_CURVE('',#7515,#7507,#4572,.T.);
#9354=EDGE_CURVE('',#7510,#7518,#4573,.T.);
#9355=EDGE_CURVE('',#7520,#7521,#4574,.T.);
#9356=EDGE_CURVE('',#7521,#7522,#4575,.T.);
#9357=EDGE_CURVE('',#7522,#7523,#4576,.F.);
#9358=EDGE_CURVE('',#7523,#7524,#4577,.T.);
#9359=EDGE_CURVE('',#7524,#7520,#4578,.T.);
#9360=EDGE_CURVE('',#7525,#7521,#4579,.T.);
#9361=EDGE_CURVE('',#7525,#7526,#4580,.T.);
#9362=EDGE_CURVE('',#7522,#7526,#4581,.T.);
#9363=EDGE_CURVE('',#7527,#7520,#4582,.T.);
#9364=EDGE_CURVE('',#7527,#7528,#4583,.T.);
#9365=EDGE_CURVE('',#7528,#7525,#4584,.T.);
#9366=EDGE_CURVE('',#7524,#7516,#4585,.T.);
#9367=EDGE_CURVE('',#7519,#7527,#4586,.T.);
#9368=EDGE_CURVE('',#7529,#7530,#4587,.T.);
#9369=EDGE_CURVE('',#7530,#7531,#4588,.T.);
#9370=EDGE_CURVE('',#7531,#7532,#4589,.F.);
#9371=EDGE_CURVE('',#7532,#7533,#4590,.T.);
#9372=EDGE_CURVE('',#7533,#7529,#4591,.T.);
#9373=EDGE_CURVE('',#7534,#7530,#4592,.T.);
#9374=EDGE_CURVE('',#7534,#7535,#4593,.T.);
#9375=EDGE_CURVE('',#7531,#7535,#4594,.T.);
#9376=EDGE_CURVE('',#7536,#7529,#4595,.T.);
#9377=EDGE_CURVE('',#7536,#7537,#4596,.T.);
#9378=EDGE_CURVE('',#7537,#7534,#4597,.T.);
#9379=EDGE_CURVE('',#7533,#7525,#4598,.T.);
#9380=EDGE_CURVE('',#7528,#7536,#4599,.T.);
#9381=EDGE_CURVE('',#7538,#7539,#4600,.T.);
#9382=EDGE_CURVE('',#7539,#7540,#4601,.T.);
#9383=EDGE_CURVE('',#7540,#7541,#4602,.F.);
#9384=EDGE_CURVE('',#7541,#7542,#4603,.T.);
#9385=EDGE_CURVE('',#7542,#7538,#4604,.T.);
#9386=EDGE_CURVE('',#7500,#7539,#4605,.T.);
#9387=EDGE_CURVE('',#7500,#7543,#4606,.T.);
#9388=EDGE_CURVE('',#7540,#7543,#4607,.T.);
#9389=EDGE_CURVE('',#7544,#7538,#4608,.T.);
#9390=EDGE_CURVE('',#7544,#7501,#4609,.T.);
#9391=EDGE_CURVE('',#7542,#7545,#4610,.T.);
#9392=EDGE_CURVE('',#7545,#7546,#4611,.T.);
#9393=EDGE_CURVE('',#7546,#7544,#4612,.T.);
#9394=EDGE_CURVE('',#7547,#7548,#4613,.T.);
#9395=EDGE_CURVE('',#7548,#7549,#4614,.T.);
#9396=EDGE_CURVE('',#7549,#7550,#4615,.F.);
#9397=EDGE_CURVE('',#7550,#7551,#4616,.T.);
#9398=EDGE_CURVE('',#7551,#7547,#4617,.T.);
#9399=EDGE_CURVE('',#7545,#7548,#4618,.T.);
#9400=EDGE_CURVE('',#7545,#7552,#4619,.T.);
#9401=EDGE_CURVE('',#7549,#7552,#4620,.T.);
#9402=EDGE_CURVE('',#7553,#7547,#4621,.T.);
#9403=EDGE_CURVE('',#7553,#7546,#4622,.T.);
#9404=EDGE_CURVE('',#7554,#7555,#4623,.T.);
#9405=EDGE_CURVE('',#7555,#7556,#4624,.T.);
#9406=EDGE_CURVE('',#7556,#7557,#4625,.F.);
#9407=EDGE_CURVE('',#7557,#7558,#4626,.T.);
#9408=EDGE_CURVE('',#7558,#7554,#4627,.T.);
#9409=EDGE_CURVE('',#7559,#7555,#4628,.T.);
#9410=EDGE_CURVE('',#7559,#7560,#4629,.T.);
#9411=EDGE_CURVE('',#7556,#7560,#4630,.T.);
#9412=EDGE_CURVE('',#7561,#7554,#4631,.T.);
#9413=EDGE_CURVE('',#7561,#7562,#4632,.T.);
#9414=EDGE_CURVE('',#7562,#7559,#4633,.T.);
#9415=EDGE_CURVE('',#7558,#7563,#4634,.T.);
#9416=EDGE_CURVE('',#7564,#7563,#4635,.T.);
#9417=EDGE_CURVE('',#7564,#7561,#4636,.T.);
#9418=EDGE_CURVE('',#7565,#7566,#4637,.T.);
#9419=EDGE_CURVE('',#7566,#7567,#4638,.T.);
#9420=EDGE_CURVE('',#7567,#7568,#4639,.F.);
#9421=EDGE_CURVE('',#7568,#7569,#4640,.T.);
#9422=EDGE_CURVE('',#7569,#7565,#4641,.T.);
#9423=EDGE_CURVE('',#7563,#7566,#4642,.T.);
#9424=EDGE_CURVE('',#7563,#7570,#4643,.T.);
#9425=EDGE_CURVE('',#7567,#7570,#4644,.T.);
#9426=EDGE_CURVE('',#7571,#7565,#4645,.T.);
#9427=EDGE_CURVE('',#7571,#7564,#4646,.T.);
#9428=EDGE_CURVE('',#7569,#7572,#4647,.T.);
#9429=EDGE_CURVE('',#7573,#7572,#4648,.T.);
#9430=EDGE_CURVE('',#7573,#7571,#4649,.T.);
#9431=EDGE_CURVE('',#7574,#7575,#4650,.T.);
#9432=EDGE_CURVE('',#7575,#7576,#4651,.T.);
#9433=EDGE_CURVE('',#7576,#7577,#4652,.F.);
#9434=EDGE_CURVE('',#7577,#7578,#4653,.T.);
#9435=EDGE_CURVE('',#7578,#7574,#4654,.T.);
#9436=EDGE_CURVE('',#7572,#7575,#4655,.T.);
#9437=EDGE_CURVE('',#7572,#7579,#4656,.T.);
#9438=EDGE_CURVE('',#7576,#7579,#4657,.T.);
#9439=EDGE_CURVE('',#7580,#7574,#4658,.T.);
#9440=EDGE_CURVE('',#7580,#7573,#4659,.T.);
#9441=EDGE_CURVE('',#7578,#7581,#4660,.T.);
#9442=EDGE_CURVE('',#7582,#7581,#4661,.T.);
#9443=EDGE_CURVE('',#7582,#7580,#4662,.T.);
#9444=EDGE_CURVE('',#7583,#7584,#4663,.T.);
#9445=EDGE_CURVE('',#7584,#7585,#4664,.T.);
#9446=EDGE_CURVE('',#7585,#7586,#4665,.F.);
#9447=EDGE_CURVE('',#7586,#7587,#4666,.T.);
#9448=EDGE_CURVE('',#7587,#7583,#4667,.T.);
#9449=EDGE_CURVE('',#7581,#7584,#4668,.T.);
#9450=EDGE_CURVE('',#7581,#7588,#4669,.T.);
#9451=EDGE_CURVE('',#7585,#7588,#4670,.T.);
#9452=EDGE_CURVE('',#7589,#7583,#4671,.T.);
#9453=EDGE_CURVE('',#7589,#7582,#4672,.T.);
#9454=EDGE_CURVE('',#7587,#7590,#4673,.T.);
#9455=EDGE_CURVE('',#7591,#7590,#4674,.T.);
#9456=EDGE_CURVE('',#7591,#7589,#4675,.T.);
#9457=EDGE_CURVE('',#7592,#7593,#4676,.T.);
#9458=EDGE_CURVE('',#7593,#7594,#4677,.T.);
#9459=EDGE_CURVE('',#7594,#7595,#4678,.F.);
#9460=EDGE_CURVE('',#7595,#7596,#4679,.T.);
#9461=EDGE_CURVE('',#7596,#7592,#4680,.T.);
#9462=EDGE_CURVE('',#7590,#7593,#4681,.T.);
#9463=EDGE_CURVE('',#7590,#7597,#4682,.T.);
#9464=EDGE_CURVE('',#7594,#7597,#4683,.T.);
#9465=EDGE_CURVE('',#7598,#7592,#4684,.T.);
#9466=EDGE_CURVE('',#7598,#7591,#4685,.T.);
#9467=EDGE_CURVE('',#7596,#7534,#4686,.T.);
#9468=EDGE_CURVE('',#7537,#7598,#4687,.T.);
#9469=EDGE_CURVE('',#7599,#7600,#3839,.T.);
#9470=EDGE_CURVE('',#7600,#7601,#3330,.T.);
#9471=EDGE_CURVE('',#7601,#7602,#3840,.T.);
#9472=EDGE_CURVE('',#7602,#7599,#3331,.T.);
#9473=EDGE_CURVE('',#7602,#7603,#3841,.T.);
#9474=EDGE_CURVE('',#7603,#7604,#3332,.T.);
#9475=EDGE_CURVE('',#7604,#7599,#3842,.T.);
#9476=EDGE_CURVE('',#7605,#7601,#3843,.T.);
#9477=EDGE_CURVE('',#7606,#7605,#3844,.T.);
#9478=EDGE_CURVE('',#7607,#7606,#3845,.T.);
#9479=EDGE_CURVE('',#7359,#7607,#3846,.T.);
#9480=EDGE_CURVE('',#7608,#7451,#3847,.T.);
#9481=EDGE_CURVE('',#7609,#7608,#3848,.T.);
#9482=EDGE_CURVE('',#7603,#7609,#3849,.T.);
#9483=EDGE_CURVE('',#7610,#7611,#3850,.T.);
#9484=EDGE_CURVE('',#7611,#7612,#3333,.T.);
#9485=EDGE_CURVE('',#7612,#7613,#3851,.T.);
#9486=EDGE_CURVE('',#7613,#7610,#3334,.T.);
#9487=EDGE_CURVE('',#7613,#7614,#3852,.T.);
#9488=EDGE_CURVE('',#7614,#7615,#3335,.T.);
#9489=EDGE_CURVE('',#7615,#7610,#3853,.T.);
#9490=EDGE_CURVE('',#7616,#7612,#3854,.T.);
#9491=EDGE_CURVE('',#7617,#7616,#3855,.T.);
#9492=EDGE_CURVE('',#7444,#7617,#3856,.T.);
#9493=EDGE_CURVE('',#7618,#7443,#3857,.T.);
#9494=EDGE_CURVE('',#7619,#7618,#3858,.T.);
#9495=EDGE_CURVE('',#7614,#7619,#3859,.T.);
#9496=EDGE_CURVE('',#7620,#7621,#3860,.T.);
#9497=EDGE_CURVE('',#7621,#7622,#3336,.T.);
#9498=EDGE_CURVE('',#7622,#7623,#3861,.T.);
#9499=EDGE_CURVE('',#7623,#7620,#3337,.T.);
#9500=EDGE_CURVE('',#7623,#7624,#3862,.T.);
#9501=EDGE_CURVE('',#7624,#7625,#3338,.T.);
#9502=EDGE_CURVE('',#7625,#7620,#3863,.T.);
#9503=EDGE_CURVE('',#7626,#7622,#3864,.T.);
#9504=EDGE_CURVE('',#7627,#7626,#3865,.T.);
#9505=EDGE_CURVE('',#7436,#7627,#3866,.T.);
#9506=EDGE_CURVE('',#7628,#7435,#3867,.T.);
#9507=EDGE_CURVE('',#7629,#7628,#3868,.T.);
#9508=EDGE_CURVE('',#7624,#7629,#3869,.T.);
#9509=EDGE_CURVE('',#7630,#7631,#3870,.T.);
#9510=EDGE_CURVE('',#7631,#7632,#3339,.T.);
#9511=EDGE_CURVE('',#7632,#7633,#3871,.T.);
#9512=EDGE_CURVE('',#7633,#7630,#3340,.T.);
#9513=EDGE_CURVE('',#7633,#7634,#3872,.T.);
#9514=EDGE_CURVE('',#7634,#7635,#3341,.T.);
#9515=EDGE_CURVE('',#7635,#7630,#3873,.T.);
#9516=EDGE_CURVE('',#7636,#7632,#3874,.T.);
#9517=EDGE_CURVE('',#7637,#7636,#3875,.T.);
#9518=EDGE_CURVE('',#7428,#7637,#3876,.T.);
#9519=EDGE_CURVE('',#7638,#7427,#3877,.T.);
#9520=EDGE_CURVE('',#7639,#7638,#3878,.T.);
#9521=EDGE_CURVE('',#7634,#7639,#3879,.T.);
#9522=EDGE_CURVE('',#7640,#7641,#3880,.T.);
#9523=EDGE_CURVE('',#7641,#7642,#3342,.T.);
#9524=EDGE_CURVE('',#7642,#7643,#3881,.T.);
#9525=EDGE_CURVE('',#7643,#7640,#3343,.T.);
#9526=EDGE_CURVE('',#7643,#7644,#3882,.T.);
#9527=EDGE_CURVE('',#7644,#7645,#3344,.T.);
#9528=EDGE_CURVE('',#7645,#7640,#3883,.T.);
#9529=EDGE_CURVE('',#7646,#7642,#3884,.T.);
#9530=EDGE_CURVE('',#7647,#7646,#3885,.T.);
#9531=EDGE_CURVE('',#7420,#7647,#3886,.T.);
#9532=EDGE_CURVE('',#7648,#7419,#3887,.T.);
#9533=EDGE_CURVE('',#7649,#7648,#3888,.T.);
#9534=EDGE_CURVE('',#7644,#7649,#3889,.T.);
#9535=EDGE_CURVE('',#7650,#7651,#3890,.T.);
#9536=EDGE_CURVE('',#7651,#7652,#3345,.T.);
#9537=EDGE_CURVE('',#7652,#7653,#3891,.T.);
#9538=EDGE_CURVE('',#7653,#7650,#3346,.T.);
#9539=EDGE_CURVE('',#7653,#7654,#3892,.T.);
#9540=EDGE_CURVE('',#7654,#7655,#3347,.T.);
#9541=EDGE_CURVE('',#7655,#7650,#3893,.T.);
#9542=EDGE_CURVE('',#7656,#7652,#3894,.T.);
#9543=EDGE_CURVE('',#7657,#7656,#3895,.T.);
#9544=EDGE_CURVE('',#7412,#7657,#3896,.T.);
#9545=EDGE_CURVE('',#7658,#7411,#3897,.T.);
#9546=EDGE_CURVE('',#7659,#7658,#3898,.T.);
#9547=EDGE_CURVE('',#7654,#7659,#3899,.T.);
#9548=EDGE_CURVE('',#7660,#7661,#3900,.T.);
#9549=EDGE_CURVE('',#7661,#7662,#3348,.T.);
#9550=EDGE_CURVE('',#7662,#7663,#3901,.T.);
#9551=EDGE_CURVE('',#7663,#7660,#3349,.T.);
#9552=EDGE_CURVE('',#7663,#7664,#3902,.T.);
#9553=EDGE_CURVE('',#7664,#7665,#3350,.T.);
#9554=EDGE_CURVE('',#7665,#7660,#3903,.T.);
#9555=EDGE_CURVE('',#7666,#7662,#3904,.T.);
#9556=EDGE_CURVE('',#7667,#7666,#3905,.T.);
#9557=EDGE_CURVE('',#7404,#7667,#3906,.T.);
#9558=EDGE_CURVE('',#7668,#7403,#3907,.T.);
#9559=EDGE_CURVE('',#7669,#7668,#3908,.T.);
#9560=EDGE_CURVE('',#7664,#7669,#3909,.T.);
#9561=EDGE_CURVE('',#7670,#7671,#3910,.T.);
#9562=EDGE_CURVE('',#7671,#7672,#3351,.T.);
#9563=EDGE_CURVE('',#7672,#7673,#3911,.T.);
#9564=EDGE_CURVE('',#7673,#7670,#3352,.T.);
#9565=EDGE_CURVE('',#7673,#7674,#3912,.T.);
#9566=EDGE_CURVE('',#7674,#7675,#3353,.T.);
#9567=EDGE_CURVE('',#7675,#7670,#3913,.T.);
#9568=EDGE_CURVE('',#7676,#7672,#3914,.T.);
#9569=EDGE_CURVE('',#7677,#7676,#3915,.T.);
#9570=EDGE_CURVE('',#7396,#7677,#3916,.T.);
#9571=EDGE_CURVE('',#7678,#7395,#3917,.T.);
#9572=EDGE_CURVE('',#7679,#7678,#3918,.T.);
#9573=EDGE_CURVE('',#7674,#7679,#3919,.T.);
#9574=EDGE_CURVE('',#7680,#7681,#3920,.T.);
#9575=EDGE_CURVE('',#7681,#7682,#3354,.T.);
#9576=EDGE_CURVE('',#7682,#7683,#3921,.T.);
#9577=EDGE_CURVE('',#7683,#7680,#3355,.T.);
#9578=EDGE_CURVE('',#7683,#7684,#3922,.T.);
#9579=EDGE_CURVE('',#7684,#7685,#3356,.T.);
#9580=EDGE_CURVE('',#7685,#7680,#3923,.T.);
#9581=EDGE_CURVE('',#7686,#7682,#3924,.T.);
#9582=EDGE_CURVE('',#7687,#7686,#3925,.T.);
#9583=EDGE_CURVE('',#7388,#7687,#3926,.T.);
#9584=EDGE_CURVE('',#7688,#7387,#3927,.T.);
#9585=EDGE_CURVE('',#7689,#7688,#3928,.T.);
#9586=EDGE_CURVE('',#7684,#7689,#3929,.T.);
#9587=EDGE_CURVE('',#7690,#7691,#3930,.T.);
#9588=EDGE_CURVE('',#7691,#7692,#3357,.T.);
#9589=EDGE_CURVE('',#7692,#7693,#3931,.T.);
#9590=EDGE_CURVE('',#7693,#7690,#3358,.T.);
#9591=EDGE_CURVE('',#7693,#7694,#3932,.T.);
#9592=EDGE_CURVE('',#7694,#7695,#3359,.T.);
#9593=EDGE_CURVE('',#7695,#7690,#3933,.T.);
#9594=EDGE_CURVE('',#7696,#7692,#3934,.T.);
#9595=EDGE_CURVE('',#7697,#7696,#3935,.T.);
#9596=EDGE_CURVE('',#7380,#7697,#3936,.T.);
#9597=EDGE_CURVE('',#7698,#7379,#3937,.T.);
#9598=EDGE_CURVE('',#7699,#7698,#3938,.T.);
#9599=EDGE_CURVE('',#7694,#7699,#3939,.T.);
#9600=EDGE_CURVE('',#7700,#7701,#3940,.T.);
#9601=EDGE_CURVE('',#7701,#7702,#3360,.T.);
#9602=EDGE_CURVE('',#7702,#7703,#3941,.T.);
#9603=EDGE_CURVE('',#7703,#7700,#3361,.T.);
#9604=EDGE_CURVE('',#7703,#7704,#3942,.T.);
#9605=EDGE_CURVE('',#7704,#7705,#3362,.T.);
#9606=EDGE_CURVE('',#7705,#7700,#3943,.T.);
#9607=EDGE_CURVE('',#7706,#7702,#3944,.T.);
#9608=EDGE_CURVE('',#7707,#7706,#3945,.T.);
#9609=EDGE_CURVE('',#7372,#7707,#3946,.T.);
#9610=EDGE_CURVE('',#7708,#7371,#3947,.T.);
#9611=EDGE_CURVE('',#7709,#7708,#3948,.T.);
#9612=EDGE_CURVE('',#7704,#7709,#3949,.T.);
#9613=EDGE_CURVE('',#7710,#7711,#3950,.T.);
#9614=EDGE_CURVE('',#7711,#7712,#3363,.T.);
#9615=EDGE_CURVE('',#7712,#7713,#3951,.T.);
#9616=EDGE_CURVE('',#7713,#7710,#3364,.T.);
#9617=EDGE_CURVE('',#7713,#7714,#3952,.T.);
#9618=EDGE_CURVE('',#7714,#7715,#3365,.T.);
#9619=EDGE_CURVE('',#7715,#7710,#3953,.T.);
#9620=EDGE_CURVE('',#7716,#7712,#3954,.T.);
#9621=EDGE_CURVE('',#7717,#7716,#3955,.T.);
#9622=EDGE_CURVE('',#7364,#7717,#3956,.T.);
#9623=EDGE_CURVE('',#7718,#7361,#3957,.T.);
#9624=EDGE_CURVE('',#7719,#7718,#3958,.T.);
#9625=EDGE_CURVE('',#7714,#7719,#3959,.T.);
#9626=EDGE_CURVE('',#7720,#7720,#3366,.T.);
#9627=EDGE_CURVE('',#7720,#7721,#4688,.T.);
#9628=EDGE_CURVE('',#7721,#7721,#3367,.T.);
#9629=EDGE_CURVE('',#7722,#7722,#3368,.T.);
#9630=EDGE_CURVE('',#7723,#7723,#3369,.T.);
#9631=EDGE_CURVE('',#7723,#7720,#4689,.T.);
#9632=EDGE_CURVE('',#7724,#7724,#3370,.T.);
#9633=EDGE_CURVE('',#7724,#7725,#4690,.T.);
#9634=EDGE_CURVE('',#7725,#7725,#3371,.T.);
#9635=EDGE_CURVE('',#7726,#7726,#3372,.T.);
#9636=EDGE_CURVE('',#7724,#7727,#4691,.T.);
#9637=EDGE_CURVE('',#7727,#7727,#3373,.T.);
#9638=EDGE_CURVE('',#7728,#7729,#978,.T.);
#9639=EDGE_CURVE('',#7729,#7730,#4692,.T.);
#9640=EDGE_CURVE('',#7730,#7731,#979,.T.);
#9641=EDGE_CURVE('',#7731,#7732,#980,.T.);
#9642=EDGE_CURVE('',#7732,#7728,#4693,.T.);
#9643=EDGE_CURVE('',#7731,#7733,#3960,.T.);
#9644=EDGE_CURVE('',#7733,#7734,#3374,.T.);
#9645=EDGE_CURVE('',#7734,#7735,#3961,.T.);
#9646=EDGE_CURVE('',#7735,#7736,#981,.T.);
#9647=EDGE_CURVE('',#7736,#7732,#3375,.T.);
#9648=EDGE_CURVE('',#7730,#7737,#3376,.T.);
#9649=EDGE_CURVE('',#7738,#7737,#982,.T.);
#9650=EDGE_CURVE('',#7739,#7738,#3962,.T.);
#9651=EDGE_CURVE('',#7733,#7739,#3377,.T.);
#9652=EDGE_CURVE('',#7729,#7617,#3378,.T.);
#9653=EDGE_CURVE('',#7616,#7740,#3379,.T.);
#9654=EDGE_CURVE('',#7740,#7741,#3963,.T.);
#9655=EDGE_CURVE('',#7741,#7742,#3380,.T.);
#9656=EDGE_CURVE('',#7737,#7742,#4694,.T.);
#9657=EDGE_CURVE('',#7742,#7743,#983,.T.);
#9658=EDGE_CURVE('',#7743,#7744,#4695,.T.);
#9659=EDGE_CURVE('',#7744,#7738,#984,.T.);
#9660=EDGE_CURVE('',#7744,#7745,#3381,.T.);
#9661=EDGE_CURVE('',#7746,#7745,#985,.T.);
#9662=EDGE_CURVE('',#7746,#7747,#3964,.T.);
#9663=EDGE_CURVE('',#7747,#7739,#3382,.T.);
#9664=EDGE_CURVE('',#7748,#7749,#986,.T.);
#9665=EDGE_CURVE('',#7749,#7750,#4696,.T.);
#9666=EDGE_CURVE('',#7750,#7746,#987,.T.);
#9667=EDGE_CURVE('',#7745,#7748,#4697,.T.);
#9668=EDGE_CURVE('',#7750,#7751,#3383,.T.);
#9669=EDGE_CURVE('',#7752,#7751,#988,.T.);
#9670=EDGE_CURVE('',#7753,#7752,#3965,.T.);
#9671=EDGE_CURVE('',#7747,#7753,#3384,.T.);
#9672=EDGE_CURVE('',#7749,#7627,#3385,.T.);
#9673=EDGE_CURVE('',#7626,#7754,#3386,.T.);
#9674=EDGE_CURVE('',#7754,#7755,#3966,.T.);
#9675=EDGE_CURVE('',#7755,#7756,#3387,.T.);
#9676=EDGE_CURVE('',#7751,#7756,#4698,.T.);
#9677=EDGE_CURVE('',#7756,#7757,#989,.T.);
#9678=EDGE_CURVE('',#7757,#7758,#4699,.T.);
#9679=EDGE_CURVE('',#7758,#7752,#990,.T.);
#9680=EDGE_CURVE('',#7758,#7759,#3388,.T.);
#9681=EDGE_CURVE('',#7760,#7759,#991,.T.);
#9682=EDGE_CURVE('',#7760,#7761,#3967,.T.);
#9683=EDGE_CURVE('',#7761,#7753,#3389,.T.);
#9684=EDGE_CURVE('',#7762,#7763,#992,.T.);
#9685=EDGE_CURVE('',#7763,#7764,#4700,.T.);
#9686=EDGE_CURVE('',#7764,#7760,#993,.T.);
#9687=EDGE_CURVE('',#7759,#7762,#4701,.T.);
#9688=EDGE_CURVE('',#7764,#7765,#3390,.T.);
#9689=EDGE_CURVE('',#7766,#7765,#994,.T.);
#9690=EDGE_CURVE('',#7767,#7766,#3968,.T.);
#9691=EDGE_CURVE('',#7761,#7767,#3391,.T.);
#9692=EDGE_CURVE('',#7763,#7637,#3392,.T.);
#9693=EDGE_CURVE('',#7636,#7768,#3393,.T.);
#9694=EDGE_CURVE('',#7768,#7769,#3969,.T.);
#9695=EDGE_CURVE('',#7769,#7770,#3394,.T.);
#9696=EDGE_CURVE('',#7765,#7770,#4702,.T.);
#9697=EDGE_CURVE('',#7770,#7771,#995,.T.);
#9698=EDGE_CURVE('',#7771,#7772,#4703,.T.);
#9699=EDGE_CURVE('',#7772,#7766,#996,.T.);
#9700=EDGE_CURVE('',#7772,#7773,#3395,.T.);
#9701=EDGE_CURVE('',#7774,#7773,#997,.T.);
#9702=EDGE_CURVE('',#7774,#7775,#3970,.T.);
#9703=EDGE_CURVE('',#7775,#7767,#3396,.T.);
#9704=EDGE_CURVE('',#7776,#7777,#998,.T.);
#9705=EDGE_CURVE('',#7777,#7778,#4704,.T.);
#9706=EDGE_CURVE('',#7778,#7774,#999,.T.);
#9707=EDGE_CURVE('',#7773,#7776,#4705,.T.);
#9708=EDGE_CURVE('',#7778,#7779,#3397,.T.);
#9709=EDGE_CURVE('',#7780,#7779,#1000,.T.);
#9710=EDGE_CURVE('',#7781,#7780,#3971,.T.);
#9711=EDGE_CURVE('',#7775,#7781,#3398,.T.);
#9712=EDGE_CURVE('',#7777,#7647,#3399,.T.);
#9713=EDGE_CURVE('',#7646,#7782,#3400,.T.);
#9714=EDGE_CURVE('',#7782,#7783,#3972,.T.);
#9715=EDGE_CURVE('',#7783,#7784,#3401,.T.);
#9716=EDGE_CURVE('',#7779,#7784,#4706,.T.);
#9717=EDGE_CURVE('',#7784,#7785,#1001,.T.);
#9718=EDGE_CURVE('',#7785,#7786,#4707,.T.);
#9719=EDGE_CURVE('',#7786,#7780,#1002,.T.);
#9720=EDGE_CURVE('',#7786,#7787,#3402,.T.);
#9721=EDGE_CURVE('',#7788,#7787,#1003,.T.);
#9722=EDGE_CURVE('',#7788,#7789,#3973,.T.);
#9723=EDGE_CURVE('',#7789,#7781,#3403,.T.);
#9724=EDGE_CURVE('',#7790,#7791,#1004,.T.);
#9725=EDGE_CURVE('',#7791,#7792,#4708,.T.);
#9726=EDGE_CURVE('',#7792,#7788,#1005,.T.);
#9727=EDGE_CURVE('',#7787,#7790,#4709,.T.);
#9728=EDGE_CURVE('',#7792,#7793,#3404,.T.);
#9729=EDGE_CURVE('',#7794,#7793,#1006,.T.);
#9730=EDGE_CURVE('',#7795,#7794,#3974,.T.);
#9731=EDGE_CURVE('',#7789,#7795,#3405,.T.);
#9732=EDGE_CURVE('',#7791,#7657,#3406,.T.);
#9733=EDGE_CURVE('',#7656,#7796,#3407,.T.);
#9734=EDGE_CURVE('',#7796,#7797,#3975,.T.);
#9735=EDGE_CURVE('',#7797,#7798,#3408,.T.);
#9736=EDGE_CURVE('',#7793,#7798,#4710,.T.);
#9737=EDGE_CURVE('',#7798,#7799,#1007,.T.);
#9738=EDGE_CURVE('',#7799,#7800,#4711,.T.);
#9739=EDGE_CURVE('',#7800,#7794,#1008,.T.);
#9740=EDGE_CURVE('',#7800,#7801,#3409,.T.);
#9741=EDGE_CURVE('',#7801,#7802,#1009,.T.);
#9742=EDGE_CURVE('',#7802,#7803,#3976,.T.);
#9743=EDGE_CURVE('',#7803,#7795,#3410,.T.);
#9744=EDGE_CURVE('',#7803,#7804,#3411,.T.);
#9745=EDGE_CURVE('',#7805,#7804,#3412,.T.);
#9746=EDGE_CURVE('',#7805,#7806,#3413,.T.);
#9747=EDGE_CURVE('',#7807,#7806,#3414,.T.);
#9748=EDGE_CURVE('',#7807,#7808,#3415,.T.);
#9749=EDGE_CURVE('',#7809,#7808,#3416,.T.);
#9750=EDGE_CURVE('',#7809,#7810,#3417,.T.);
#9751=EDGE_CURVE('',#7811,#7810,#3418,.T.);
#9752=EDGE_CURVE('',#7811,#7812,#3419,.T.);
#9753=EDGE_CURVE('',#7813,#7812,#3420,.T.);
#9754=EDGE_CURVE('',#7813,#7814,#3421,.T.);
#9755=EDGE_CURVE('',#7815,#7814,#3422,.T.);
#9756=EDGE_CURVE('',#7815,#7734,#3423,.T.);
#9757=EDGE_CURVE('',#7816,#7816,#3424,.T.);
#9758=EDGE_CURVE('',#7817,#7802,#1010,.T.);
#9759=EDGE_CURVE('',#7817,#7818,#3425,.T.);
#9760=EDGE_CURVE('',#7819,#7818,#1011,.T.);
#9761=EDGE_CURVE('',#7804,#7819,#3977,.T.);
#9762=EDGE_CURVE('',#7801,#7820,#4712,.T.);
#9763=EDGE_CURVE('',#7820,#7821,#1012,.T.);
#9764=EDGE_CURVE('',#7821,#7817,#4713,.T.);
#9765=EDGE_CURVE('',#7440,#7743,#3978,.T.);
#9766=EDGE_CURVE('',#7438,#7439,#3426,.T.);
#9767=EDGE_CURVE('',#7748,#7437,#3979,.T.);
#9768=EDGE_CURVE('',#7822,#7736,#4714,.T.);
#9769=EDGE_CURVE('',#7448,#7822,#3980,.T.);
#9770=EDGE_CURVE('',#7446,#7447,#3427,.T.);
#9771=EDGE_CURVE('',#7728,#7445,#3981,.T.);
#9772=EDGE_CURVE('',#7735,#7823,#1013,.T.);
#9773=EDGE_CURVE('',#7823,#7824,#4715,.T.);
#9774=EDGE_CURVE('',#7824,#7822,#1014,.T.);
#9775=EDGE_CURVE('',#7821,#7667,#3428,.T.);
#9776=EDGE_CURVE('',#7666,#7825,#3429,.T.);
#9777=EDGE_CURVE('',#7825,#7826,#3982,.T.);
#9778=EDGE_CURVE('',#7826,#7827,#3430,.T.);
#9779=EDGE_CURVE('',#7818,#7827,#4716,.T.);
#9780=EDGE_CURVE('',#7827,#7828,#1015,.T.);
#9781=EDGE_CURVE('',#7828,#7829,#4717,.T.);
#9782=EDGE_CURVE('',#7829,#7819,#1016,.T.);
#9783=EDGE_CURVE('',#7829,#7830,#3431,.T.);
#9784=EDGE_CURVE('',#7830,#7831,#1017,.T.);
#9785=EDGE_CURVE('',#7831,#7805,#3983,.T.);
#9786=EDGE_CURVE('',#7832,#7831,#1018,.T.);
#9787=EDGE_CURVE('',#7832,#7833,#3432,.T.);
#9788=EDGE_CURVE('',#7834,#7833,#1019,.T.);
#9789=EDGE_CURVE('',#7806,#7834,#3984,.T.);
#9790=EDGE_CURVE('',#7830,#7835,#4718,.T.);
#9791=EDGE_CURVE('',#7835,#7836,#1020,.T.);
#9792=EDGE_CURVE('',#7836,#7832,#4719,.T.);
#9793=EDGE_CURVE('',#7836,#7677,#3433,.T.);
#9794=EDGE_CURVE('',#7676,#7837,#3434,.T.);
#9795=EDGE_CURVE('',#7837,#7838,#3985,.T.);
#9796=EDGE_CURVE('',#7838,#7839,#3435,.T.);
#9797=EDGE_CURVE('',#7833,#7839,#4720,.T.);
#9798=EDGE_CURVE('',#7839,#7840,#1021,.T.);
#9799=EDGE_CURVE('',#7840,#7841,#4721,.T.);
#9800=EDGE_CURVE('',#7841,#7834,#1022,.T.);
#9801=EDGE_CURVE('',#7841,#7842,#3436,.T.);
#9802=EDGE_CURVE('',#7842,#7843,#1023,.T.);
#9803=EDGE_CURVE('',#7843,#7807,#3986,.T.);
#9804=EDGE_CURVE('',#7844,#7843,#1024,.T.);
#9805=EDGE_CURVE('',#7844,#7845,#3437,.T.);
#9806=EDGE_CURVE('',#7846,#7845,#1025,.T.);
#9807=EDGE_CURVE('',#7808,#7846,#3987,.T.);
#9808=EDGE_CURVE('',#7842,#7847,#4722,.T.);
#9809=EDGE_CURVE('',#7847,#7848,#1026,.T.);
#9810=EDGE_CURVE('',#7848,#7844,#4723,.T.);
#9811=EDGE_CURVE('',#7848,#7687,#3438,.T.);
#9812=EDGE_CURVE('',#7686,#7849,#3439,.T.);
#9813=EDGE_CURVE('',#7849,#7850,#3988,.T.);
#9814=EDGE_CURVE('',#7850,#7851,#3440,.T.);
#9815=EDGE_CURVE('',#7845,#7851,#4724,.T.);
#9816=EDGE_CURVE('',#7851,#7852,#1027,.T.);
#9817=EDGE_CURVE('',#7852,#7853,#4725,.T.);
#9818=EDGE_CURVE('',#7853,#7846,#1028,.T.);
#9819=EDGE_CURVE('',#7853,#7854,#3441,.T.);
#9820=EDGE_CURVE('',#7854,#7855,#1029,.T.);
#9821=EDGE_CURVE('',#7855,#7809,#3989,.T.);
#9822=EDGE_CURVE('',#7856,#7855,#1030,.T.);
#9823=EDGE_CURVE('',#7856,#7857,#3442,.T.);
#9824=EDGE_CURVE('',#7858,#7857,#1031,.T.);
#9825=EDGE_CURVE('',#7810,#7858,#3990,.T.);
#9826=EDGE_CURVE('',#7854,#7859,#4726,.T.);
#9827=EDGE_CURVE('',#7859,#7860,#1032,.T.);
#9828=EDGE_CURVE('',#7860,#7856,#4727,.T.);
#9829=EDGE_CURVE('',#7860,#7697,#3443,.T.);
#9830=EDGE_CURVE('',#7696,#7861,#3444,.T.);
#9831=EDGE_CURVE('',#7861,#7862,#3991,.T.);
#9832=EDGE_CURVE('',#7862,#7863,#3445,.T.);
#9833=EDGE_CURVE('',#7857,#7863,#4728,.T.);
#9834=EDGE_CURVE('',#7863,#7864,#1033,.T.);
#9835=EDGE_CURVE('',#7864,#7865,#4729,.T.);
#9836=EDGE_CURVE('',#7865,#7858,#1034,.T.);
#9837=EDGE_CURVE('',#7865,#7866,#3446,.T.);
#9838=EDGE_CURVE('',#7866,#7867,#1035,.T.);
#9839=EDGE_CURVE('',#7867,#7811,#3992,.T.);
#9840=EDGE_CURVE('',#7868,#7867,#1036,.T.);
#9841=EDGE_CURVE('',#7868,#7869,#3447,.T.);
#9842=EDGE_CURVE('',#7870,#7869,#1037,.T.);
#9843=EDGE_CURVE('',#7812,#7870,#3993,.T.);
#9844=EDGE_CURVE('',#7866,#7871,#4730,.T.);
#9845=EDGE_CURVE('',#7871,#7872,#1038,.T.);
#9846=EDGE_CURVE('',#7872,#7868,#4731,.T.);
#9847=EDGE_CURVE('',#7872,#7707,#3448,.T.);
#9848=EDGE_CURVE('',#7706,#7873,#3449,.T.);
#9849=EDGE_CURVE('',#7873,#7874,#3994,.T.);
#9850=EDGE_CURVE('',#7874,#7875,#3450,.T.);
#9851=EDGE_CURVE('',#7869,#7875,#4732,.T.);
#9852=EDGE_CURVE('',#7875,#7876,#1039,.T.);
#9853=EDGE_CURVE('',#7876,#7877,#4733,.T.);
#9854=EDGE_CURVE('',#7877,#7870,#1040,.T.);
#9855=EDGE_CURVE('',#7877,#7878,#3451,.T.);
#9856=EDGE_CURVE('',#7878,#7879,#1041,.T.);
#9857=EDGE_CURVE('',#7879,#7813,#3995,.T.);
#9858=EDGE_CURVE('',#7880,#7879,#1042,.T.);
#9859=EDGE_CURVE('',#7880,#7881,#3452,.T.);
#9860=EDGE_CURVE('',#7882,#7881,#1043,.T.);
#9861=EDGE_CURVE('',#7814,#7882,#3996,.T.);
#9862=EDGE_CURVE('',#7878,#7883,#4734,.T.);
#9863=EDGE_CURVE('',#7883,#7884,#1044,.T.);
#9864=EDGE_CURVE('',#7884,#7880,#4735,.T.);
#9865=EDGE_CURVE('',#7885,#7823,#3453,.T.);
#9866=EDGE_CURVE('',#7886,#7885,#4736,.T.);
#9867=EDGE_CURVE('',#7886,#7606,#3454,.T.);
#9868=EDGE_CURVE('',#7605,#7887,#3455,.T.);
#9869=EDGE_CURVE('',#7887,#7888,#3997,.T.);
#9870=EDGE_CURVE('',#7888,#7824,#3456,.T.);
#9871=EDGE_CURVE('',#7889,#7815,#3998,.T.);
#9872=EDGE_CURVE('',#7885,#7889,#1045,.T.);
#9873=EDGE_CURVE('',#7884,#7717,#3457,.T.);
#9874=EDGE_CURVE('',#7716,#7890,#3458,.T.);
#9875=EDGE_CURVE('',#7890,#7891,#3999,.T.);
#9876=EDGE_CURVE('',#7891,#7892,#3459,.T.);
#9877=EDGE_CURVE('',#7881,#7892,#4737,.T.);
#9878=EDGE_CURVE('',#7892,#7893,#1046,.T.);
#9879=EDGE_CURVE('',#7893,#7894,#4738,.T.);
#9880=EDGE_CURVE('',#7894,#7882,#1047,.T.);
#9881=EDGE_CURVE('',#7894,#7895,#3460,.T.);
#9882=EDGE_CURVE('',#7895,#7889,#1048,.T.);
#9883=EDGE_CURVE('',#7895,#7896,#4739,.T.);
#9884=EDGE_CURVE('',#7896,#7886,#1049,.T.);
#9885=EDGE_CURVE('',#7896,#7897,#4000,.T.);
#9886=EDGE_CURVE('',#7897,#7607,#3461,.T.);
#9887=EDGE_CURVE('',#7898,#7893,#4001,.T.);
#9888=EDGE_CURVE('',#7899,#7898,#4002,.T.);
#9889=EDGE_CURVE('',#7900,#7899,#3462,.T.);
#9890=EDGE_CURVE('',#7897,#7900,#4003,.T.);
#9891=EDGE_CURVE('',#7454,#7901,#4004,.T.);
#9892=EDGE_CURVE('',#7902,#7901,#3463,.F.);
#9893=EDGE_CURVE('',#7903,#7902,#3464,.F.);
#9894=EDGE_CURVE('',#7903,#7455,#4005,.T.);
#9895=EDGE_CURVE('',#7357,#7903,#4006,.T.);
#9896=EDGE_CURVE('',#7904,#7327,#4007,.T.);
#9897=EDGE_CURVE('',#7904,#7485,#4008,.T.);
#9898=EDGE_CURVE('',#7327,#7905,#3465,.T.);
#9899=EDGE_CURVE('',#7905,#7326,#3466,.T.);
#9900=EDGE_CURVE('',#7326,#7906,#4009,.T.);
#9901=EDGE_CURVE('',#7906,#7904,#3467,.T.);
#9902=EDGE_CURVE('',#7906,#7484,#4010,.T.);
#9903=EDGE_CURVE('',#7901,#7356,#4011,.T.);
#9904=EDGE_CURVE('',#7900,#7899,#4012,.T.);
#9905=EDGE_CURVE('',#7907,#7898,#3468,.T.);
#9906=EDGE_CURVE('',#7907,#7358,#4013,.T.);
#9907=EDGE_CURVE('',#7891,#7907,#4014,.T.);
#9908=EDGE_CURVE('',#7366,#7367,#3469,.T.);
#9909=EDGE_CURVE('',#7368,#7876,#4015,.T.);
#9910=EDGE_CURVE('',#7883,#7365,#4016,.T.);
#9911=EDGE_CURVE('',#7874,#7369,#4017,.T.);
#9912=EDGE_CURVE('',#7374,#7375,#3470,.T.);
#9913=EDGE_CURVE('',#7376,#7864,#4018,.T.);
#9914=EDGE_CURVE('',#7871,#7373,#4019,.T.);
#9915=EDGE_CURVE('',#7862,#7377,#4020,.T.);
#9916=EDGE_CURVE('',#7382,#7383,#3471,.T.);
#9917=EDGE_CURVE('',#7384,#7852,#4021,.T.);
#9918=EDGE_CURVE('',#7859,#7381,#4022,.T.);
#9919=EDGE_CURVE('',#7850,#7385,#4023,.T.);
#9920=EDGE_CURVE('',#7390,#7391,#3472,.T.);
#9921=EDGE_CURVE('',#7392,#7840,#4024,.T.);
#9922=EDGE_CURVE('',#7847,#7389,#4025,.T.);
#9923=EDGE_CURVE('',#7838,#7393,#4026,.T.);
#9924=EDGE_CURVE('',#7398,#7399,#3473,.T.);
#9925=EDGE_CURVE('',#7400,#7828,#4027,.T.);
#9926=EDGE_CURVE('',#7835,#7397,#4028,.T.);
#9927=EDGE_CURVE('',#7826,#7401,#4029,.T.);
#9928=EDGE_CURVE('',#7406,#7407,#3474,.T.);
#9929=EDGE_CURVE('',#7408,#7799,#4030,.T.);
#9930=EDGE_CURVE('',#7820,#7405,#4031,.T.);
#9931=EDGE_CURVE('',#7797,#7409,#4032,.T.);
#9932=EDGE_CURVE('',#7414,#7415,#3475,.T.);
#9933=EDGE_CURVE('',#7416,#7785,#4033,.T.);
#9934=EDGE_CURVE('',#7790,#7413,#4034,.T.);
#9935=EDGE_CURVE('',#7783,#7417,#4035,.T.);
#9936=EDGE_CURVE('',#7422,#7423,#3476,.T.);
#9937=EDGE_CURVE('',#7424,#7771,#4036,.T.);
#9938=EDGE_CURVE('',#7776,#7421,#4037,.T.);
#9939=EDGE_CURVE('',#7769,#7425,#4038,.T.);
#9940=EDGE_CURVE('',#7430,#7431,#3477,.T.);
#9941=EDGE_CURVE('',#7432,#7757,#4039,.T.);
#9942=EDGE_CURVE('',#7762,#7429,#4040,.T.);
#9943=EDGE_CURVE('',#7755,#7433,#4041,.T.);
#9944=EDGE_CURVE('',#7741,#7441,#4042,.T.);
#9945=EDGE_CURVE('',#7888,#7449,#4043,.T.);
#9946=EDGE_CURVE('',#7908,#7908,#3478,.T.);
#9947=EDGE_CURVE('',#7908,#7909,#4740,.T.);
#9948=EDGE_CURVE('',#7909,#7909,#3479,.T.);
#9949=EDGE_CURVE('',#7910,#7910,#3480,.T.);
#9950=EDGE_CURVE('',#7911,#7911,#3481,.T.);
#9951=EDGE_CURVE('',#7911,#7910,#4741,.T.);
#9952=EDGE_CURVE('',#7726,#7722,#4742,.T.);
#9953=EDGE_CURVE('',#7360,#7912,#4044,.T.);
#9954=EDGE_CURVE('',#7718,#7912,#3482,.T.);
#9955=EDGE_CURVE('',#7711,#7890,#4045,.T.);
#9956=EDGE_CURVE('',#7912,#7715,#4046,.T.);
#9957=EDGE_CURVE('',#7370,#7913,#4047,.T.);
#9958=EDGE_CURVE('',#7708,#7913,#3483,.T.);
#9959=EDGE_CURVE('',#7701,#7873,#4048,.T.);
#9960=EDGE_CURVE('',#7913,#7705,#4049,.T.);
#9961=EDGE_CURVE('',#7378,#7914,#4050,.T.);
#9962=EDGE_CURVE('',#7698,#7914,#3484,.T.);
#9963=EDGE_CURVE('',#7691,#7861,#4051,.T.);
#9964=EDGE_CURVE('',#7914,#7695,#4052,.T.);
#9965=EDGE_CURVE('',#7386,#7915,#4053,.T.);
#9966=EDGE_CURVE('',#7688,#7915,#3485,.T.);
#9967=EDGE_CURVE('',#7681,#7849,#4054,.T.);
#9968=EDGE_CURVE('',#7915,#7685,#4055,.T.);
#9969=EDGE_CURVE('',#7394,#7916,#4056,.T.);
#9970=EDGE_CURVE('',#7678,#7916,#3486,.T.);
#9971=EDGE_CURVE('',#7671,#7837,#4057,.T.);
#9972=EDGE_CURVE('',#7916,#7675,#4058,.T.);
#9973=EDGE_CURVE('',#7402,#7917,#4059,.T.);
#9974=EDGE_CURVE('',#7668,#7917,#3487,.T.);
#9975=EDGE_CURVE('',#7661,#7825,#4060,.T.);
#9976=EDGE_CURVE('',#7917,#7665,#4061,.T.);
#9977=EDGE_CURVE('',#7410,#7918,#4062,.T.);
#9978=EDGE_CURVE('',#7658,#7918,#3488,.T.);
#9979=EDGE_CURVE('',#7651,#7796,#4063,.T.);
#9980=EDGE_CURVE('',#7918,#7655,#4064,.T.);
#9981=EDGE_CURVE('',#7418,#7919,#4065,.T.);
#9982=EDGE_CURVE('',#7648,#7919,#3489,.T.);
#9983=EDGE_CURVE('',#7641,#7782,#4066,.T.);
#9984=EDGE_CURVE('',#7919,#7645,#4067,.T.);
#9985=EDGE_CURVE('',#7426,#7920,#4068,.T.);
#9986=EDGE_CURVE('',#7638,#7920,#3490,.T.);
#9987=EDGE_CURVE('',#7631,#7768,#4069,.T.);
#9988=EDGE_CURVE('',#7920,#7635,#4070,.T.);
#9989=EDGE_CURVE('',#7434,#7921,#4071,.T.);
#9990=EDGE_CURVE('',#7628,#7921,#3491,.T.);
#9991=EDGE_CURVE('',#7621,#7754,#4072,.T.);
#9992=EDGE_CURVE('',#7921,#7625,#4073,.T.);
#9993=EDGE_CURVE('',#7442,#7922,#4074,.T.);
#9994=EDGE_CURVE('',#7618,#7922,#3492,.T.);
#9995=EDGE_CURVE('',#7611,#7740,#4075,.T.);
#9996=EDGE_CURVE('',#7922,#7615,#4076,.T.);
#9997=EDGE_CURVE('',#7450,#7923,#4077,.T.);
#9998=EDGE_CURVE('',#7608,#7923,#3493,.T.);
#9999=EDGE_CURVE('',#7600,#7887,#4078,.T.);
#10000=EDGE_CURVE('',#7923,#7604,#4079,.T.);
#10001=EDGE_CURVE('',#7551,#7559,#4743,.T.);
#10002=EDGE_CURVE('',#7562,#7553,#4744,.T.);
#10003=EDGE_CURVE('',#7597,#7586,#4745,.T.);
#10004=EDGE_CURVE('',#7588,#7577,#4746,.T.);
#10005=EDGE_CURVE('',#7579,#7568,#4747,.T.);
#10006=EDGE_CURVE('',#7570,#7557,#4748,.T.);
#10007=EDGE_CURVE('',#7560,#7550,#4749,.T.);
#10008=EDGE_CURVE('',#7552,#7541,#4750,.T.);
#10009=EDGE_CURVE('',#7526,#7532,#4751,.T.);
#10010=EDGE_CURVE('',#7517,#7523,#4752,.T.);
#10011=EDGE_CURVE('',#7508,#7514,#4753,.T.);
#10012=EDGE_CURVE('',#7497,#7505,#4754,.T.);
#10013=EDGE_CURVE('',#7543,#7494,#4755,.T.);
#10014=EDGE_CURVE('',#7535,#7595,#4756,.T.);
#10015=EDGE_CURVE('',#7924,#7924,#3494,.T.);
#10016=EDGE_CURVE('',#7924,#7816,#4757,.T.);
#10017=EDGE_CURVE('',#7489,#7924,#4758,.T.);
#10018=EDGE_CURVE('',#7727,#7490,#4759,.T.);
#10019=EDGE_CURVE('',#7925,#7925,#3495,.T.);
#10020=EDGE_CURVE('',#7925,#7911,#4760,.T.);
#10021=EDGE_CURVE('',#7926,#7926,#3496,.T.);
#10022=EDGE_CURVE('',#7927,#7927,#3497,.T.);
#10023=EDGE_CURVE('',#7927,#7926,#4761,.T.);
#10024=EDGE_CURVE('',#7928,#7928,#3498,.T.);
#10025=EDGE_CURVE('',#7928,#7927,#4762,.T.);
#10026=EDGE_CURVE('',#7929,#7929,#3499,.T.);
#10027=EDGE_CURVE('',#7929,#7928,#4763,.T.);
#10028=EDGE_CURVE('',#7930,#7930,#3500,.T.);
#10029=EDGE_CURVE('',#7930,#7929,#4764,.T.);
#10030=EDGE_CURVE('',#7931,#7931,#3501,.T.);
#10031=EDGE_CURVE('',#7932,#7932,#3502,.T.);
#10032=EDGE_CURVE('',#7932,#7931,#4765,.T.);
#10033=EDGE_CURVE('',#7933,#7933,#3503,.T.);
#10034=EDGE_CURVE('',#7933,#7932,#4766,.T.);
#10035=EDGE_CURVE('',#7934,#7934,#3504,.T.);
#10036=EDGE_CURVE('',#7934,#7933,#4767,.T.);
#10037=EDGE_CURVE('',#7935,#7935,#3505,.T.);
#10038=EDGE_CURVE('',#7935,#7934,#4768,.T.);
#10039=EDGE_CURVE('',#7936,#7936,#3506,.T.);
#10040=EDGE_CURVE('',#7936,#7935,#4769,.T.);
#10041=EDGE_CURVE('',#7905,#7936,#4770,.T.);
#10042=EDGE_CURVE('',#7901,#7903,#3507,.F.);
#10043=EDGE_CURVE('',#7937,#7937,#3508,.T.);
#10044=EDGE_CURVE('',#7937,#7902,#4771,.T.);
#10045=EDGE_CURVE('',#7938,#7939,#4080,.T.);
#10046=EDGE_CURVE('',#7939,#7940,#4081,.T.);
#10047=EDGE_CURVE('',#7940,#7941,#4082,.T.);
#10048=EDGE_CURVE('',#7941,#7938,#4083,.T.);
#10049=EDGE_CURVE('',#7942,#7938,#4772,.T.);
#10050=EDGE_CURVE('',#7943,#7942,#4084,.T.);
#10051=EDGE_CURVE('',#7943,#7944,#4773,.T.);
#10052=EDGE_CURVE('',#7945,#7944,#4085,.T.);
#10053=EDGE_CURVE('',#7945,#7946,#4774,.T.);
#10054=EDGE_CURVE('',#7947,#7946,#4086,.T.);
#10055=EDGE_CURVE('',#7939,#7947,#4775,.T.);
#10056=EDGE_CURVE('',#7948,#7941,#4776,.T.);
#10057=EDGE_CURVE('',#7942,#7948,#4087,.T.);
#10058=EDGE_CURVE('',#7948,#7949,#4088,.T.);
#10059=EDGE_CURVE('',#7949,#7943,#4089,.T.);
#10060=EDGE_CURVE('',#7950,#7951,#4090,.T.);
#10061=EDGE_CURVE('',#7951,#7947,#4091,.T.);
#10062=EDGE_CURVE('',#7946,#7950,#4092,.T.);
#10063=EDGE_CURVE('',#7952,#7945,#4093,.T.);
#10064=EDGE_CURVE('',#7952,#7950,#4777,.T.);
#10065=EDGE_CURVE('',#7953,#7952,#4094,.T.);
#10066=EDGE_CURVE('',#7944,#7953,#4095,.T.);
#10067=EDGE_CURVE('',#7951,#7940,#4778,.T.);
#10068=EDGE_CURVE('',#7953,#7949,#4779,.T.);
#10069=EDGE_CURVE('',#7954,#7954,#3509,.T.);
#10070=EDGE_CURVE('',#7954,#7955,#4780,.T.);
#10071=EDGE_CURVE('',#7955,#7955,#3510,.T.);
#10072=EDGE_CURVE('',#7956,#7956,#3511,.T.);
#10073=EDGE_CURVE('',#7956,#7954,#4781,.T.);
#10074=EDGE_CURVE('',#7957,#7957,#3512,.T.);
#10075=EDGE_CURVE('',#7957,#7956,#4782,.T.);
#10076=EDGE_CURVE('',#7958,#7958,#3513,.T.);
#10077=EDGE_CURVE('',#7958,#7959,#4783,.T.);
#10078=EDGE_CURVE('',#7959,#7959,#3514,.T.);
#10079=EDGE_CURVE('',#7959,#7960,#4784,.T.);
#10080=EDGE_CURVE('',#7960,#7960,#3515,.T.);
#10081=EDGE_CURVE('',#7960,#7961,#4785,.T.);
#10082=EDGE_CURVE('',#7961,#7961,#3516,.T.);
#10083=EDGE_CURVE('',#7962,#7963,#4786,.F.);
#10084=EDGE_CURVE('',#7963,#7964,#4787,.T.);
#10085=EDGE_CURVE('',#7964,#7965,#4788,.F.);
#10086=EDGE_CURVE('',#7965,#7962,#4789,.T.);
#10087=EDGE_CURVE('',#7966,#7963,#4790,.T.);
#10088=EDGE_CURVE('',#7967,#7966,#4791,.T.);
#10089=EDGE_CURVE('',#7967,#7964,#4792,.T.);
#10090=EDGE_CURVE('',#7968,#7968,#3517,.T.);
#10091=EDGE_CURVE('',#7966,#7969,#4793,.F.);
#10092=EDGE_CURVE('',#7969,#7970,#4794,.T.);
#10093=EDGE_CURVE('',#7970,#7967,#4795,.F.);
#10094=EDGE_CURVE('',#7970,#7971,#4796,.T.);
#10095=EDGE_CURVE('',#7972,#7969,#4797,.T.);
#10096=EDGE_CURVE('',#7971,#7972,#3518,.T.);
#10097=EDGE_CURVE('',#7973,#7973,#3519,.T.);
#10098=EDGE_CURVE('',#7974,#7974,#3520,.T.);
#10099=EDGE_CURVE('',#7975,#7975,#3521,.T.);
#10100=EDGE_CURVE('',#7976,#7977,#4798,.T.);
#10101=EDGE_CURVE('',#7977,#7978,#4799,.T.);
#10102=EDGE_CURVE('',#7978,#7979,#4800,.T.);
#10103=EDGE_CURVE('',#7979,#7980,#4801,.T.);
#10104=EDGE_CURVE('',#7980,#7981,#4802,.T.);
#10105=EDGE_CURVE('',#7981,#7982,#4803,.T.);
#10106=EDGE_CURVE('',#7982,#7983,#4804,.T.);
#10107=EDGE_CURVE('',#7983,#7984,#4805,.T.);
#10108=EDGE_CURVE('',#7984,#7985,#4806,.T.);
#10109=EDGE_CURVE('',#7985,#7986,#4807,.T.);
#10110=EDGE_CURVE('',#7986,#7987,#4808,.T.);
#10111=EDGE_CURVE('',#7987,#7988,#4809,.T.);
#10112=EDGE_CURVE('',#7988,#7989,#4810,.T.);
#10113=EDGE_CURVE('',#7989,#7976,#4811,.T.);
#10114=EDGE_CURVE('',#7990,#7991,#4812,.T.);
#10115=EDGE_CURVE('',#7991,#7992,#4813,.T.);
#10116=EDGE_CURVE('',#7992,#7993,#4814,.T.);
#10117=EDGE_CURVE('',#7993,#7994,#4815,.T.);
#10118=EDGE_CURVE('',#7994,#7995,#4816,.T.);
#10119=EDGE_CURVE('',#7995,#7996,#4817,.T.);
#10120=EDGE_CURVE('',#7996,#7997,#4818,.T.);
#10121=EDGE_CURVE('',#7997,#7998,#4819,.T.);
#10122=EDGE_CURVE('',#7998,#7999,#4820,.T.);
#10123=EDGE_CURVE('',#7999,#8000,#4821,.T.);
#10124=EDGE_CURVE('',#8000,#8001,#4822,.T.);
#10125=EDGE_CURVE('',#8001,#8002,#4823,.T.);
#10126=EDGE_CURVE('',#8002,#8003,#4824,.T.);
#10127=EDGE_CURVE('',#8003,#7990,#4825,.T.);
#10128=EDGE_CURVE('',#8004,#8005,#4826,.T.);
#10129=EDGE_CURVE('',#8005,#8006,#4827,.T.);
#10130=EDGE_CURVE('',#8006,#8007,#4828,.T.);
#10131=EDGE_CURVE('',#8007,#8008,#4829,.T.);
#10132=EDGE_CURVE('',#8008,#8009,#4830,.T.);
#10133=EDGE_CURVE('',#8009,#8010,#4831,.T.);
#10134=EDGE_CURVE('',#8010,#8011,#4832,.T.);
#10135=EDGE_CURVE('',#8011,#8012,#4833,.T.);
#10136=EDGE_CURVE('',#8012,#8013,#4834,.T.);
#10137=EDGE_CURVE('',#8013,#8014,#4835,.T.);
#10138=EDGE_CURVE('',#8014,#8015,#4836,.T.);
#10139=EDGE_CURVE('',#8015,#8016,#4837,.T.);
#10140=EDGE_CURVE('',#8016,#8017,#4838,.T.);
#10141=EDGE_CURVE('',#8017,#8004,#4839,.T.);
#10142=EDGE_CURVE('',#8018,#8019,#4840,.T.);
#10143=EDGE_CURVE('',#8019,#8020,#4841,.T.);
#10144=EDGE_CURVE('',#8020,#8021,#4842,.T.);
#10145=EDGE_CURVE('',#8021,#8022,#4843,.T.);
#10146=EDGE_CURVE('',#8022,#8023,#4844,.T.);
#10147=EDGE_CURVE('',#8023,#8024,#4845,.T.);
#10148=EDGE_CURVE('',#8024,#8025,#4846,.T.);
#10149=EDGE_CURVE('',#8025,#8026,#4847,.T.);
#10150=EDGE_CURVE('',#8026,#8027,#4848,.T.);
#10151=EDGE_CURVE('',#8027,#8028,#4849,.T.);
#10152=EDGE_CURVE('',#8028,#8029,#4850,.T.);
#10153=EDGE_CURVE('',#8029,#8030,#4851,.T.);
#10154=EDGE_CURVE('',#8030,#8031,#4852,.T.);
#10155=EDGE_CURVE('',#8031,#8018,#4853,.T.);
#10156=EDGE_CURVE('',#8032,#8033,#4854,.T.);
#10157=EDGE_CURVE('',#8033,#8034,#4855,.T.);
#10158=EDGE_CURVE('',#8034,#8035,#4856,.T.);
#10159=EDGE_CURVE('',#8035,#8036,#4857,.T.);
#10160=EDGE_CURVE('',#8036,#8037,#4858,.T.);
#10161=EDGE_CURVE('',#8037,#8038,#4859,.T.);
#10162=EDGE_CURVE('',#8038,#8039,#4860,.T.);
#10163=EDGE_CURVE('',#8039,#8040,#4861,.T.);
#10164=EDGE_CURVE('',#8040,#8041,#4862,.T.);
#10165=EDGE_CURVE('',#8041,#8042,#4863,.T.);
#10166=EDGE_CURVE('',#8042,#8043,#4864,.T.);
#10167=EDGE_CURVE('',#8043,#8044,#4865,.T.);
#10168=EDGE_CURVE('',#8044,#8045,#4866,.T.);
#10169=EDGE_CURVE('',#8045,#8032,#4867,.T.);
#10170=EDGE_CURVE('',#8046,#8047,#4868,.T.);
#10171=EDGE_CURVE('',#8047,#8048,#4869,.T.);
#10172=EDGE_CURVE('',#8048,#8049,#4870,.T.);
#10173=EDGE_CURVE('',#8049,#8050,#4871,.T.);
#10174=EDGE_CURVE('',#8050,#8051,#4872,.T.);
#10175=EDGE_CURVE('',#8051,#8052,#4873,.T.);
#10176=EDGE_CURVE('',#8052,#8053,#4874,.T.);
#10177=EDGE_CURVE('',#8053,#8054,#4875,.T.);
#10178=EDGE_CURVE('',#8054,#8055,#4876,.T.);
#10179=EDGE_CURVE('',#8055,#8056,#4877,.T.);
#10180=EDGE_CURVE('',#8056,#8057,#4878,.T.);
#10181=EDGE_CURVE('',#8057,#8058,#4879,.T.);
#10182=EDGE_CURVE('',#8058,#8059,#4880,.T.);
#10183=EDGE_CURVE('',#8059,#8046,#4881,.T.);
#10184=EDGE_CURVE('',#8060,#8060,#3522,.T.);
#10185=EDGE_CURVE('',#7972,#8061,#1050,.T.);
#10186=EDGE_CURVE('',#8061,#8062,#4096,.T.);
#10187=EDGE_CURVE('',#8062,#8063,#3523,.T.);
#10188=EDGE_CURVE('',#8063,#8064,#4097,.T.);
#10189=EDGE_CURVE('',#8064,#7971,#1051,.T.);
#10190=EDGE_CURVE('',#8065,#8062,#4882,.T.);
#10191=EDGE_CURVE('',#8061,#8066,#4883,.T.);
#10192=EDGE_CURVE('',#8066,#8065,#4098,.T.);
#10193=EDGE_CURVE('',#8067,#8065,#3524,.T.);
#10194=EDGE_CURVE('',#8066,#8068,#1052,.T.);
#10195=EDGE_CURVE('',#8068,#8069,#3525,.T.);
#10196=EDGE_CURVE('',#8069,#8070,#1053,.T.);
#10197=EDGE_CURVE('',#8067,#8070,#4099,.T.);
#10198=EDGE_CURVE('',#8070,#8064,#4884,.T.);
#10199=EDGE_CURVE('',#8063,#8067,#4885,.T.);
#10200=EDGE_CURVE('',#7965,#8069,#4886,.T.);
#10201=EDGE_CURVE('',#8068,#7962,#4887,.T.);
#10202=EDGE_CURVE('',#8071,#8071,#3526,.T.);
#10203=EDGE_CURVE('',#8072,#8072,#3527,.T.);
#10204=EDGE_CURVE('',#8073,#8073,#3528,.T.);
#10205=EDGE_CURVE('',#8074,#8075,#4888,.T.);
#10206=EDGE_CURVE('',#8075,#8076,#4889,.T.);
#10207=EDGE_CURVE('',#8076,#8077,#4890,.T.);
#10208=EDGE_CURVE('',#8077,#8078,#4891,.T.);
#10209=EDGE_CURVE('',#8078,#8079,#4892,.T.);
#10210=EDGE_CURVE('',#8079,#8080,#4893,.T.);
#10211=EDGE_CURVE('',#8080,#8081,#4894,.T.);
#10212=EDGE_CURVE('',#8081,#8082,#4895,.T.);
#10213=EDGE_CURVE('',#8082,#8083,#4896,.T.);
#10214=EDGE_CURVE('',#8083,#8084,#4897,.T.);
#10215=EDGE_CURVE('',#8084,#8085,#4898,.T.);
#10216=EDGE_CURVE('',#8085,#8086,#4899,.T.);
#10217=EDGE_CURVE('',#8086,#8087,#4900,.T.);
#10218=EDGE_CURVE('',#8087,#8074,#4901,.T.);
#10219=EDGE_CURVE('',#8088,#8089,#4902,.T.);
#10220=EDGE_CURVE('',#8089,#8090,#4903,.T.);
#10221=EDGE_CURVE('',#8090,#8091,#4904,.T.);
#10222=EDGE_CURVE('',#8091,#8092,#4905,.T.);
#10223=EDGE_CURVE('',#8092,#8093,#4906,.T.);
#10224=EDGE_CURVE('',#8093,#8094,#4907,.T.);
#10225=EDGE_CURVE('',#8094,#8095,#4908,.T.);
#10226=EDGE_CURVE('',#8095,#8096,#4909,.T.);
#10227=EDGE_CURVE('',#8096,#8097,#4910,.T.);
#10228=EDGE_CURVE('',#8097,#8098,#4911,.T.);
#10229=EDGE_CURVE('',#8098,#8099,#4912,.T.);
#10230=EDGE_CURVE('',#8099,#8100,#4913,.T.);
#10231=EDGE_CURVE('',#8100,#8101,#4914,.T.);
#10232=EDGE_CURVE('',#8101,#8088,#4915,.T.);
#10233=EDGE_CURVE('',#8102,#8103,#4916,.T.);
#10234=EDGE_CURVE('',#8103,#8104,#4917,.T.);
#10235=EDGE_CURVE('',#8104,#8105,#4918,.T.);
#10236=EDGE_CURVE('',#8105,#8106,#4919,.T.);
#10237=EDGE_CURVE('',#8106,#8107,#4920,.T.);
#10238=EDGE_CURVE('',#8107,#8108,#4921,.T.);
#10239=EDGE_CURVE('',#8108,#8109,#4922,.T.);
#10240=EDGE_CURVE('',#8109,#8110,#4923,.T.);
#10241=EDGE_CURVE('',#8110,#8111,#4924,.T.);
#10242=EDGE_CURVE('',#8111,#8112,#4925,.T.);
#10243=EDGE_CURVE('',#8112,#8113,#4926,.T.);
#10244=EDGE_CURVE('',#8113,#8114,#4927,.T.);
#10245=EDGE_CURVE('',#8114,#8115,#4928,.T.);
#10246=EDGE_CURVE('',#8115,#8102,#4929,.T.);
#10247=EDGE_CURVE('',#8116,#8117,#4930,.T.);
#10248=EDGE_CURVE('',#8117,#8118,#4931,.T.);
#10249=EDGE_CURVE('',#8118,#8119,#4932,.T.);
#10250=EDGE_CURVE('',#8119,#8120,#4933,.T.);
#10251=EDGE_CURVE('',#8120,#8121,#4934,.T.);
#10252=EDGE_CURVE('',#8121,#8122,#4935,.T.);
#10253=EDGE_CURVE('',#8122,#8123,#4936,.T.);
#10254=EDGE_CURVE('',#8123,#8124,#4937,.T.);
#10255=EDGE_CURVE('',#8124,#8125,#4938,.T.);
#10256=EDGE_CURVE('',#8125,#8126,#4939,.T.);
#10257=EDGE_CURVE('',#8126,#8127,#4940,.T.);
#10258=EDGE_CURVE('',#8127,#8128,#4941,.T.);
#10259=EDGE_CURVE('',#8128,#8129,#4942,.T.);
#10260=EDGE_CURVE('',#8129,#8116,#4943,.T.);
#10261=EDGE_CURVE('',#8130,#8131,#4944,.T.);
#10262=EDGE_CURVE('',#8131,#8132,#4945,.T.);
#10263=EDGE_CURVE('',#8132,#8133,#4946,.T.);
#10264=EDGE_CURVE('',#8133,#8134,#4947,.T.);
#10265=EDGE_CURVE('',#8134,#8135,#4948,.T.);
#10266=EDGE_CURVE('',#8135,#8136,#4949,.T.);
#10267=EDGE_CURVE('',#8136,#8137,#4950,.T.);
#10268=EDGE_CURVE('',#8137,#8138,#4951,.T.);
#10269=EDGE_CURVE('',#8138,#8139,#4952,.T.);
#10270=EDGE_CURVE('',#8139,#8140,#4953,.T.);
#10271=EDGE_CURVE('',#8140,#8141,#4954,.T.);
#10272=EDGE_CURVE('',#8141,#8142,#4955,.T.);
#10273=EDGE_CURVE('',#8142,#8143,#4956,.T.);
#10274=EDGE_CURVE('',#8143,#8130,#4957,.T.);
#10275=EDGE_CURVE('',#8144,#8145,#4958,.T.);
#10276=EDGE_CURVE('',#8145,#8146,#4959,.T.);
#10277=EDGE_CURVE('',#8146,#8147,#4960,.T.);
#10278=EDGE_CURVE('',#8147,#8148,#4961,.T.);
#10279=EDGE_CURVE('',#8148,#8149,#4962,.T.);
#10280=EDGE_CURVE('',#8149,#8150,#4963,.T.);
#10281=EDGE_CURVE('',#8150,#8151,#4964,.T.);
#10282=EDGE_CURVE('',#8151,#8152,#4965,.T.);
#10283=EDGE_CURVE('',#8152,#8153,#4966,.T.);
#10284=EDGE_CURVE('',#8153,#8154,#4967,.T.);
#10285=EDGE_CURVE('',#8154,#8155,#4968,.T.);
#10286=EDGE_CURVE('',#8155,#8156,#4969,.T.);
#10287=EDGE_CURVE('',#8156,#8157,#4970,.T.);
#10288=EDGE_CURVE('',#8157,#8144,#4971,.T.);
#10289=EDGE_CURVE('',#8158,#8158,#3529,.T.);
#10290=EDGE_CURVE('',#7973,#8159,#4972,.T.);
#10291=EDGE_CURVE('',#8159,#8159,#3530,.T.);
#10292=EDGE_CURVE('',#8159,#8160,#4973,.T.);
#10293=EDGE_CURVE('',#8160,#8160,#3531,.T.);
#10294=EDGE_CURVE('',#8071,#8160,#4974,.T.);
#10295=EDGE_CURVE('',#8060,#8161,#4975,.T.);
#10296=EDGE_CURVE('',#8161,#8161,#3532,.T.);
#10297=EDGE_CURVE('',#8161,#8162,#4976,.T.);
#10298=EDGE_CURVE('',#8162,#8162,#3533,.T.);
#10299=EDGE_CURVE('',#8158,#8162,#4977,.T.);
#10300=EDGE_CURVE('',#7974,#8163,#4978,.T.);
#10301=EDGE_CURVE('',#8163,#8163,#3534,.T.);
#10302=EDGE_CURVE('',#8163,#8164,#4979,.T.);
#10303=EDGE_CURVE('',#8164,#8164,#3535,.T.);
#10304=EDGE_CURVE('',#8072,#8164,#4980,.T.);
#10305=EDGE_CURVE('',#7968,#8165,#4981,.T.);
#10306=EDGE_CURVE('',#8165,#8165,#3536,.T.);
#10307=EDGE_CURVE('',#8165,#8166,#4982,.T.);
#10308=EDGE_CURVE('',#8167,#8166,#4100,.T.);
#10309=EDGE_CURVE('',#8168,#8167,#4101,.T.);
#10310=EDGE_CURVE('',#8166,#8168,#4102,.T.);
#10311=EDGE_CURVE('',#8144,#8169,#4983,.T.);
#10312=EDGE_CURVE('',#8169,#8170,#4984,.T.);
#10313=EDGE_CURVE('',#8145,#8170,#4985,.T.);
#10314=EDGE_CURVE('',#8157,#8171,#4986,.T.);
#10315=EDGE_CURVE('',#8171,#8169,#4987,.T.);
#10316=EDGE_CURVE('',#8156,#8172,#4988,.T.);
#10317=EDGE_CURVE('',#8172,#8171,#4989,.T.);
#10318=EDGE_CURVE('',#8155,#8173,#4990,.T.);
#10319=EDGE_CURVE('',#8173,#8172,#4991,.T.);
#10320=EDGE_CURVE('',#8154,#8174,#4992,.T.);
#10321=EDGE_CURVE('',#8174,#8173,#4993,.T.);
#10322=EDGE_CURVE('',#8153,#8175,#4994,.T.);
#10323=EDGE_CURVE('',#8175,#8174,#4995,.T.);
#10324=EDGE_CURVE('',#8152,#8176,#4996,.T.);
#10325=EDGE_CURVE('',#8176,#8175,#4997,.T.);
#10326=EDGE_CURVE('',#8151,#8177,#4998,.T.);
#10327=EDGE_CURVE('',#8177,#8176,#4999,.T.);
#10328=EDGE_CURVE('',#8150,#8178,#5000,.T.);
#10329=EDGE_CURVE('',#8178,#8177,#5001,.T.);
#10330=EDGE_CURVE('',#8149,#8179,#5002,.T.);
#10331=EDGE_CURVE('',#8179,#8178,#5003,.T.);
#10332=EDGE_CURVE('',#8148,#8180,#5004,.T.);
#10333=EDGE_CURVE('',#8180,#8179,#5005,.T.);
#10334=EDGE_CURVE('',#8147,#8181,#5006,.T.);
#10335=EDGE_CURVE('',#8181,#8180,#5007,.T.);
#10336=EDGE_CURVE('',#8146,#8182,#5008,.T.);
#10337=EDGE_CURVE('',#8182,#8181,#5009,.T.);
#10338=EDGE_CURVE('',#8170,#8182,#5010,.T.);
#10339=EDGE_CURVE('',#8130,#8183,#5011,.T.);
#10340=EDGE_CURVE('',#8183,#8184,#5012,.T.);
#10341=EDGE_CURVE('',#8131,#8184,#5013,.T.);
#10342=EDGE_CURVE('',#8143,#8185,#5014,.T.);
#10343=EDGE_CURVE('',#8185,#8183,#5015,.T.);
#10344=EDGE_CURVE('',#8142,#8186,#5016,.T.);
#10345=EDGE_CURVE('',#8186,#8185,#5017,.T.);
#10346=EDGE_CURVE('',#8141,#8187,#5018,.T.);
#10347=EDGE_CURVE('',#8187,#8186,#5019,.T.);
#10348=EDGE_CURVE('',#8140,#8188,#5020,.T.);
#10349=EDGE_CURVE('',#8188,#8187,#5021,.T.);
#10350=EDGE_CURVE('',#8139,#8189,#5022,.T.);
#10351=EDGE_CURVE('',#8189,#8188,#5023,.T.);
#10352=EDGE_CURVE('',#8138,#8190,#5024,.T.);
#10353=EDGE_CURVE('',#8190,#8189,#5025,.T.);
#10354=EDGE_CURVE('',#8137,#8191,#5026,.T.);
#10355=EDGE_CURVE('',#8191,#8190,#5027,.T.);
#10356=EDGE_CURVE('',#8136,#8192,#5028,.T.);
#10357=EDGE_CURVE('',#8192,#8191,#5029,.T.);
#10358=EDGE_CURVE('',#8135,#8193,#5030,.T.);
#10359=EDGE_CURVE('',#8193,#8192,#5031,.T.);
#10360=EDGE_CURVE('',#8134,#8194,#5032,.T.);
#10361=EDGE_CURVE('',#8194,#8193,#5033,.T.);
#10362=EDGE_CURVE('',#8133,#8195,#5034,.T.);
#10363=EDGE_CURVE('',#8195,#8194,#5035,.T.);
#10364=EDGE_CURVE('',#8132,#8196,#5036,.T.);
#10365=EDGE_CURVE('',#8196,#8195,#5037,.T.);
#10366=EDGE_CURVE('',#8184,#8196,#5038,.T.);
#10367=EDGE_CURVE('',#8116,#8197,#5039,.T.);
#10368=EDGE_CURVE('',#8197,#8198,#5040,.T.);
#10369=EDGE_CURVE('',#8117,#8198,#5041,.T.);
#10370=EDGE_CURVE('',#8129,#8199,#5042,.T.);
#10371=EDGE_CURVE('',#8199,#8197,#5043,.T.);
#10372=EDGE_CURVE('',#8128,#8200,#5044,.T.);
#10373=EDGE_CURVE('',#8200,#8199,#5045,.T.);
#10374=EDGE_CURVE('',#8127,#8201,#5046,.T.);
#10375=EDGE_CURVE('',#8201,#8200,#5047,.T.);
#10376=EDGE_CURVE('',#8126,#8202,#5048,.T.);
#10377=EDGE_CURVE('',#8202,#8201,#5049,.T.);
#10378=EDGE_CURVE('',#8125,#8203,#5050,.T.);
#10379=EDGE_CURVE('',#8203,#8202,#5051,.T.);
#10380=EDGE_CURVE('',#8124,#8204,#5052,.T.);
#10381=EDGE_CURVE('',#8204,#8203,#5053,.T.);
#10382=EDGE_CURVE('',#8123,#8205,#5054,.T.);
#10383=EDGE_CURVE('',#8205,#8204,#5055,.T.);
#10384=EDGE_CURVE('',#8122,#8206,#5056,.T.);
#10385=EDGE_CURVE('',#8206,#8205,#5057,.T.);
#10386=EDGE_CURVE('',#8121,#8207,#5058,.T.);
#10387=EDGE_CURVE('',#8207,#8206,#5059,.T.);
#10388=EDGE_CURVE('',#8120,#8208,#5060,.T.);
#10389=EDGE_CURVE('',#8208,#8207,#5061,.T.);
#10390=EDGE_CURVE('',#8119,#8209,#5062,.T.);
#10391=EDGE_CURVE('',#8209,#8208,#5063,.T.);
#10392=EDGE_CURVE('',#8118,#8210,#5064,.T.);
#10393=EDGE_CURVE('',#8210,#8209,#5065,.T.);
#10394=EDGE_CURVE('',#8198,#8210,#5066,.T.);
#10395=EDGE_CURVE('',#8102,#8211,#5067,.T.);
#10396=EDGE_CURVE('',#8211,#8212,#5068,.T.);
#10397=EDGE_CURVE('',#8103,#8212,#5069,.T.);
#10398=EDGE_CURVE('',#8115,#8213,#5070,.T.);
#10399=EDGE_CURVE('',#8213,#8211,#5071,.T.);
#10400=EDGE_CURVE('',#8114,#8214,#5072,.T.);
#10401=EDGE_CURVE('',#8214,#8213,#5073,.T.);
#10402=EDGE_CURVE('',#8113,#8215,#5074,.T.);
#10403=EDGE_CURVE('',#8215,#8214,#5075,.T.);
#10404=EDGE_CURVE('',#8112,#8216,#5076,.T.);
#10405=EDGE_CURVE('',#8216,#8215,#5077,.T.);
#10406=EDGE_CURVE('',#8111,#8217,#5078,.T.);
#10407=EDGE_CURVE('',#8217,#8216,#5079,.T.);
#10408=EDGE_CURVE('',#8110,#8218,#5080,.T.);
#10409=EDGE_CURVE('',#8218,#8217,#5081,.T.);
#10410=EDGE_CURVE('',#8109,#8219,#5082,.T.);
#10411=EDGE_CURVE('',#8219,#8218,#5083,.T.);
#10412=EDGE_CURVE('',#8108,#8220,#5084,.T.);
#10413=EDGE_CURVE('',#8220,#8219,#5085,.T.);
#10414=EDGE_CURVE('',#8107,#8221,#5086,.T.);
#10415=EDGE_CURVE('',#8221,#8220,#5087,.T.);
#10416=EDGE_CURVE('',#8106,#8222,#5088,.T.);
#10417=EDGE_CURVE('',#8222,#8221,#5089,.T.);
#10418=EDGE_CURVE('',#8105,#8223,#5090,.T.);
#10419=EDGE_CURVE('',#8223,#8222,#5091,.T.);
#10420=EDGE_CURVE('',#8104,#8224,#5092,.T.);
#10421=EDGE_CURVE('',#8224,#8223,#5093,.T.);
#10422=EDGE_CURVE('',#8212,#8224,#5094,.T.);
#10423=EDGE_CURVE('',#8088,#8225,#5095,.T.);
#10424=EDGE_CURVE('',#8225,#8226,#5096,.T.);
#10425=EDGE_CURVE('',#8089,#8226,#5097,.T.);
#10426=EDGE_CURVE('',#8101,#8227,#5098,.T.);
#10427=EDGE_CURVE('',#8227,#8225,#5099,.T.);
#10428=EDGE_CURVE('',#8100,#8228,#5100,.T.);
#10429=EDGE_CURVE('',#8228,#8227,#5101,.T.);
#10430=EDGE_CURVE('',#8099,#8229,#5102,.T.);
#10431=EDGE_CURVE('',#8229,#8228,#5103,.T.);
#10432=EDGE_CURVE('',#8098,#8230,#5104,.T.);
#10433=EDGE_CURVE('',#8230,#8229,#5105,.T.);
#10434=EDGE_CURVE('',#8097,#8231,#5106,.T.);
#10435=EDGE_CURVE('',#8231,#8230,#5107,.T.);
#10436=EDGE_CURVE('',#8096,#8232,#5108,.T.);
#10437=EDGE_CURVE('',#8232,#8231,#5109,.T.);
#10438=EDGE_CURVE('',#8095,#8233,#5110,.T.);
#10439=EDGE_CURVE('',#8233,#8232,#5111,.T.);
#10440=EDGE_CURVE('',#8094,#8234,#5112,.T.);
#10441=EDGE_CURVE('',#8234,#8233,#5113,.T.);
#10442=EDGE_CURVE('',#8093,#8235,#5114,.T.);
#10443=EDGE_CURVE('',#8235,#8234,#5115,.T.);
#10444=EDGE_CURVE('',#8092,#8236,#5116,.T.);
#10445=EDGE_CURVE('',#8236,#8235,#5117,.T.);
#10446=EDGE_CURVE('',#8091,#8237,#5118,.T.);
#10447=EDGE_CURVE('',#8237,#8236,#5119,.T.);
#10448=EDGE_CURVE('',#8090,#8238,#5120,.T.);
#10449=EDGE_CURVE('',#8238,#8237,#5121,.T.);
#10450=EDGE_CURVE('',#8226,#8238,#5122,.T.);
#10451=EDGE_CURVE('',#8074,#8239,#5123,.T.);
#10452=EDGE_CURVE('',#8239,#8240,#5124,.T.);
#10453=EDGE_CURVE('',#8075,#8240,#5125,.T.);
#10454=EDGE_CURVE('',#8087,#8241,#5126,.T.);
#10455=EDGE_CURVE('',#8241,#8239,#5127,.T.);
#10456=EDGE_CURVE('',#8086,#8242,#5128,.T.);
#10457=EDGE_CURVE('',#8242,#8241,#5129,.T.);
#10458=EDGE_CURVE('',#8085,#8243,#5130,.T.);
#10459=EDGE_CURVE('',#8243,#8242,#5131,.T.);
#10460=EDGE_CURVE('',#8084,#8244,#5132,.T.);
#10461=EDGE_CURVE('',#8244,#8243,#5133,.T.);
#10462=EDGE_CURVE('',#8083,#8245,#5134,.T.);
#10463=EDGE_CURVE('',#8245,#8244,#5135,.T.);
#10464=EDGE_CURVE('',#8082,#8246,#5136,.T.);
#10465=EDGE_CURVE('',#8246,#8245,#5137,.T.);
#10466=EDGE_CURVE('',#8081,#8247,#5138,.T.);
#10467=EDGE_CURVE('',#8247,#8246,#5139,.T.);
#10468=EDGE_CURVE('',#8080,#8248,#5140,.T.);
#10469=EDGE_CURVE('',#8248,#8247,#5141,.T.);
#10470=EDGE_CURVE('',#8079,#8249,#5142,.T.);
#10471=EDGE_CURVE('',#8249,#8248,#5143,.T.);
#10472=EDGE_CURVE('',#8078,#8250,#5144,.T.);
#10473=EDGE_CURVE('',#8250,#8249,#5145,.T.);
#10474=EDGE_CURVE('',#8077,#8251,#5146,.T.);
#10475=EDGE_CURVE('',#8251,#8250,#5147,.T.);
#10476=EDGE_CURVE('',#8076,#8252,#5148,.T.);
#10477=EDGE_CURVE('',#8252,#8251,#5149,.T.);
#10478=EDGE_CURVE('',#8240,#8252,#5150,.T.);
#10479=EDGE_CURVE('',#8046,#8253,#5151,.T.);
#10480=EDGE_CURVE('',#8253,#8254,#5152,.T.);
#10481=EDGE_CURVE('',#8047,#8254,#5153,.T.);
#10482=EDGE_CURVE('',#8059,#8255,#5154,.T.);
#10483=EDGE_CURVE('',#8255,#8253,#5155,.T.);
#10484=EDGE_CURVE('',#8058,#8256,#5156,.T.);
#10485=EDGE_CURVE('',#8256,#8255,#5157,.T.);
#10486=EDGE_CURVE('',#8057,#8257,#5158,.T.);
#10487=EDGE_CURVE('',#8257,#8256,#5159,.T.);
#10488=EDGE_CURVE('',#8056,#8258,#5160,.T.);
#10489=EDGE_CURVE('',#8258,#8257,#5161,.T.);
#10490=EDGE_CURVE('',#8055,#8259,#5162,.T.);
#10491=EDGE_CURVE('',#8259,#8258,#5163,.T.);
#10492=EDGE_CURVE('',#8054,#8260,#5164,.T.);
#10493=EDGE_CURVE('',#8260,#8259,#5165,.T.);
#10494=EDGE_CURVE('',#8053,#8261,#5166,.T.);
#10495=EDGE_CURVE('',#8261,#8260,#5167,.T.);
#10496=EDGE_CURVE('',#8052,#8262,#5168,.T.);
#10497=EDGE_CURVE('',#8262,#8261,#5169,.T.);
#10498=EDGE_CURVE('',#8051,#8263,#5170,.T.);
#10499=EDGE_CURVE('',#8263,#8262,#5171,.T.);
#10500=EDGE_CURVE('',#8050,#8264,#5172,.T.);
#10501=EDGE_CURVE('',#8264,#8263,#5173,.T.);
#10502=EDGE_CURVE('',#8049,#8265,#5174,.T.);
#10503=EDGE_CURVE('',#8265,#8264,#5175,.T.);
#10504=EDGE_CURVE('',#8048,#8266,#5176,.T.);
#10505=EDGE_CURVE('',#8266,#8265,#5177,.T.);
#10506=EDGE_CURVE('',#8254,#8266,#5178,.T.);
#10507=EDGE_CURVE('',#8032,#8267,#5179,.T.);
#10508=EDGE_CURVE('',#8267,#8268,#5180,.T.);
#10509=EDGE_CURVE('',#8033,#8268,#5181,.T.);
#10510=EDGE_CURVE('',#8045,#8269,#5182,.T.);
#10511=EDGE_CURVE('',#8269,#8267,#5183,.T.);
#10512=EDGE_CURVE('',#8044,#8270,#5184,.T.);
#10513=EDGE_CURVE('',#8270,#8269,#5185,.T.);
#10514=EDGE_CURVE('',#8043,#8271,#5186,.T.);
#10515=EDGE_CURVE('',#8271,#8270,#5187,.T.);
#10516=EDGE_CURVE('',#8042,#8272,#5188,.T.);
#10517=EDGE_CURVE('',#8272,#8271,#5189,.T.);
#10518=EDGE_CURVE('',#8041,#8273,#5190,.T.);
#10519=EDGE_CURVE('',#8273,#8272,#5191,.T.);
#10520=EDGE_CURVE('',#8040,#8274,#5192,.T.);
#10521=EDGE_CURVE('',#8274,#8273,#5193,.T.);
#10522=EDGE_CURVE('',#8039,#8275,#5194,.T.);
#10523=EDGE_CURVE('',#8275,#8274,#5195,.T.);
#10524=EDGE_CURVE('',#8038,#8276,#5196,.T.);
#10525=EDGE_CURVE('',#8276,#8275,#5197,.T.);
#10526=EDGE_CURVE('',#8037,#8277,#5198,.T.);
#10527=EDGE_CURVE('',#8277,#8276,#5199,.T.);
#10528=EDGE_CURVE('',#8036,#8278,#5200,.T.);
#10529=EDGE_CURVE('',#8278,#8277,#5201,.T.);
#10530=EDGE_CURVE('',#8035,#8279,#5202,.T.);
#10531=EDGE_CURVE('',#8279,#8278,#5203,.T.);
#10532=EDGE_CURVE('',#8034,#8280,#5204,.T.);
#10533=EDGE_CURVE('',#8280,#8279,#5205,.T.);
#10534=EDGE_CURVE('',#8268,#8280,#5206,.T.);
#10535=EDGE_CURVE('',#8018,#8281,#5207,.T.);
#10536=EDGE_CURVE('',#8281,#8282,#5208,.T.);
#10537=EDGE_CURVE('',#8019,#8282,#5209,.T.);
#10538=EDGE_CURVE('',#8031,#8283,#5210,.T.);
#10539=EDGE_CURVE('',#8283,#8281,#5211,.T.);
#10540=EDGE_CURVE('',#8030,#8284,#5212,.T.);
#10541=EDGE_CURVE('',#8284,#8283,#5213,.T.);
#10542=EDGE_CURVE('',#8029,#8285,#5214,.T.);
#10543=EDGE_CURVE('',#8285,#8284,#5215,.T.);
#10544=EDGE_CURVE('',#8028,#8286,#5216,.T.);
#10545=EDGE_CURVE('',#8286,#8285,#5217,.T.);
#10546=EDGE_CURVE('',#8027,#8287,#5218,.T.);
#10547=EDGE_CURVE('',#8287,#8286,#5219,.T.);
#10548=EDGE_CURVE('',#8026,#8288,#5220,.T.);
#10549=EDGE_CURVE('',#8288,#8287,#5221,.T.);
#10550=EDGE_CURVE('',#8025,#8289,#5222,.T.);
#10551=EDGE_CURVE('',#8289,#8288,#5223,.T.);
#10552=EDGE_CURVE('',#8024,#8290,#5224,.T.);
#10553=EDGE_CURVE('',#8290,#8289,#5225,.T.);
#10554=EDGE_CURVE('',#8023,#8291,#5226,.T.);
#10555=EDGE_CURVE('',#8291,#8290,#5227,.T.);
#10556=EDGE_CURVE('',#8022,#8292,#5228,.T.);
#10557=EDGE_CURVE('',#8292,#8291,#5229,.T.);
#10558=EDGE_CURVE('',#8021,#8293,#5230,.T.);
#10559=EDGE_CURVE('',#8293,#8292,#5231,.T.);
#10560=EDGE_CURVE('',#8020,#8294,#5232,.T.);
#10561=EDGE_CURVE('',#8294,#8293,#5233,.T.);
#10562=EDGE_CURVE('',#8282,#8294,#5234,.T.);
#10563=EDGE_CURVE('',#8004,#8295,#5235,.T.);
#10564=EDGE_CURVE('',#8295,#8296,#5236,.T.);
#10565=EDGE_CURVE('',#8005,#8296,#5237,.T.);
#10566=EDGE_CURVE('',#8017,#8297,#5238,.T.);
#10567=EDGE_CURVE('',#8297,#8295,#5239,.T.);
#10568=EDGE_CURVE('',#8016,#8298,#5240,.T.);
#10569=EDGE_CURVE('',#8298,#8297,#5241,.T.);
#10570=EDGE_CURVE('',#8015,#8299,#5242,.T.);
#10571=EDGE_CURVE('',#8299,#8298,#5243,.T.);
#10572=EDGE_CURVE('',#8014,#8300,#5244,.T.);
#10573=EDGE_CURVE('',#8300,#8299,#5245,.T.);
#10574=EDGE_CURVE('',#8013,#8301,#5246,.T.);
#10575=EDGE_CURVE('',#8301,#8300,#5247,.T.);
#10576=EDGE_CURVE('',#8012,#8302,#5248,.T.);
#10577=EDGE_CURVE('',#8302,#8301,#5249,.T.);
#10578=EDGE_CURVE('',#8011,#8303,#5250,.T.);
#10579=EDGE_CURVE('',#8303,#8302,#5251,.T.);
#10580=EDGE_CURVE('',#8010,#8304,#5252,.T.);
#10581=EDGE_CURVE('',#8304,#8303,#5253,.T.);
#10582=EDGE_CURVE('',#8009,#8305,#5254,.T.);
#10583=EDGE_CURVE('',#8305,#8304,#5255,.T.);
#10584=EDGE_CURVE('',#8008,#8306,#5256,.T.);
#10585=EDGE_CURVE('',#8306,#8305,#5257,.T.);
#10586=EDGE_CURVE('',#8007,#8307,#5258,.T.);
#10587=EDGE_CURVE('',#8307,#8306,#5259,.T.);
#10588=EDGE_CURVE('',#8006,#8308,#5260,.T.);
#10589=EDGE_CURVE('',#8308,#8307,#5261,.T.);
#10590=EDGE_CURVE('',#8296,#8308,#5262,.T.);
#10591=EDGE_CURVE('',#7990,#8309,#5263,.T.);
#10592=EDGE_CURVE('',#8309,#8310,#5264,.T.);
#10593=EDGE_CURVE('',#7991,#8310,#5265,.T.);
#10594=EDGE_CURVE('',#8003,#8311,#5266,.T.);
#10595=EDGE_CURVE('',#8311,#8309,#5267,.T.);
#10596=EDGE_CURVE('',#8002,#8312,#5268,.T.);
#10597=EDGE_CURVE('',#8312,#8311,#5269,.T.);
#10598=EDGE_CURVE('',#8001,#8313,#5270,.T.);
#10599=EDGE_CURVE('',#8313,#8312,#5271,.T.);
#10600=EDGE_CURVE('',#8000,#8314,#5272,.T.);
#10601=EDGE_CURVE('',#8314,#8313,#5273,.T.);
#10602=EDGE_CURVE('',#7999,#8315,#5274,.T.);
#10603=EDGE_CURVE('',#8315,#8314,#5275,.T.);
#10604=EDGE_CURVE('',#7998,#8316,#5276,.T.);
#10605=EDGE_CURVE('',#8316,#8315,#5277,.T.);
#10606=EDGE_CURVE('',#7997,#8317,#5278,.T.);
#10607=EDGE_CURVE('',#8317,#8316,#5279,.T.);
#10608=EDGE_CURVE('',#7996,#8318,#5280,.T.);
#10609=EDGE_CURVE('',#8318,#8317,#5281,.T.);
#10610=EDGE_CURVE('',#7995,#8319,#5282,.T.);
#10611=EDGE_CURVE('',#8319,#8318,#5283,.T.);
#10612=EDGE_CURVE('',#7994,#8320,#5284,.T.);
#10613=EDGE_CURVE('',#8320,#8319,#5285,.T.);
#10614=EDGE_CURVE('',#7993,#8321,#5286,.T.);
#10615=EDGE_CURVE('',#8321,#8320,#5287,.T.);
#10616=EDGE_CURVE('',#7992,#8322,#5288,.T.);
#10617=EDGE_CURVE('',#8322,#8321,#5289,.T.);
#10618=EDGE_CURVE('',#8310,#8322,#5290,.T.);
#10619=EDGE_CURVE('',#7976,#8323,#5291,.T.);
#10620=EDGE_CURVE('',#8323,#8324,#5292,.T.);
#10621=EDGE_CURVE('',#7977,#8324,#5293,.T.);
#10622=EDGE_CURVE('',#7989,#8325,#5294,.T.);
#10623=EDGE_CURVE('',#8325,#8323,#5295,.T.);
#10624=EDGE_CURVE('',#7988,#8326,#5296,.T.);
#10625=EDGE_CURVE('',#8326,#8325,#5297,.T.);
#10626=EDGE_CURVE('',#7987,#8327,#5298,.T.);
#10627=EDGE_CURVE('',#8327,#8326,#5299,.T.);
#10628=EDGE_CURVE('',#7986,#8328,#5300,.T.);
#10629=EDGE_CURVE('',#8328,#8327,#5301,.T.);
#10630=EDGE_CURVE('',#7985,#8329,#5302,.T.);
#10631=EDGE_CURVE('',#8329,#8328,#5303,.T.);
#10632=EDGE_CURVE('',#7984,#8330,#5304,.T.);
#10633=EDGE_CURVE('',#8330,#8329,#5305,.T.);
#10634=EDGE_CURVE('',#7983,#8331,#5306,.T.);
#10635=EDGE_CURVE('',#8331,#8330,#5307,.T.);
#10636=EDGE_CURVE('',#7982,#8332,#5308,.T.);
#10637=EDGE_CURVE('',#8332,#8331,#5309,.T.);
#10638=EDGE_CURVE('',#7981,#8333,#5310,.T.);
#10639=EDGE_CURVE('',#8333,#8332,#5311,.T.);
#10640=EDGE_CURVE('',#7980,#8334,#5312,.T.);
#10641=EDGE_CURVE('',#8334,#8333,#5313,.T.);
#10642=EDGE_CURVE('',#7979,#8335,#5314,.T.);
#10643=EDGE_CURVE('',#8335,#8334,#5315,.T.);
#10644=EDGE_CURVE('',#7978,#8336,#5316,.T.);
#10645=EDGE_CURVE('',#8336,#8335,#5317,.T.);
#10646=EDGE_CURVE('',#8324,#8336,#5318,.T.);
#10647=EDGE_CURVE('',#8073,#8168,#5319,.T.);
#10648=EDGE_CURVE('',#8166,#7975,#5320,.T.);
#10649=EDGE_CURVE('',#8337,#8337,#3537,.T.);
#10650=EDGE_CURVE('',#8337,#8338,#5321,.T.);
#10651=EDGE_CURVE('',#8338,#8338,#3538,.T.);
#10652=EDGE_CURVE('',#8339,#8339,#3539,.T.);
#10653=EDGE_CURVE('',#8339,#8340,#5322,.T.);
#10654=EDGE_CURVE('',#8340,#8340,#3540,.T.);
#10655=EDGE_CURVE('',#8341,#8341,#3541,.T.);
#10656=EDGE_CURVE('',#8341,#8342,#5323,.T.);
#10657=EDGE_CURVE('',#8342,#8342,#3542,.T.);
#10658=EDGE_CURVE('',#8343,#8343,#3543,.T.);
#10659=EDGE_CURVE('',#8343,#8344,#5324,.T.);
#10660=EDGE_CURVE('',#8344,#8344,#3544,.T.);
#10661=EDGE_CURVE('',#8345,#8345,#3545,.T.);
#10662=EDGE_CURVE('',#8345,#8346,#5325,.T.);
#10663=EDGE_CURVE('',#8346,#8346,#3546,.T.);
#10664=EDGE_CURVE('',#8347,#8347,#3547,.T.);
#10665=EDGE_CURVE('',#8347,#8348,#5326,.T.);
#10666=EDGE_CURVE('',#8348,#8348,#3548,.T.);
#10667=EDGE_CURVE('',#8349,#8349,#3549,.T.);
#10668=EDGE_CURVE('',#8349,#8350,#5327,.T.);
#10669=EDGE_CURVE('',#8350,#8350,#3550,.T.);
#10670=EDGE_CURVE('',#8351,#8351,#3551,.T.);
#10671=EDGE_CURVE('',#8352,#8352,#3552,.T.);
#10672=EDGE_CURVE('',#8353,#8353,#3553,.T.);
#10673=EDGE_CURVE('',#8353,#8352,#5328,.T.);
#10674=EDGE_CURVE('',#8354,#8354,#3554,.T.);
#10675=EDGE_CURVE('',#8354,#8355,#5329,.T.);
#10676=EDGE_CURVE('',#8355,#8355,#3555,.T.);
#10677=EDGE_CURVE('',#8356,#8356,#3556,.T.);
#10678=EDGE_CURVE('',#8356,#8354,#5330,.T.);
#10679=EDGE_CURVE('',#8357,#8357,#3557,.T.);
#10680=EDGE_CURVE('',#8358,#8358,#3558,.T.);
#10681=EDGE_CURVE('',#8358,#8357,#5331,.T.);
#10682=EDGE_CURVE('',#8359,#8359,#3559,.T.);
#10683=EDGE_CURVE('',#8359,#8358,#5332,.T.);
#10684=EDGE_CURVE('',#8360,#8360,#3560,.T.);
#10685=EDGE_CURVE('',#8360,#8359,#5333,.T.);
#10686=EDGE_CURVE('',#8361,#8361,#3561,.T.);
#10687=EDGE_CURVE('',#8362,#8362,#3562,.T.);
#10688=EDGE_CURVE('',#8362,#8361,#5334,.T.);
#10689=EDGE_CURVE('',#8351,#8362,#5335,.T.);
#10690=EDGE_CURVE('',#8363,#8363,#3563,.T.);
#10691=EDGE_CURVE('',#8363,#8353,#5336,.T.);
#10692=EDGE_CURVE('',#8364,#8364,#3564,.T.);
#10693=EDGE_CURVE('',#8364,#8365,#5337,.T.);
#10694=EDGE_CURVE('',#8365,#8365,#3565,.T.);
#10695=EDGE_CURVE('',#8365,#8366,#5338,.T.);
#10696=EDGE_CURVE('',#8366,#8366,#3566,.T.);
#10697=EDGE_CURVE('',#8366,#8367,#5339,.T.);
#10698=EDGE_CURVE('',#8367,#8367,#3567,.T.);
#10699=EDGE_CURVE('',#8368,#8369,#4103,.T.);
#10700=EDGE_CURVE('',#8369,#8370,#4104,.T.);
#10701=EDGE_CURVE('',#8370,#8371,#4105,.T.);
#10702=EDGE_CURVE('',#8371,#8368,#4106,.T.);
#10703=EDGE_CURVE('',#8372,#8368,#5340,.T.);
#10704=EDGE_CURVE('',#8373,#8372,#4107,.T.);
#10705=EDGE_CURVE('',#8373,#8374,#5341,.T.);
#10706=EDGE_CURVE('',#8375,#8374,#4108,.T.);
#10707=EDGE_CURVE('',#8375,#8376,#5342,.T.);
#10708=EDGE_CURVE('',#8377,#8376,#4109,.T.);
#10709=EDGE_CURVE('',#8369,#8377,#5343,.T.);
#10710=EDGE_CURVE('',#8378,#8371,#5344,.T.);
#10711=EDGE_CURVE('',#8372,#8378,#4110,.T.);
#10712=EDGE_CURVE('',#8378,#8379,#4111,.T.);
#10713=EDGE_CURVE('',#8379,#8373,#4112,.T.);
#10714=EDGE_CURVE('',#8380,#8381,#4113,.T.);
#10715=EDGE_CURVE('',#8381,#8377,#4114,.T.);
#10716=EDGE_CURVE('',#8376,#8380,#4115,.T.);
#10717=EDGE_CURVE('',#8382,#8375,#4116,.T.);
#10718=EDGE_CURVE('',#8382,#8380,#5345,.T.);
#10719=EDGE_CURVE('',#8383,#8382,#4117,.T.);
#10720=EDGE_CURVE('',#8374,#8383,#4118,.T.);
#10721=EDGE_CURVE('',#8381,#8370,#5346,.T.);
#10722=EDGE_CURVE('',#8383,#8379,#5347,.T.);
#10723=EDGE_CURVE('',#8384,#8385,#1054,.T.);
#10724=EDGE_CURVE('',#8384,#8386,#4119,.T.);
#10725=EDGE_CURVE('',#8386,#8387,#3568,.T.);
#10726=EDGE_CURVE('',#8387,#8388,#4120,.T.);
#10727=EDGE_CURVE('',#8388,#8389,#4121,.T.);
#10728=EDGE_CURVE('',#8389,#8390,#4122,.T.);
#10729=EDGE_CURVE('',#8390,#8391,#3569,.T.);
#10730=EDGE_CURVE('',#8391,#8385,#4123,.T.);
#10731=EDGE_CURVE('',#8392,#8393,#4124,.F.);
#10732=EDGE_CURVE('',#8393,#8394,#3570,.T.);
#10733=EDGE_CURVE('',#8394,#8395,#4125,.F.);
#10734=EDGE_CURVE('',#8395,#8392,#3571,.T.);
#10735=EDGE_CURVE('',#8394,#8396,#4126,.T.);
#10736=EDGE_CURVE('',#8397,#8393,#4127,.T.);
#10737=EDGE_CURVE('',#8397,#8398,#4128,.T.);
#10738=EDGE_CURVE('',#8399,#8398,#3572,.T.);
#10739=EDGE_CURVE('',#8399,#8400,#4129,.T.);
#10740=EDGE_CURVE('',#8401,#8400,#4130,.T.);
#10741=EDGE_CURVE('',#8402,#8401,#3573,.T.);
#10742=EDGE_CURVE('',#8403,#8402,#4131,.T.);
#10743=EDGE_CURVE('',#8403,#8404,#4132,.T.);
#10744=EDGE_CURVE('',#8405,#8404,#3574,.T.);
#10745=EDGE_CURVE('',#8405,#8406,#4133,.T.);
#10746=EDGE_CURVE('',#8407,#8406,#4134,.T.);
#10747=EDGE_CURVE('',#8408,#8407,#3575,.T.);
#10748=EDGE_CURVE('',#8409,#8408,#4135,.T.);
#10749=EDGE_CURVE('',#8409,#8410,#4136,.T.);
#10750=EDGE_CURVE('',#8411,#8410,#3576,.T.);
#10751=EDGE_CURVE('',#8411,#8412,#4137,.T.);
#10752=EDGE_CURVE('',#8413,#8412,#4138,.T.);
#10753=EDGE_CURVE('',#8414,#8413,#3577,.T.);
#10754=EDGE_CURVE('',#8415,#8414,#4139,.T.);
#10755=EDGE_CURVE('',#8415,#8416,#4140,.T.);
#10756=EDGE_CURVE('',#8417,#8416,#3578,.T.);
#10757=EDGE_CURVE('',#8417,#8418,#4141,.T.);
#10758=EDGE_CURVE('',#8419,#8418,#4142,.T.);
#10759=EDGE_CURVE('',#8420,#8419,#3579,.T.);
#10760=EDGE_CURVE('',#8421,#8420,#4143,.T.);
#10761=EDGE_CURVE('',#8421,#8422,#4144,.T.);
#10762=EDGE_CURVE('',#8423,#8422,#3580,.T.);
#10763=EDGE_CURVE('',#8423,#8424,#4145,.T.);
#10764=EDGE_CURVE('',#8425,#8424,#4146,.T.);
#10765=EDGE_CURVE('',#8426,#8425,#3581,.T.);
#10766=EDGE_CURVE('',#8427,#8426,#4147,.T.);
#10767=EDGE_CURVE('',#8427,#8428,#4148,.T.);
#10768=EDGE_CURVE('',#8429,#8428,#3582,.T.);
#10769=EDGE_CURVE('',#8429,#8430,#4149,.T.);
#10770=EDGE_CURVE('',#8431,#8430,#4150,.T.);
#10771=EDGE_CURVE('',#8432,#8431,#3583,.T.);
#10772=EDGE_CURVE('',#8433,#8432,#4151,.T.);
#10773=EDGE_CURVE('',#8433,#8434,#4152,.T.);
#10774=EDGE_CURVE('',#8435,#8434,#3584,.T.);
#10775=EDGE_CURVE('',#8435,#8436,#5348,.T.);
#10776=EDGE_CURVE('',#8436,#8436,#3585,.T.);
#10777=EDGE_CURVE('',#8437,#8435,#3586,.T.);
#10778=EDGE_CURVE('',#8437,#8438,#4153,.T.);
#10779=EDGE_CURVE('',#8439,#8438,#4154,.T.);
#10780=EDGE_CURVE('',#8440,#8439,#3587,.T.);
#10781=EDGE_CURVE('',#8441,#8440,#4155,.T.);
#10782=EDGE_CURVE('',#8441,#8442,#4156,.T.);
#10783=EDGE_CURVE('',#8443,#8442,#3588,.T.);
#10784=EDGE_CURVE('',#8443,#8444,#4157,.T.);
#10785=EDGE_CURVE('',#8445,#8444,#4158,.T.);
#10786=EDGE_CURVE('',#8446,#8445,#3589,.T.);
#10787=EDGE_CURVE('',#8447,#8446,#4159,.T.);
#10788=EDGE_CURVE('',#8447,#8448,#4160,.T.);
#10789=EDGE_CURVE('',#8449,#8448,#3590,.T.);
#10790=EDGE_CURVE('',#8449,#8450,#4161,.T.);
#10791=EDGE_CURVE('',#8451,#8450,#4162,.T.);
#10792=EDGE_CURVE('',#8452,#8451,#3591,.T.);
#10793=EDGE_CURVE('',#8453,#8452,#4163,.T.);
#10794=EDGE_CURVE('',#8453,#8454,#4164,.T.);
#10795=EDGE_CURVE('',#8455,#8454,#3592,.T.);
#10796=EDGE_CURVE('',#8455,#8456,#4165,.T.);
#10797=EDGE_CURVE('',#8457,#8456,#4166,.T.);
#10798=EDGE_CURVE('',#8458,#8457,#3593,.T.);
#10799=EDGE_CURVE('',#8459,#8458,#4167,.T.);
#10800=EDGE_CURVE('',#8459,#8460,#4168,.T.);
#10801=EDGE_CURVE('',#8461,#8460,#3594,.T.);
#10802=EDGE_CURVE('',#8461,#8462,#4169,.T.);
#10803=EDGE_CURVE('',#8463,#8462,#4170,.T.);
#10804=EDGE_CURVE('',#8464,#8463,#3595,.T.);
#10805=EDGE_CURVE('',#8465,#8464,#4171,.T.);
#10806=EDGE_CURVE('',#8465,#8466,#4172,.T.);
#10807=EDGE_CURVE('',#8467,#8466,#3596,.T.);
#10808=EDGE_CURVE('',#8467,#8468,#4173,.T.);
#10809=EDGE_CURVE('',#8469,#8468,#4174,.T.);
#10810=EDGE_CURVE('',#8470,#8469,#3597,.T.);
#10811=EDGE_CURVE('',#8471,#8470,#4175,.T.);
#10812=EDGE_CURVE('',#8471,#8472,#4176,.T.);
#10813=EDGE_CURVE('',#8473,#8472,#3598,.T.);
#10814=EDGE_CURVE('',#8473,#8474,#4177,.T.);
#10815=EDGE_CURVE('',#8475,#8474,#4178,.T.);
#10816=EDGE_CURVE('',#8476,#8475,#3599,.T.);
#10817=EDGE_CURVE('',#8477,#8476,#4179,.T.);
#10818=EDGE_CURVE('',#8477,#8478,#4180,.T.);
#10819=EDGE_CURVE('',#8479,#8478,#3600,.T.);
#10820=EDGE_CURVE('',#8479,#8396,#4181,.T.);
#10821=EDGE_CURVE('',#8480,#8470,#4182,.F.);
#10822=EDGE_CURVE('',#8469,#8481,#4183,.F.);
#10823=EDGE_CURVE('',#8481,#8480,#3601,.T.);
#10824=EDGE_CURVE('',#8482,#8458,#4184,.F.);
#10825=EDGE_CURVE('',#8457,#8483,#4185,.F.);
#10826=EDGE_CURVE('',#8483,#8482,#3602,.T.);
#10827=EDGE_CURVE('',#8484,#8446,#4186,.F.);
#10828=EDGE_CURVE('',#8445,#8485,#4187,.F.);
#10829=EDGE_CURVE('',#8485,#8484,#3603,.T.);
#10830=EDGE_CURVE('',#8486,#8432,#4188,.F.);
#10831=EDGE_CURVE('',#8431,#8487,#4189,.F.);
#10832=EDGE_CURVE('',#8487,#8486,#3604,.T.);
#10833=EDGE_CURVE('',#8488,#8420,#4190,.F.);
#10834=EDGE_CURVE('',#8419,#8489,#4191,.F.);
#10835=EDGE_CURVE('',#8489,#8488,#3605,.T.);
#10836=EDGE_CURVE('',#8490,#8408,#4192,.F.);
#10837=EDGE_CURVE('',#8407,#8491,#4193,.F.);
#10838=EDGE_CURVE('',#8491,#8490,#3606,.T.);
#10839=EDGE_CURVE('',#8492,#8476,#4194,.F.);
#10840=EDGE_CURVE('',#8475,#8493,#4195,.F.);
#10841=EDGE_CURVE('',#8493,#8492,#3607,.T.);
#10842=EDGE_CURVE('',#8494,#8464,#4196,.F.);
#10843=EDGE_CURVE('',#8463,#8495,#4197,.F.);
#10844=EDGE_CURVE('',#8495,#8494,#3608,.T.);
#10845=EDGE_CURVE('',#8496,#8452,#4198,.F.);
#10846=EDGE_CURVE('',#8451,#8497,#4199,.F.);
#10847=EDGE_CURVE('',#8497,#8496,#3609,.T.);
#10848=EDGE_CURVE('',#8498,#8440,#4200,.F.);
#10849=EDGE_CURVE('',#8439,#8499,#4201,.F.);
#10850=EDGE_CURVE('',#8499,#8498,#3610,.T.);
#10851=EDGE_CURVE('',#8500,#8426,#4202,.F.);
#10852=EDGE_CURVE('',#8425,#8501,#4203,.F.);
#10853=EDGE_CURVE('',#8501,#8500,#3611,.T.);
#10854=EDGE_CURVE('',#8502,#8414,#4204,.F.);
#10855=EDGE_CURVE('',#8413,#8503,#4205,.F.);
#10856=EDGE_CURVE('',#8503,#8502,#3612,.T.);
#10857=EDGE_CURVE('',#8504,#8402,#4206,.F.);
#10858=EDGE_CURVE('',#8401,#8505,#4207,.F.);
#10859=EDGE_CURVE('',#8505,#8504,#3613,.T.);
#10860=EDGE_CURVE('',#8506,#8506,#3614,.T.);
#10861=EDGE_CURVE('',#8506,#8507,#5349,.T.);
#10862=EDGE_CURVE('',#8507,#8508,#3615,.T.);
#10863=EDGE_CURVE('',#8508,#8507,#3616,.T.);
#10864=EDGE_CURVE('',#8509,#8510,#3617,.T.);
#10865=EDGE_CURVE('',#8510,#8509,#3618,.T.);
#10866=EDGE_CURVE('',#8510,#8508,#5350,.T.);
#10867=EDGE_CURVE('',#8511,#8511,#3619,.T.);
#10868=EDGE_CURVE('',#8509,#8512,#5351,.T.);
#10869=EDGE_CURVE('',#8512,#8512,#3620,.T.);
#10870=EDGE_CURVE('',#8513,#8513,#3621,.T.);
#10871=EDGE_CURVE('',#8514,#8392,#4208,.T.);
#10872=EDGE_CURVE('',#8515,#8514,#4209,.T.);
#10873=EDGE_CURVE('',#8516,#8515,#4210,.T.);
#10874=EDGE_CURVE('',#8398,#8516,#4211,.T.);
#10875=EDGE_CURVE('',#8517,#8515,#4212,.T.);
#10876=EDGE_CURVE('',#8517,#8518,#4213,.T.);
#10877=EDGE_CURVE('',#8518,#8516,#3622,.T.);
#10878=EDGE_CURVE('',#8518,#8399,#4214,.T.);
#10879=EDGE_CURVE('',#8519,#8517,#4215,.T.);
#10880=EDGE_CURVE('',#8505,#8519,#4216,.T.);
#10881=EDGE_CURVE('',#8520,#8519,#3623,.T.);
#10882=EDGE_CURVE('',#8520,#8504,#4217,.T.);
#10883=EDGE_CURVE('',#8521,#8490,#4218,.T.);
#10884=EDGE_CURVE('',#8522,#8521,#4219,.T.);
#10885=EDGE_CURVE('',#8523,#8522,#4220,.T.);
#10886=EDGE_CURVE('',#8410,#8523,#4221,.T.);
#10887=EDGE_CURVE('',#8524,#8522,#4222,.T.);
#10888=EDGE_CURVE('',#8524,#8525,#4223,.T.);
#10889=EDGE_CURVE('',#8525,#8523,#3624,.T.);
#10890=EDGE_CURVE('',#8525,#8411,#4224,.T.);
#10891=EDGE_CURVE('',#8526,#8524,#4225,.T.);
#10892=EDGE_CURVE('',#8503,#8526,#4226,.T.);
#10893=EDGE_CURVE('',#8527,#8526,#3625,.T.);
#10894=EDGE_CURVE('',#8527,#8502,#4227,.T.);
#10895=EDGE_CURVE('',#8528,#8488,#4228,.T.);
#10896=EDGE_CURVE('',#8529,#8528,#4229,.T.);
#10897=EDGE_CURVE('',#8530,#8529,#4230,.T.);
#10898=EDGE_CURVE('',#8422,#8530,#4231,.T.);
#10899=EDGE_CURVE('',#8531,#8529,#4232,.T.);
#10900=EDGE_CURVE('',#8531,#8532,#4233,.T.);
#10901=EDGE_CURVE('',#8532,#8530,#3626,.T.);
#10902=EDGE_CURVE('',#8532,#8423,#4234,.T.);
#10903=EDGE_CURVE('',#8533,#8531,#4235,.T.);
#10904=EDGE_CURVE('',#8501,#8533,#4236,.T.);
#10905=EDGE_CURVE('',#8534,#8533,#3627,.T.);
#10906=EDGE_CURVE('',#8534,#8500,#4237,.T.);
#10907=EDGE_CURVE('',#8535,#8486,#4238,.T.);
#10908=EDGE_CURVE('',#8536,#8535,#4239,.T.);
#10909=EDGE_CURVE('',#8537,#8536,#4240,.T.);
#10910=EDGE_CURVE('',#8434,#8537,#4241,.T.);
#10911=EDGE_CURVE('',#8538,#8536,#4242,.T.);
#10912=EDGE_CURVE('',#8538,#8539,#4243,.T.);
#10913=EDGE_CURVE('',#8539,#8537,#3628,.T.);
#10914=EDGE_CURVE('',#8539,#8437,#4244,.T.);
#10915=EDGE_CURVE('',#8540,#8538,#4245,.T.);
#10916=EDGE_CURVE('',#8499,#8540,#4246,.T.);
#10917=EDGE_CURVE('',#8541,#8540,#3629,.T.);
#10918=EDGE_CURVE('',#8541,#8498,#4247,.T.);
#10919=EDGE_CURVE('',#8542,#8484,#4248,.T.);
#10920=EDGE_CURVE('',#8543,#8542,#4249,.T.);
#10921=EDGE_CURVE('',#8544,#8543,#4250,.T.);
#10922=EDGE_CURVE('',#8448,#8544,#4251,.T.);
#10923=EDGE_CURVE('',#8545,#8543,#4252,.T.);
#10924=EDGE_CURVE('',#8545,#8546,#4253,.T.);
#10925=EDGE_CURVE('',#8546,#8544,#3630,.T.);
#10926=EDGE_CURVE('',#8546,#8449,#4254,.T.);
#10927=EDGE_CURVE('',#8547,#8545,#4255,.T.);
#10928=EDGE_CURVE('',#8497,#8547,#4256,.T.);
#10929=EDGE_CURVE('',#8548,#8547,#3631,.T.);
#10930=EDGE_CURVE('',#8548,#8496,#4257,.T.);
#10931=EDGE_CURVE('',#8549,#8482,#4258,.T.);
#10932=EDGE_CURVE('',#8550,#8549,#4259,.T.);
#10933=EDGE_CURVE('',#8551,#8550,#4260,.T.);
#10934=EDGE_CURVE('',#8460,#8551,#4261,.T.);
#10935=EDGE_CURVE('',#8552,#8550,#4262,.T.);
#10936=EDGE_CURVE('',#8552,#8553,#4263,.T.);
#10937=EDGE_CURVE('',#8553,#8551,#3632,.T.);
#10938=EDGE_CURVE('',#8553,#8461,#4264,.T.);
#10939=EDGE_CURVE('',#8554,#8552,#4265,.T.);
#10940=EDGE_CURVE('',#8495,#8554,#4266,.T.);
#10941=EDGE_CURVE('',#8555,#8554,#3633,.T.);
#10942=EDGE_CURVE('',#8555,#8494,#4267,.T.);
#10943=EDGE_CURVE('',#8390,#8480,#4268,.T.);
#10944=EDGE_CURVE('',#8556,#8389,#4269,.T.);
#10945=EDGE_CURVE('',#8472,#8556,#4270,.T.);
#10946=EDGE_CURVE('',#8388,#8557,#4271,.T.);
#10947=EDGE_CURVE('',#8557,#8556,#3634,.T.);
#10948=EDGE_CURVE('',#8557,#8473,#4272,.T.);
#10949=EDGE_CURVE('',#8493,#8387,#4273,.T.);
#10950=EDGE_CURVE('',#8386,#8492,#4274,.T.);
#10951=EDGE_CURVE('',#8558,#8520,#4275,.T.);
#10952=EDGE_CURVE('',#8559,#8558,#4276,.T.);
#10953=EDGE_CURVE('',#8560,#8559,#4277,.T.);
#10954=EDGE_CURVE('',#8404,#8560,#4278,.T.);
#10955=EDGE_CURVE('',#8561,#8558,#4279,.T.);
#10956=EDGE_CURVE('',#8561,#8562,#4280,.T.);
#10957=EDGE_CURVE('',#8562,#8559,#3635,.T.);
#10958=EDGE_CURVE('',#8562,#8405,#4281,.T.);
#10959=EDGE_CURVE('',#8563,#8561,#4282,.T.);
#10960=EDGE_CURVE('',#8491,#8563,#4283,.T.);
#10961=EDGE_CURVE('',#8521,#8563,#3636,.T.);
#10962=EDGE_CURVE('',#8564,#8527,#4284,.T.);
#10963=EDGE_CURVE('',#8565,#8564,#4285,.T.);
#10964=EDGE_CURVE('',#8566,#8565,#4286,.T.);
#10965=EDGE_CURVE('',#8416,#8566,#4287,.T.);
#10966=EDGE_CURVE('',#8567,#8564,#4288,.T.);
#10967=EDGE_CURVE('',#8567,#8568,#4289,.T.);
#10968=EDGE_CURVE('',#8568,#8565,#3637,.T.);
#10969=EDGE_CURVE('',#8568,#8417,#4290,.T.);
#10970=EDGE_CURVE('',#8569,#8567,#4291,.T.);
#10971=EDGE_CURVE('',#8489,#8569,#4292,.T.);
#10972=EDGE_CURVE('',#8528,#8569,#3638,.T.);
#10973=EDGE_CURVE('',#8570,#8534,#4293,.T.);
#10974=EDGE_CURVE('',#8571,#8570,#4294,.T.);
#10975=EDGE_CURVE('',#8572,#8571,#4295,.T.);
#10976=EDGE_CURVE('',#8428,#8572,#4296,.T.);
#10977=EDGE_CURVE('',#8573,#8570,#4297,.T.);
#10978=EDGE_CURVE('',#8573,#8574,#4298,.T.);
#10979=EDGE_CURVE('',#8574,#8571,#3639,.T.);
#10980=EDGE_CURVE('',#8574,#8429,#4299,.T.);
#10981=EDGE_CURVE('',#8575,#8573,#4300,.T.);
#10982=EDGE_CURVE('',#8487,#8575,#4301,.T.);
#10983=EDGE_CURVE('',#8535,#8575,#3640,.T.);
#10984=EDGE_CURVE('',#8576,#8541,#4302,.T.);
#10985=EDGE_CURVE('',#8577,#8576,#4303,.T.);
#10986=EDGE_CURVE('',#8578,#8577,#4304,.T.);
#10987=EDGE_CURVE('',#8442,#8578,#4305,.T.);
#10988=EDGE_CURVE('',#8579,#8576,#4306,.T.);
#10989=EDGE_CURVE('',#8579,#8580,#4307,.T.);
#10990=EDGE_CURVE('',#8580,#8577,#3641,.T.);
#10991=EDGE_CURVE('',#8580,#8443,#4308,.T.);
#10992=EDGE_CURVE('',#8581,#8579,#4309,.T.);
#10993=EDGE_CURVE('',#8485,#8581,#4310,.T.);
#10994=EDGE_CURVE('',#8542,#8581,#3642,.T.);
#10995=EDGE_CURVE('',#8582,#8548,#4311,.T.);
#10996=EDGE_CURVE('',#8583,#8582,#4312,.T.);
#10997=EDGE_CURVE('',#8584,#8583,#4313,.T.);
#10998=EDGE_CURVE('',#8454,#8584,#4314,.T.);
#10999=EDGE_CURVE('',#8585,#8582,#4315,.T.);
#11000=EDGE_CURVE('',#8585,#8586,#4316,.T.);
#11001=EDGE_CURVE('',#8586,#8583,#3643,.T.);
#11002=EDGE_CURVE('',#8586,#8455,#4317,.T.);
#11003=EDGE_CURVE('',#8587,#8585,#4318,.T.);
#11004=EDGE_CURVE('',#8483,#8587,#4319,.T.);
#11005=EDGE_CURVE('',#8549,#8587,#3644,.T.);
#11006=EDGE_CURVE('',#8588,#8555,#4320,.T.);
#11007=EDGE_CURVE('',#8589,#8588,#4321,.T.);
#11008=EDGE_CURVE('',#8590,#8589,#4322,.T.);
#11009=EDGE_CURVE('',#8466,#8590,#4323,.T.);
#11010=EDGE_CURVE('',#8591,#8588,#4324,.T.);
#11011=EDGE_CURVE('',#8592,#8591,#4325,.T.);
#11012=EDGE_CURVE('',#8592,#8593,#4326,.T.);
#11013=EDGE_CURVE('',#8593,#8589,#3645,.T.);
#11014=EDGE_CURVE('',#8593,#8467,#4327,.T.);
#11015=EDGE_CURVE('',#8385,#8592,#4328,.T.);
#11016=EDGE_CURVE('',#8481,#8391,#4329,.T.);
#11017=EDGE_CURVE('',#8591,#8594,#1055,.T.);
#11018=EDGE_CURVE('',#8595,#8594,#3646,.T.);
#11019=EDGE_CURVE('',#8594,#8595,#3647,.T.);
#11020=EDGE_CURVE('',#8514,#8596,#3648,.T.);
#11021=EDGE_CURVE('',#8596,#8597,#4330,.T.);
#11022=EDGE_CURVE('',#8597,#8598,#4331,.T.);
#11023=EDGE_CURVE('',#8598,#8384,#4332,.T.);
#11024=EDGE_CURVE('',#8599,#8598,#4333,.T.);
#11025=EDGE_CURVE('',#8600,#8599,#4334,.T.);
#11026=EDGE_CURVE('',#8478,#8600,#4335,.T.);
#11027=EDGE_CURVE('',#8597,#8601,#4336,.T.);
#11028=EDGE_CURVE('',#8601,#8599,#3649,.T.);
#11029=EDGE_CURVE('',#8601,#8479,#4337,.T.);
#11030=EDGE_CURVE('',#8395,#8596,#4338,.T.);
#11031=EDGE_CURVE('',#8436,#8511,#5352,.T.);
#11032=EDGE_CURVE('',#8602,#8602,#3650,.T.);
#11033=EDGE_CURVE('',#8602,#8595,#5353,.T.);
#11034=EDGE_CURVE('',#8603,#8603,#3651,.T.);
#11035=EDGE_CURVE('',#8603,#8602,#5354,.T.);
#11036=EDGE_CURVE('',#8513,#8603,#5355,.T.);
#11037=EDGE_CURVE('',#8604,#8605,#4339,.T.);
#11038=EDGE_CURVE('',#8605,#8606,#5356,.T.);
#11039=EDGE_CURVE('',#8606,#8607,#5357,.F.);
#11040=EDGE_CURVE('',#8607,#8608,#5358,.T.);
#11041=EDGE_CURVE('',#8608,#8604,#4340,.T.);
#11042=EDGE_CURVE('',#8609,#8605,#4341,.T.);
#11043=EDGE_CURVE('',#8610,#8609,#5359,.T.);
#11044=EDGE_CURVE('',#8606,#8610,#5360,.T.);
#11045=EDGE_CURVE('',#8611,#8604,#4342,.T.);
#11046=EDGE_CURVE('',#8611,#8612,#4343,.T.);
#11047=EDGE_CURVE('',#8612,#8613,#4344,.T.);
#11048=EDGE_CURVE('',#8613,#8609,#4345,.T.);
#11049=EDGE_CURVE('',#8614,#8615,#4346,.T.);
#11050=EDGE_CURVE('',#8615,#8616,#5361,.T.);
#11051=EDGE_CURVE('',#8616,#8617,#5362,.F.);
#11052=EDGE_CURVE('',#8617,#8618,#5363,.T.);
#11053=EDGE_CURVE('',#8618,#8614,#4347,.T.);
#11054=EDGE_CURVE('',#8619,#8615,#4348,.T.);
#11055=EDGE_CURVE('',#8620,#8619,#5364,.T.);
#11056=EDGE_CURVE('',#8616,#8620,#5365,.T.);
#11057=EDGE_CURVE('',#8621,#8614,#4349,.T.);
#11058=EDGE_CURVE('',#8621,#8622,#4350,.T.);
#11059=EDGE_CURVE('',#8622,#8623,#4351,.T.);
#11060=EDGE_CURVE('',#8623,#8619,#4352,.T.);
#11061=EDGE_CURVE('',#8624,#8625,#4353,.T.);
#11062=EDGE_CURVE('',#8625,#8626,#5366,.T.);
#11063=EDGE_CURVE('',#8626,#8627,#5367,.F.);
#11064=EDGE_CURVE('',#8627,#8628,#5368,.T.);
#11065=EDGE_CURVE('',#8628,#8624,#4354,.T.);
#11066=EDGE_CURVE('',#8629,#8625,#4355,.T.);
#11067=EDGE_CURVE('',#8630,#8629,#5369,.T.);
#11068=EDGE_CURVE('',#8626,#8630,#5370,.T.);
#11069=EDGE_CURVE('',#8631,#8624,#4356,.T.);
#11070=EDGE_CURVE('',#8631,#8632,#4357,.T.);
#11071=EDGE_CURVE('',#8632,#8633,#4358,.T.);
#11072=EDGE_CURVE('',#8633,#8629,#4359,.T.);
#11073=EDGE_CURVE('',#8634,#8635,#1056,.T.);
#11074=EDGE_CURVE('',#8635,#8636,#5371,.T.);
#11075=EDGE_CURVE('',#8636,#8637,#5372,.F.);
#11076=EDGE_CURVE('',#8637,#8634,#5373,.T.);
#11077=EDGE_CURVE('',#8635,#8638,#1057,.T.);
#11078=EDGE_CURVE('',#8638,#8639,#1058,.T.);
#11079=EDGE_CURVE('',#8640,#8639,#4360,.F.);
#11080=EDGE_CURVE('',#8641,#8640,#5374,.T.);
#11081=EDGE_CURVE('',#8636,#8641,#5375,.T.);
#11082=EDGE_CURVE('',#8642,#8634,#1059,.T.);
#11083=EDGE_CURVE('',#8643,#8642,#1060,.T.);
#11084=EDGE_CURVE('',#8644,#8643,#1061,.T.);
#11085=EDGE_CURVE('',#8645,#8644,#1062,.T.);
#11086=EDGE_CURVE('',#8646,#8645,#1063,.T.);
#11087=EDGE_CURVE('',#8647,#8646,#4361,.T.);
#11088=EDGE_CURVE('',#8648,#8647,#4362,.T.);
#11089=EDGE_CURVE('',#8649,#8648,#4363,.T.);
#11090=EDGE_CURVE('',#8650,#8649,#3652,.T.);
#11091=EDGE_CURVE('',#8632,#8650,#4364,.T.);
#11092=EDGE_CURVE('',#8639,#8631,#4365,.T.);
#11093=EDGE_CURVE('',#8643,#8651,#5376,.T.);
#11094=EDGE_CURVE('',#8651,#8652,#5377,.F.);
#11095=EDGE_CURVE('',#8652,#8644,#5378,.T.);
#11096=EDGE_CURVE('',#8653,#8642,#5379,.T.);
#11097=EDGE_CURVE('',#8651,#8653,#5380,.T.);
#11098=EDGE_CURVE('',#8654,#8655,#4366,.T.);
#11099=EDGE_CURVE('',#8655,#8656,#5381,.T.);
#11100=EDGE_CURVE('',#8656,#8657,#5382,.F.);
#11101=EDGE_CURVE('',#8657,#8658,#5383,.T.);
#11102=EDGE_CURVE('',#8658,#8654,#4367,.T.);
#11103=EDGE_CURVE('',#8659,#8655,#4368,.T.);
#11104=EDGE_CURVE('',#8660,#8659,#5384,.T.);
#11105=EDGE_CURVE('',#8656,#8660,#5385,.T.);
#11106=EDGE_CURVE('',#8654,#8661,#4369,.T.);
#11107=EDGE_CURVE('',#8661,#8662,#4370,.T.);
#11108=EDGE_CURVE('',#8662,#8663,#4371,.T.);
#11109=EDGE_CURVE('',#8659,#8663,#4372,.T.);
#11110=EDGE_CURVE('',#8658,#8664,#4373,.T.);
#11111=EDGE_CURVE('',#8664,#8665,#4374,.T.);
#11112=EDGE_CURVE('',#8666,#8665,#4375,.T.);
#11113=EDGE_CURVE('',#8666,#8661,#4376,.T.);
#11114=EDGE_CURVE('',#8667,#8668,#4377,.T.);
#11115=EDGE_CURVE('',#8668,#8669,#5386,.T.);
#11116=EDGE_CURVE('',#8669,#8670,#5387,.F.);
#11117=EDGE_CURVE('',#8670,#8671,#5388,.T.);
#11118=EDGE_CURVE('',#8671,#8667,#4378,.T.);
#11119=EDGE_CURVE('',#8664,#8668,#4379,.T.);
#11120=EDGE_CURVE('',#8672,#8664,#5389,.T.);
#11121=EDGE_CURVE('',#8669,#8672,#5390,.T.);
#11122=EDGE_CURVE('',#8667,#8673,#4380,.T.);
#11123=EDGE_CURVE('',#8673,#8674,#4381,.T.);
#11124=EDGE_CURVE('',#8674,#8665,#4382,.T.);
#11125=EDGE_CURVE('',#8671,#8675,#4383,.T.);
#11126=EDGE_CURVE('',#8675,#8676,#4384,.T.);
#11127=EDGE_CURVE('',#8677,#8676,#4385,.T.);
#11128=EDGE_CURVE('',#8677,#8673,#4386,.T.);
#11129=EDGE_CURVE('',#8678,#8679,#4387,.T.);
#11130=EDGE_CURVE('',#8679,#8680,#5391,.T.);
#11131=EDGE_CURVE('',#8680,#8681,#5392,.F.);
#11132=EDGE_CURVE('',#8681,#8682,#5393,.T.);
#11133=EDGE_CURVE('',#8682,#8678,#4388,.T.);
#11134=EDGE_CURVE('',#8675,#8679,#4389,.T.);
#11135=EDGE_CURVE('',#8683,#8675,#5394,.T.);
#11136=EDGE_CURVE('',#8680,#8683,#5395,.T.);
#11137=EDGE_CURVE('',#8684,#8678,#4390,.T.);
#11138=EDGE_CURVE('',#8684,#8685,#4391,.T.);
#11139=EDGE_CURVE('',#8685,#8676,#4392,.T.);
#11140=EDGE_CURVE('',#8686,#8687,#4393,.T.);
#11141=EDGE_CURVE('',#8687,#8688,#5396,.T.);
#11142=EDGE_CURVE('',#8688,#8689,#5397,.F.);
#11143=EDGE_CURVE('',#8689,#8690,#5398,.T.);
#11144=EDGE_CURVE('',#8690,#8686,#4394,.T.);
#11145=EDGE_CURVE('',#8691,#8687,#4395,.T.);
#11146=EDGE_CURVE('',#8692,#8691,#5399,.T.);
#11147=EDGE_CURVE('',#8688,#8692,#5400,.T.);
#11148=EDGE_CURVE('',#8686,#8647,#4396,.T.);
#11149=EDGE_CURVE('',#8646,#8691,#4397,.F.);
#11150=EDGE_CURVE('',#8690,#8693,#4398,.T.);
#11151=EDGE_CURVE('',#8693,#8694,#4399,.T.);
#11152=EDGE_CURVE('',#8648,#8694,#4400,.T.);
#11153=EDGE_CURVE('',#8695,#8696,#4401,.T.);
#11154=EDGE_CURVE('',#8696,#8697,#5401,.T.);
#11155=EDGE_CURVE('',#8697,#8698,#5402,.F.);
#11156=EDGE_CURVE('',#8698,#8699,#5403,.T.);
#11157=EDGE_CURVE('',#8699,#8695,#4402,.T.);
#11158=EDGE_CURVE('',#8693,#8696,#4403,.T.);
#11159=EDGE_CURVE('',#8700,#8693,#5404,.T.);
#11160=EDGE_CURVE('',#8697,#8700,#5405,.T.);
#11161=EDGE_CURVE('',#8695,#8701,#4404,.T.);
#11162=EDGE_CURVE('',#8701,#8702,#4405,.T.);
#11163=EDGE_CURVE('',#8702,#8694,#4406,.T.);
#11164=EDGE_CURVE('',#8699,#8703,#4407,.T.);
#11165=EDGE_CURVE('',#8703,#8704,#4408,.T.);
#11166=EDGE_CURVE('',#8705,#8704,#4409,.T.);
#11167=EDGE_CURVE('',#8705,#8701,#4410,.T.);
#11168=EDGE_CURVE('',#8706,#8707,#4411,.T.);
#11169=EDGE_CURVE('',#8707,#8708,#5406,.T.);
#11170=EDGE_CURVE('',#8708,#8709,#5407,.F.);
#11171=EDGE_CURVE('',#8709,#8710,#5408,.T.);
#11172=EDGE_CURVE('',#8710,#8706,#4412,.T.);
#11173=EDGE_CURVE('',#8703,#8707,#4413,.T.);
#11174=EDGE_CURVE('',#8711,#8703,#5409,.T.);
#11175=EDGE_CURVE('',#8708,#8711,#5410,.T.);
#11176=EDGE_CURVE('',#8706,#8712,#4414,.T.);
#11177=EDGE_CURVE('',#8712,#8713,#4415,.T.);
#11178=EDGE_CURVE('',#8713,#8704,#4416,.T.);
#11179=EDGE_CURVE('',#8710,#8714,#4417,.T.);
#11180=EDGE_CURVE('',#8714,#8715,#4418,.T.);
#11181=EDGE_CURVE('',#8716,#8715,#4419,.T.);
#11182=EDGE_CURVE('',#8716,#8712,#4420,.T.);
#11183=EDGE_CURVE('',#8717,#8718,#4421,.T.);
#11184=EDGE_CURVE('',#8718,#8719,#5411,.T.);
#11185=EDGE_CURVE('',#8719,#8720,#5412,.F.);
#11186=EDGE_CURVE('',#8720,#8721,#5413,.T.);
#11187=EDGE_CURVE('',#8721,#8717,#4422,.T.);
#11188=EDGE_CURVE('',#8714,#8718,#4423,.T.);
#11189=EDGE_CURVE('',#8722,#8714,#5414,.T.);
#11190=EDGE_CURVE('',#8719,#8722,#5415,.T.);
#11191=EDGE_CURVE('',#8717,#8723,#4424,.T.);
#11192=EDGE_CURVE('',#8723,#8724,#4425,.T.);
#11193=EDGE_CURVE('',#8724,#8715,#4426,.T.);
#11194=EDGE_CURVE('',#8721,#8659,#4427,.T.);
#11195=EDGE_CURVE('',#8725,#8663,#4428,.T.);
#11196=EDGE_CURVE('',#8725,#8723,#4429,.T.);
#11197=EDGE_CURVE('',#8685,#8726,#4430,.T.);
#11198=EDGE_CURVE('',#8726,#8727,#4431,.T.);
#11199=EDGE_CURVE('',#8676,#8727,#4432,.T.);
#11200=EDGE_CURVE('',#8674,#8728,#4433,.T.);
#11201=EDGE_CURVE('',#8728,#8729,#4434,.T.);
#11202=EDGE_CURVE('',#8665,#8729,#4435,.T.);
#11203=EDGE_CURVE('',#8662,#8730,#4436,.T.);
#11204=EDGE_CURVE('',#8730,#8731,#4437,.T.);
#11205=EDGE_CURVE('',#8663,#8731,#4438,.T.);
#11206=EDGE_CURVE('',#8724,#8732,#4439,.T.);
#11207=EDGE_CURVE('',#8732,#8733,#4440,.T.);
#11208=EDGE_CURVE('',#8715,#8733,#4441,.T.);
#11209=EDGE_CURVE('',#8713,#8734,#4442,.T.);
#11210=EDGE_CURVE('',#8734,#8735,#4443,.T.);
#11211=EDGE_CURVE('',#8704,#8735,#4444,.T.);
#11212=EDGE_CURVE('',#8702,#8736,#4445,.T.);
#11213=EDGE_CURVE('',#8736,#8737,#4446,.T.);
#11214=EDGE_CURVE('',#8694,#8737,#4447,.T.);
#11215=EDGE_CURVE('',#8682,#8609,#4448,.T.);
#11216=EDGE_CURVE('',#8738,#8613,#4449,.T.);
#11217=EDGE_CURVE('',#8738,#8684,#4450,.T.);
#11218=EDGE_CURVE('',#8612,#8739,#4451,.T.);
#11219=EDGE_CURVE('',#8739,#8740,#4452,.T.);
#11220=EDGE_CURVE('',#8740,#8613,#4453,.T.);
#11221=EDGE_CURVE('',#8608,#8619,#4454,.T.);
#11222=EDGE_CURVE('',#8741,#8623,#4455,.T.);
#11223=EDGE_CURVE('',#8741,#8611,#4456,.T.);
#11224=EDGE_CURVE('',#8622,#8742,#4457,.T.);
#11225=EDGE_CURVE('',#8742,#8743,#4458,.T.);
#11226=EDGE_CURVE('',#8743,#8623,#4459,.T.);
#11227=EDGE_CURVE('',#8618,#8629,#4460,.T.);
#11228=EDGE_CURVE('',#8744,#8633,#4461,.T.);
#11229=EDGE_CURVE('',#8744,#8621,#4462,.T.);
#11230=EDGE_CURVE('',#8650,#8745,#4463,.T.);
#11231=EDGE_CURVE('',#8745,#8633,#4464,.T.);
#11232=EDGE_CURVE('',#8628,#8640,#4465,.T.);
#11233=EDGE_CURVE('',#8745,#8746,#4466,.T.);
#11234=EDGE_CURVE('',#8746,#8744,#4467,.T.);
#11235=EDGE_CURVE('',#8743,#8747,#4468,.T.);
#11236=EDGE_CURVE('',#8747,#8741,#4469,.T.);
#11237=EDGE_CURVE('',#8740,#8748,#4470,.T.);
#11238=EDGE_CURVE('',#8748,#8738,#4471,.T.);
#11239=EDGE_CURVE('',#8737,#8649,#4472,.T.);
#11240=EDGE_CURVE('',#8735,#8749,#4473,.T.);
#11241=EDGE_CURVE('',#8749,#8705,#4474,.T.);
#11242=EDGE_CURVE('',#8733,#8750,#4475,.T.);
#11243=EDGE_CURVE('',#8750,#8716,#4476,.T.);
#11244=EDGE_CURVE('',#8731,#8751,#4477,.T.);
#11245=EDGE_CURVE('',#8751,#8725,#4478,.T.);
#11246=EDGE_CURVE('',#8729,#8752,#4479,.T.);
#11247=EDGE_CURVE('',#8752,#8666,#4480,.T.);
#11248=EDGE_CURVE('',#8727,#8753,#4481,.T.);
#11249=EDGE_CURVE('',#8753,#8677,#4482,.T.);
#11250=EDGE_CURVE('',#8660,#8720,#5416,.T.);
#11251=EDGE_CURVE('',#8722,#8709,#5417,.T.);
#11252=EDGE_CURVE('',#8711,#8698,#5418,.T.);
#11253=EDGE_CURVE('',#8700,#8689,#5419,.T.);
#11254=EDGE_CURVE('',#8736,#8749,#3653,.T.);
#11255=EDGE_CURVE('',#8734,#8750,#3654,.T.);
#11256=EDGE_CURVE('',#8732,#8751,#3655,.T.);
#11257=EDGE_CURVE('',#8730,#8752,#3656,.T.);
#11258=EDGE_CURVE('',#8728,#8753,#3657,.T.);
#11259=EDGE_CURVE('',#8726,#8748,#3658,.T.);
#11260=EDGE_CURVE('',#8739,#8747,#3659,.T.);
#11261=EDGE_CURVE('',#8742,#8746,#3660,.T.);
#11262=EDGE_CURVE('',#8754,#8754,#3661,.T.);
#11263=EDGE_CURVE('',#8755,#8755,#3662,.T.);
#11264=EDGE_CURVE('',#8755,#8754,#5420,.T.);
#11265=EDGE_CURVE('',#8756,#8756,#3663,.T.);
#11266=EDGE_CURVE('',#8756,#8757,#5421,.T.);
#11267=EDGE_CURVE('',#8757,#8757,#3664,.T.);
#11268=EDGE_CURVE('',#8683,#8670,#5422,.T.);
#11269=EDGE_CURVE('',#8672,#8657,#5423,.T.);
#11270=EDGE_CURVE('',#8692,#8652,#5424,.T.);
#11271=EDGE_CURVE('',#8653,#8637,#5425,.T.);
#11272=EDGE_CURVE('',#8641,#8627,#5426,.T.);
#11273=EDGE_CURVE('',#8630,#8617,#5427,.T.);
#11274=EDGE_CURVE('',#8620,#8607,#5428,.T.);
#11275=EDGE_CURVE('',#8610,#8681,#5429,.T.);
#11276=EDGE_CURVE('',#8755,#8757,#5430,.T.);
#11277=EDGE_CURVE('',#8758,#8758,#3665,.T.);
#11278=EDGE_CURVE('',#8759,#8759,#3666,.T.);
#11279=EDGE_CURVE('',#8759,#8758,#5431,.T.);
#11280=EDGE_CURVE('',#8760,#8760,#3667,.T.);
#11281=EDGE_CURVE('',#8760,#8759,#5432,.T.);
#11282=EDGE_CURVE('',#8761,#8761,#3668,.T.);
#11283=EDGE_CURVE('',#8761,#8760,#5433,.T.);
#11284=EDGE_CURVE('',#8762,#8763,#3669,.T.);
#11285=EDGE_CURVE('',#8762,#8763,#3670,.T.);
#11286=EDGE_CURVE('',#8764,#8762,#5434,.T.);
#11287=EDGE_CURVE('',#8764,#8765,#3671,.T.);
#11288=EDGE_CURVE('',#8763,#8765,#5435,.T.);
#11289=EDGE_CURVE('',#8765,#8764,#3672,.T.);
#11290=EDGE_CURVE('',#8766,#8767,#3673,.T.);
#11291=EDGE_CURVE('',#8766,#8767,#3674,.T.);
#11292=EDGE_CURVE('',#8768,#8766,#5436,.T.);
#11293=EDGE_CURVE('',#8768,#8769,#3675,.T.);
#11294=EDGE_CURVE('',#8767,#8769,#5437,.T.);
#11295=EDGE_CURVE('',#8769,#8768,#3676,.T.);
#11296=EDGE_CURVE('',#8770,#8771,#3677,.T.);
#11297=EDGE_CURVE('',#8770,#8771,#3678,.T.);
#11298=EDGE_CURVE('',#8772,#8770,#5438,.T.);
#11299=EDGE_CURVE('',#8772,#8773,#3679,.T.);
#11300=EDGE_CURVE('',#8771,#8773,#5439,.T.);
#11301=EDGE_CURVE('',#8773,#8772,#3680,.T.);
#11302=EDGE_CURVE('',#8774,#8775,#3681,.T.);
#11303=EDGE_CURVE('',#8774,#8775,#3682,.T.);
#11304=EDGE_CURVE('',#8776,#8774,#5440,.T.);
#11305=EDGE_CURVE('',#8776,#8777,#3683,.T.);
#11306=EDGE_CURVE('',#8775,#8777,#5441,.T.);
#11307=EDGE_CURVE('',#8777,#8776,#3684,.T.);
#11308=EDGE_CURVE('',#8778,#8779,#4483,.T.);
#11309=EDGE_CURVE('',#8779,#8778,#4484,.T.);
#11310=EDGE_CURVE('',#8779,#8780,#5442,.T.);
#11311=EDGE_CURVE('',#8781,#8780,#4485,.T.);
#11312=EDGE_CURVE('',#8780,#8781,#4486,.T.);
#11313=EDGE_CURVE('',#8782,#8783,#4487,.T.);
#11314=EDGE_CURVE('',#8783,#8782,#4488,.T.);
#11315=EDGE_CURVE('',#8783,#8784,#5443,.T.);
#11316=EDGE_CURVE('',#8785,#8784,#4489,.T.);
#11317=EDGE_CURVE('',#8784,#8785,#4490,.T.);
#11318=EDGE_CURVE('',#8786,#8787,#4491,.T.);
#11319=EDGE_CURVE('',#8787,#8786,#4492,.T.);
#11320=EDGE_CURVE('',#8787,#8788,#5444,.T.);
#11321=EDGE_CURVE('',#8789,#8788,#4493,.T.);
#11322=EDGE_CURVE('',#8790,#8789,#4494,.T.);
#11323=EDGE_CURVE('',#8788,#8790,#4495,.T.);
#11324=EDGE_CURVE('',#8791,#8792,#4496,.T.);
#11325=EDGE_CURVE('',#8792,#8791,#4497,.T.);
#11326=EDGE_CURVE('',#8792,#8793,#5445,.T.);
#11327=EDGE_CURVE('',#8794,#8793,#4498,.T.);
#11328=EDGE_CURVE('',#8793,#8794,#4499,.T.);
#11329=EDGE_CURVE('',#8795,#8795,#3685,.T.);
#11330=EDGE_CURVE('',#8795,#8787,#5446,.T.);
#11331=EDGE_CURVE('',#8786,#8796,#5447,.T.);
#11332=EDGE_CURVE('',#8796,#8796,#3686,.T.);
#11333=EDGE_CURVE('',#8797,#8797,#3687,.T.);
#11334=EDGE_CURVE('',#8798,#8798,#3688,.T.);
#11335=EDGE_CURVE('',#8799,#8799,#3689,.T.);
#11336=EDGE_CURVE('',#8799,#8798,#5448,.T.);
#11337=EDGE_CURVE('',#8800,#8800,#3690,.T.);
#11338=EDGE_CURVE('',#8800,#8801,#5449,.T.);
#11339=EDGE_CURVE('',#8801,#8801,#3691,.T.);
#11340=EDGE_CURVE('',#8797,#8800,#5450,.T.);
#11341=EDGE_CURVE('',#8802,#8802,#3692,.T.);
#11342=EDGE_CURVE('',#8802,#8799,#5451,.T.);
#11343=EDGE_CURVE('',#8803,#8803,#3693,.T.);
#11344=EDGE_CURVE('',#8803,#8804,#5452,.T.);
#11345=EDGE_CURVE('',#8804,#8804,#3694,.T.);
#11346=EDGE_CURVE('',#8804,#8790,#5453,.T.);
#11347=EDGE_CURVE('',#8788,#8805,#5454,.T.);
#11348=EDGE_CURVE('',#8805,#8805,#3695,.T.);
#11349=EDGE_CURVE('',#8805,#8806,#5455,.T.);
#11350=EDGE_CURVE('',#8806,#8806,#3696,.T.);
#11351=EDGE_CURVE('',#8807,#8807,#3697,.T.);
#11352=EDGE_CURVE('',#8807,#8808,#5456,.T.);
#11353=EDGE_CURVE('',#8808,#8808,#3698,.T.);
#11354=EDGE_CURVE('',#8808,#8809,#5457,.T.);
#11355=EDGE_CURVE('',#8809,#8809,#3699,.T.);
#11356=EDGE_CURVE('',#8810,#8811,#5458,.T.);
#11357=EDGE_CURVE('',#8812,#8810,#5459,.T.);
#11358=EDGE_CURVE('',#8813,#8812,#5460,.T.);
#11359=EDGE_CURVE('',#8814,#8813,#5461,.T.);
#11360=EDGE_CURVE('',#8815,#8814,#5462,.T.);
#11361=EDGE_CURVE('',#8816,#8815,#5463,.T.);
#11362=EDGE_CURVE('',#8817,#8816,#5464,.T.);
#11363=EDGE_CURVE('',#8818,#8817,#5465,.T.);
#11364=EDGE_CURVE('',#8819,#8818,#5466,.T.);
#11365=EDGE_CURVE('',#8820,#8819,#5467,.T.);
#11366=EDGE_CURVE('',#8821,#8820,#5468,.T.);
#11367=EDGE_CURVE('',#8822,#8821,#5469,.T.);
#11368=EDGE_CURVE('',#8823,#8822,#5470,.T.);
#11369=EDGE_CURVE('',#8824,#8823,#5471,.T.);
#11370=EDGE_CURVE('',#8825,#8824,#5472,.T.);
#11371=EDGE_CURVE('',#8826,#8825,#5473,.T.);
#11372=EDGE_CURVE('',#8827,#8826,#5474,.T.);
#11373=EDGE_CURVE('',#8828,#8827,#5475,.T.);
#11374=EDGE_CURVE('',#8829,#8828,#5476,.T.);
#11375=EDGE_CURVE('',#8830,#8829,#5477,.T.);
#11376=EDGE_CURVE('',#8831,#8830,#5478,.T.);
#11377=EDGE_CURVE('',#8832,#8831,#5479,.T.);
#11378=EDGE_CURVE('',#8833,#8832,#5480,.T.);
#11379=EDGE_CURVE('',#8834,#8833,#5481,.T.);
#11380=EDGE_CURVE('',#8835,#8834,#5482,.T.);
#11381=EDGE_CURVE('',#8836,#8835,#5483,.T.);
#11382=EDGE_CURVE('',#8837,#8836,#5484,.T.);
#11383=EDGE_CURVE('',#8838,#8837,#5485,.T.);
#11384=EDGE_CURVE('',#8839,#8838,#5486,.T.);
#11385=EDGE_CURVE('',#8840,#8839,#5487,.T.);
#11386=EDGE_CURVE('',#8841,#8840,#5488,.T.);
#11387=EDGE_CURVE('',#8842,#8841,#5489,.T.);
#11388=EDGE_CURVE('',#8843,#8842,#5490,.T.);
#11389=EDGE_CURVE('',#8844,#8843,#5491,.T.);
#11390=EDGE_CURVE('',#8845,#8844,#5492,.T.);
#11391=EDGE_CURVE('',#8846,#8845,#5493,.T.);
#11392=EDGE_CURVE('',#8847,#8846,#5494,.T.);
#11393=EDGE_CURVE('',#8848,#8847,#5495,.T.);
#11394=EDGE_CURVE('',#8849,#8848,#5496,.T.);
#11395=EDGE_CURVE('',#8850,#8849,#5497,.T.);
#11396=EDGE_CURVE('',#8851,#8850,#5498,.T.);
#11397=EDGE_CURVE('',#8852,#8851,#5499,.T.);
#11398=EDGE_CURVE('',#8853,#8852,#5500,.T.);
#11399=EDGE_CURVE('',#8854,#8853,#5501,.T.);
#11400=EDGE_CURVE('',#8855,#8854,#5502,.T.);
#11401=EDGE_CURVE('',#8856,#8855,#5503,.T.);
#11402=EDGE_CURVE('',#8857,#8856,#5504,.T.);
#11403=EDGE_CURVE('',#8858,#8857,#5505,.T.);
#11404=EDGE_CURVE('',#8859,#8858,#5506,.T.);
#11405=EDGE_CURVE('',#8860,#8859,#5507,.T.);
#11406=EDGE_CURVE('',#8861,#8860,#5508,.T.);
#11407=EDGE_CURVE('',#8862,#8861,#5509,.T.);
#11408=EDGE_CURVE('',#8863,#8862,#5510,.T.);
#11409=EDGE_CURVE('',#8864,#8863,#5511,.T.);
#11410=EDGE_CURVE('',#8865,#8864,#5512,.T.);
#11411=EDGE_CURVE('',#8866,#8865,#5513,.T.);
#11412=EDGE_CURVE('',#8867,#8866,#5514,.T.);
#11413=EDGE_CURVE('',#8868,#8867,#5515,.T.);
#11414=EDGE_CURVE('',#8869,#8868,#5516,.T.);
#11415=EDGE_CURVE('',#8870,#8869,#5517,.T.);
#11416=EDGE_CURVE('',#8871,#8870,#5518,.T.);
#11417=EDGE_CURVE('',#8872,#8871,#5519,.T.);
#11418=EDGE_CURVE('',#8873,#8872,#5520,.T.);
#11419=EDGE_CURVE('',#8874,#8873,#5521,.T.);
#11420=EDGE_CURVE('',#8875,#8874,#5522,.T.);
#11421=EDGE_CURVE('',#8876,#8875,#5523,.T.);
#11422=EDGE_CURVE('',#8877,#8876,#5524,.T.);
#11423=EDGE_CURVE('',#8878,#8877,#5525,.T.);
#11424=EDGE_CURVE('',#8879,#8878,#5526,.T.);
#11425=EDGE_CURVE('',#8880,#8879,#5527,.T.);
#11426=EDGE_CURVE('',#8881,#8880,#5528,.T.);
#11427=EDGE_CURVE('',#8882,#8881,#5529,.T.);
#11428=EDGE_CURVE('',#8883,#8882,#5530,.T.);
#11429=EDGE_CURVE('',#8884,#8883,#5531,.T.);
#11430=EDGE_CURVE('',#8885,#8884,#5532,.T.);
#11431=EDGE_CURVE('',#8886,#8885,#5533,.T.);
#11432=EDGE_CURVE('',#8887,#8886,#5534,.T.);
#11433=EDGE_CURVE('',#8888,#8887,#5535,.T.);
#11434=EDGE_CURVE('',#8889,#8888,#5536,.T.);
#11435=EDGE_CURVE('',#8890,#8889,#5537,.T.);
#11436=EDGE_CURVE('',#8891,#8890,#5538,.T.);
#11437=EDGE_CURVE('',#8892,#8891,#5539,.T.);
#11438=EDGE_CURVE('',#8893,#8892,#5540,.T.);
#11439=EDGE_CURVE('',#8894,#8893,#5541,.T.);
#11440=EDGE_CURVE('',#8895,#8894,#5542,.T.);
#11441=EDGE_CURVE('',#8896,#8895,#5543,.T.);
#11442=EDGE_CURVE('',#8897,#8896,#5544,.T.);
#11443=EDGE_CURVE('',#8898,#8897,#5545,.T.);
#11444=EDGE_CURVE('',#8899,#8898,#5546,.T.);
#11445=EDGE_CURVE('',#8900,#8899,#5547,.T.);
#11446=EDGE_CURVE('',#8901,#8900,#5548,.T.);
#11447=EDGE_CURVE('',#8902,#8901,#5549,.T.);
#11448=EDGE_CURVE('',#8903,#8902,#5550,.T.);
#11449=EDGE_CURVE('',#8904,#8903,#5551,.T.);
#11450=EDGE_CURVE('',#8905,#8904,#5552,.T.);
#11451=EDGE_CURVE('',#8906,#8905,#5553,.T.);
#11452=EDGE_CURVE('',#8907,#8906,#5554,.T.);
#11453=EDGE_CURVE('',#8908,#8907,#5555,.T.);
#11454=EDGE_CURVE('',#8909,#8908,#5556,.T.);
#11455=EDGE_CURVE('',#8910,#8909,#5557,.T.);
#11456=EDGE_CURVE('',#8911,#8910,#5558,.T.);
#11457=EDGE_CURVE('',#8912,#8911,#5559,.T.);
#11458=EDGE_CURVE('',#8913,#8912,#5560,.T.);
#11459=EDGE_CURVE('',#8914,#8913,#5561,.T.);
#11460=EDGE_CURVE('',#8915,#8914,#5562,.T.);
#11461=EDGE_CURVE('',#8916,#8915,#5563,.T.);
#11462=EDGE_CURVE('',#8917,#8916,#5564,.T.);
#11463=EDGE_CURVE('',#8918,#8917,#5565,.T.);
#11464=EDGE_CURVE('',#8919,#8918,#5566,.T.);
#11465=EDGE_CURVE('',#8920,#8919,#5567,.T.);
#11466=EDGE_CURVE('',#8921,#8920,#5568,.T.);
#11467=EDGE_CURVE('',#8922,#8921,#5569,.T.);
#11468=EDGE_CURVE('',#8923,#8922,#5570,.T.);
#11469=EDGE_CURVE('',#8924,#8923,#5571,.T.);
#11470=EDGE_CURVE('',#8925,#8924,#5572,.T.);
#11471=EDGE_CURVE('',#8926,#8925,#5573,.T.);
#11472=EDGE_CURVE('',#8927,#8926,#5574,.T.);
#11473=EDGE_CURVE('',#8928,#8927,#5575,.T.);
#11474=EDGE_CURVE('',#8929,#8928,#5576,.T.);
#11475=EDGE_CURVE('',#8930,#8929,#5577,.T.);
#11476=EDGE_CURVE('',#8931,#8930,#5578,.T.);
#11477=EDGE_CURVE('',#8932,#8931,#5579,.T.);
#11478=EDGE_CURVE('',#8933,#8932,#5580,.T.);
#11479=EDGE_CURVE('',#8934,#8933,#5581,.T.);
#11480=EDGE_CURVE('',#8935,#8934,#5582,.T.);
#11481=EDGE_CURVE('',#8936,#8935,#5583,.T.);
#11482=EDGE_CURVE('',#8937,#8936,#5584,.T.);
#11483=EDGE_CURVE('',#8938,#8937,#5585,.T.);
#11484=EDGE_CURVE('',#8939,#8938,#5586,.T.);
#11485=EDGE_CURVE('',#8940,#8939,#5587,.T.);
#11486=EDGE_CURVE('',#8941,#8940,#5588,.T.);
#11487=EDGE_CURVE('',#8942,#8941,#5589,.T.);
#11488=EDGE_CURVE('',#8943,#8942,#5590,.T.);
#11489=EDGE_CURVE('',#8944,#8943,#5591,.T.);
#11490=EDGE_CURVE('',#8945,#8944,#5592,.T.);
#11491=EDGE_CURVE('',#8946,#8945,#5593,.T.);
#11492=EDGE_CURVE('',#8947,#8946,#5594,.T.);
#11493=EDGE_CURVE('',#8948,#8947,#5595,.T.);
#11494=EDGE_CURVE('',#8949,#8948,#5596,.T.);
#11495=EDGE_CURVE('',#8950,#8949,#5597,.T.);
#11496=EDGE_CURVE('',#8951,#8950,#5598,.T.);
#11497=EDGE_CURVE('',#8952,#8951,#5599,.T.);
#11498=EDGE_CURVE('',#8953,#8952,#5600,.T.);
#11499=EDGE_CURVE('',#8954,#8953,#5601,.T.);
#11500=EDGE_CURVE('',#8955,#8954,#5602,.T.);
#11501=EDGE_CURVE('',#8956,#8955,#5603,.T.);
#11502=EDGE_CURVE('',#8957,#8956,#5604,.T.);
#11503=EDGE_CURVE('',#8958,#8957,#5605,.T.);
#11504=EDGE_CURVE('',#8959,#8958,#5606,.T.);
#11505=EDGE_CURVE('',#8811,#8959,#5607,.T.);
#11506=EDGE_CURVE('',#8960,#8960,#3700,.T.);
#11507=EDGE_CURVE('',#8961,#8961,#3701,.T.);
#11508=EDGE_CURVE('',#8961,#8809,#5608,.T.);
#11509=EDGE_CURVE('',#8962,#8963,#5609,.T.);
#11510=EDGE_CURVE('',#8963,#8964,#5610,.T.);
#11511=EDGE_CURVE('',#8964,#8965,#5611,.T.);
#11512=EDGE_CURVE('',#8965,#8966,#5612,.T.);
#11513=EDGE_CURVE('',#8966,#8967,#5613,.T.);
#11514=EDGE_CURVE('',#8967,#8968,#5614,.T.);
#11515=EDGE_CURVE('',#8968,#8969,#5615,.T.);
#11516=EDGE_CURVE('',#8969,#8970,#5616,.T.);
#11517=EDGE_CURVE('',#8970,#8971,#5617,.T.);
#11518=EDGE_CURVE('',#8971,#8972,#5618,.T.);
#11519=EDGE_CURVE('',#8972,#8973,#5619,.T.);
#11520=EDGE_CURVE('',#8973,#8974,#5620,.T.);
#11521=EDGE_CURVE('',#8974,#8975,#5621,.T.);
#11522=EDGE_CURVE('',#8975,#8976,#5622,.T.);
#11523=EDGE_CURVE('',#8976,#8977,#5623,.T.);
#11524=EDGE_CURVE('',#8977,#8978,#5624,.T.);
#11525=EDGE_CURVE('',#8978,#8979,#5625,.T.);
#11526=EDGE_CURVE('',#8979,#8980,#5626,.T.);
#11527=EDGE_CURVE('',#8980,#8981,#5627,.T.);
#11528=EDGE_CURVE('',#8981,#8982,#5628,.T.);
#11529=EDGE_CURVE('',#8982,#8983,#5629,.T.);
#11530=EDGE_CURVE('',#8983,#8984,#5630,.T.);
#11531=EDGE_CURVE('',#8984,#8985,#5631,.T.);
#11532=EDGE_CURVE('',#8985,#8986,#5632,.T.);
#11533=EDGE_CURVE('',#8986,#8987,#5633,.T.);
#11534=EDGE_CURVE('',#8987,#8988,#5634,.T.);
#11535=EDGE_CURVE('',#8988,#8989,#5635,.T.);
#11536=EDGE_CURVE('',#8989,#8990,#5636,.T.);
#11537=EDGE_CURVE('',#8990,#8991,#5637,.T.);
#11538=EDGE_CURVE('',#8991,#8992,#5638,.T.);
#11539=EDGE_CURVE('',#8992,#8993,#5639,.T.);
#11540=EDGE_CURVE('',#8993,#8994,#5640,.T.);
#11541=EDGE_CURVE('',#8994,#8995,#5641,.T.);
#11542=EDGE_CURVE('',#8995,#8996,#5642,.T.);
#11543=EDGE_CURVE('',#8996,#8997,#5643,.T.);
#11544=EDGE_CURVE('',#8997,#8998,#5644,.T.);
#11545=EDGE_CURVE('',#8998,#8999,#5645,.T.);
#11546=EDGE_CURVE('',#8999,#9000,#5646,.T.);
#11547=EDGE_CURVE('',#9000,#9001,#5647,.T.);
#11548=EDGE_CURVE('',#9001,#9002,#5648,.T.);
#11549=EDGE_CURVE('',#9002,#9003,#5649,.T.);
#11550=EDGE_CURVE('',#9003,#9004,#5650,.T.);
#11551=EDGE_CURVE('',#9004,#9005,#5651,.T.);
#11552=EDGE_CURVE('',#9005,#9006,#5652,.T.);
#11553=EDGE_CURVE('',#9006,#9007,#5653,.T.);
#11554=EDGE_CURVE('',#9007,#9008,#5654,.T.);
#11555=EDGE_CURVE('',#9008,#9009,#5655,.T.);
#11556=EDGE_CURVE('',#9009,#9010,#5656,.T.);
#11557=EDGE_CURVE('',#9010,#9011,#5657,.T.);
#11558=EDGE_CURVE('',#9011,#9012,#5658,.T.);
#11559=EDGE_CURVE('',#9012,#9013,#5659,.T.);
#11560=EDGE_CURVE('',#9013,#9014,#5660,.T.);
#11561=EDGE_CURVE('',#9014,#9015,#5661,.T.);
#11562=EDGE_CURVE('',#9015,#9016,#5662,.T.);
#11563=EDGE_CURVE('',#9016,#9017,#5663,.T.);
#11564=EDGE_CURVE('',#9017,#9018,#5664,.T.);
#11565=EDGE_CURVE('',#9018,#9019,#5665,.T.);
#11566=EDGE_CURVE('',#9019,#9020,#5666,.T.);
#11567=EDGE_CURVE('',#9020,#9021,#5667,.T.);
#11568=EDGE_CURVE('',#9021,#9022,#5668,.T.);
#11569=EDGE_CURVE('',#9022,#9023,#5669,.T.);
#11570=EDGE_CURVE('',#9023,#9024,#5670,.T.);
#11571=EDGE_CURVE('',#9024,#9025,#5671,.T.);
#11572=EDGE_CURVE('',#9025,#9026,#5672,.T.);
#11573=EDGE_CURVE('',#9026,#9027,#5673,.T.);
#11574=EDGE_CURVE('',#9027,#9028,#5674,.T.);
#11575=EDGE_CURVE('',#9028,#9029,#5675,.T.);
#11576=EDGE_CURVE('',#9029,#9030,#5676,.T.);
#11577=EDGE_CURVE('',#9030,#9031,#5677,.T.);
#11578=EDGE_CURVE('',#9031,#9032,#5678,.T.);
#11579=EDGE_CURVE('',#9032,#9033,#5679,.T.);
#11580=EDGE_CURVE('',#9033,#9034,#5680,.T.);
#11581=EDGE_CURVE('',#9034,#9035,#5681,.T.);
#11582=EDGE_CURVE('',#9035,#9036,#5682,.T.);
#11583=EDGE_CURVE('',#9036,#9037,#5683,.T.);
#11584=EDGE_CURVE('',#9037,#9038,#5684,.T.);
#11585=EDGE_CURVE('',#9038,#9039,#5685,.T.);
#11586=EDGE_CURVE('',#9039,#9040,#5686,.T.);
#11587=EDGE_CURVE('',#9040,#9041,#5687,.T.);
#11588=EDGE_CURVE('',#9041,#9042,#5688,.T.);
#11589=EDGE_CURVE('',#9042,#9043,#5689,.T.);
#11590=EDGE_CURVE('',#9043,#9044,#5690,.T.);
#11591=EDGE_CURVE('',#9044,#9045,#5691,.T.);
#11592=EDGE_CURVE('',#9045,#9046,#5692,.T.);
#11593=EDGE_CURVE('',#9046,#9047,#5693,.T.);
#11594=EDGE_CURVE('',#9047,#9048,#5694,.T.);
#11595=EDGE_CURVE('',#9048,#9049,#5695,.T.);
#11596=EDGE_CURVE('',#9049,#9050,#5696,.T.);
#11597=EDGE_CURVE('',#9050,#9051,#5697,.T.);
#11598=EDGE_CURVE('',#9051,#9052,#5698,.T.);
#11599=EDGE_CURVE('',#9052,#9053,#5699,.T.);
#11600=EDGE_CURVE('',#9053,#9054,#5700,.T.);
#11601=EDGE_CURVE('',#9054,#9055,#5701,.T.);
#11602=EDGE_CURVE('',#9055,#9056,#5702,.T.);
#11603=EDGE_CURVE('',#9056,#9057,#5703,.T.);
#11604=EDGE_CURVE('',#9057,#9058,#5704,.T.);
#11605=EDGE_CURVE('',#9058,#9059,#5705,.T.);
#11606=EDGE_CURVE('',#9059,#9060,#5706,.T.);
#11607=EDGE_CURVE('',#9060,#9061,#5707,.T.);
#11608=EDGE_CURVE('',#9061,#9062,#5708,.T.);
#11609=EDGE_CURVE('',#9062,#9063,#5709,.T.);
#11610=EDGE_CURVE('',#9063,#9064,#5710,.T.);
#11611=EDGE_CURVE('',#9064,#9065,#5711,.T.);
#11612=EDGE_CURVE('',#9065,#9066,#5712,.T.);
#11613=EDGE_CURVE('',#9066,#9067,#5713,.T.);
#11614=EDGE_CURVE('',#9067,#9068,#5714,.T.);
#11615=EDGE_CURVE('',#9068,#9069,#5715,.T.);
#11616=EDGE_CURVE('',#9069,#9070,#5716,.T.);
#11617=EDGE_CURVE('',#9070,#9071,#5717,.T.);
#11618=EDGE_CURVE('',#9071,#9072,#5718,.T.);
#11619=EDGE_CURVE('',#9072,#9073,#5719,.T.);
#11620=EDGE_CURVE('',#9073,#9074,#5720,.T.);
#11621=EDGE_CURVE('',#9074,#9075,#5721,.T.);
#11622=EDGE_CURVE('',#9075,#9076,#5722,.T.);
#11623=EDGE_CURVE('',#9076,#9077,#5723,.T.);
#11624=EDGE_CURVE('',#9077,#9078,#5724,.T.);
#11625=EDGE_CURVE('',#9078,#9079,#5725,.T.);
#11626=EDGE_CURVE('',#9079,#9080,#5726,.T.);
#11627=EDGE_CURVE('',#9080,#9081,#5727,.T.);
#11628=EDGE_CURVE('',#9081,#9082,#5728,.T.);
#11629=EDGE_CURVE('',#9082,#9083,#5729,.T.);
#11630=EDGE_CURVE('',#9083,#9084,#5730,.T.);
#11631=EDGE_CURVE('',#9084,#9085,#5731,.T.);
#11632=EDGE_CURVE('',#9085,#9086,#5732,.T.);
#11633=EDGE_CURVE('',#9086,#9087,#5733,.T.);
#11634=EDGE_CURVE('',#9087,#9088,#5734,.T.);
#11635=EDGE_CURVE('',#9088,#9089,#5735,.T.);
#11636=EDGE_CURVE('',#9089,#9090,#5736,.T.);
#11637=EDGE_CURVE('',#9090,#9091,#5737,.T.);
#11638=EDGE_CURVE('',#9091,#9092,#5738,.T.);
#11639=EDGE_CURVE('',#9092,#9093,#5739,.T.);
#11640=EDGE_CURVE('',#9093,#9094,#5740,.T.);
#11641=EDGE_CURVE('',#9094,#9095,#5741,.T.);
#11642=EDGE_CURVE('',#9095,#9096,#5742,.T.);
#11643=EDGE_CURVE('',#9096,#9097,#5743,.T.);
#11644=EDGE_CURVE('',#9097,#9098,#5744,.T.);
#11645=EDGE_CURVE('',#9098,#9099,#5745,.T.);
#11646=EDGE_CURVE('',#9099,#9100,#5746,.T.);
#11647=EDGE_CURVE('',#9100,#9101,#5747,.T.);
#11648=EDGE_CURVE('',#9101,#9102,#5748,.T.);
#11649=EDGE_CURVE('',#9102,#9103,#5749,.T.);
#11650=EDGE_CURVE('',#9103,#9104,#5750,.T.);
#11651=EDGE_CURVE('',#9104,#9105,#5751,.T.);
#11652=EDGE_CURVE('',#9105,#9106,#5752,.T.);
#11653=EDGE_CURVE('',#9106,#9107,#5753,.T.);
#11654=EDGE_CURVE('',#9107,#9108,#5754,.T.);
#11655=EDGE_CURVE('',#9108,#9109,#5755,.T.);
#11656=EDGE_CURVE('',#9109,#9110,#5756,.T.);
#11657=EDGE_CURVE('',#9110,#9111,#5757,.T.);
#11658=EDGE_CURVE('',#9111,#8962,#5758,.T.);
#11659=EDGE_CURVE('',#9112,#9112,#3702,.T.);
#11660=EDGE_CURVE('',#8960,#9113,#5759,.T.);
#11661=EDGE_CURVE('',#9113,#9113,#3703,.T.);
#11662=EDGE_CURVE('',#9113,#9114,#5760,.T.);
#11663=EDGE_CURVE('',#9114,#9114,#3704,.T.);
#11664=EDGE_CURVE('',#9112,#9114,#5761,.T.);
#11665=EDGE_CURVE('',#8810,#8962,#5762,.T.);
#11666=EDGE_CURVE('',#8812,#9111,#5763,.T.);
#11667=EDGE_CURVE('',#8813,#9110,#5764,.T.);
#11668=EDGE_CURVE('',#8814,#9109,#5765,.T.);
#11669=EDGE_CURVE('',#8815,#9108,#5766,.T.);
#11670=EDGE_CURVE('',#8816,#9107,#5767,.T.);
#11671=EDGE_CURVE('',#8817,#9106,#5768,.T.);
#11672=EDGE_CURVE('',#8818,#9105,#5769,.T.);
#11673=EDGE_CURVE('',#8819,#9104,#5770,.T.);
#11674=EDGE_CURVE('',#8820,#9103,#5771,.T.);
#11675=EDGE_CURVE('',#8821,#9102,#5772,.T.);
#11676=EDGE_CURVE('',#8822,#9101,#5773,.T.);
#11677=EDGE_CURVE('',#8823,#9100,#5774,.T.);
#11678=EDGE_CURVE('',#8824,#9099,#5775,.T.);
#11679=EDGE_CURVE('',#8825,#9098,#5776,.T.);
#11680=EDGE_CURVE('',#8826,#9097,#5777,.T.);
#11681=EDGE_CURVE('',#8827,#9096,#5778,.T.);
#11682=EDGE_CURVE('',#8828,#9095,#5779,.T.);
#11683=EDGE_CURVE('',#8829,#9094,#5780,.T.);
#11684=EDGE_CURVE('',#8830,#9093,#5781,.T.);
#11685=EDGE_CURVE('',#8831,#9092,#5782,.T.);
#11686=EDGE_CURVE('',#8832,#9091,#5783,.T.);
#11687=EDGE_CURVE('',#8833,#9090,#5784,.T.);
#11688=EDGE_CURVE('',#8834,#9089,#5785,.T.);
#11689=EDGE_CURVE('',#8835,#9088,#5786,.T.);
#11690=EDGE_CURVE('',#8836,#9087,#5787,.T.);
#11691=EDGE_CURVE('',#8837,#9086,#5788,.T.);
#11692=EDGE_CURVE('',#8838,#9085,#5789,.T.);
#11693=EDGE_CURVE('',#8839,#9084,#5790,.T.);
#11694=EDGE_CURVE('',#8840,#9083,#5791,.T.);
#11695=EDGE_CURVE('',#8841,#9082,#5792,.T.);
#11696=EDGE_CURVE('',#8842,#9081,#5793,.T.);
#11697=EDGE_CURVE('',#8843,#9080,#5794,.T.);
#11698=EDGE_CURVE('',#8844,#9079,#5795,.T.);
#11699=EDGE_CURVE('',#8845,#9078,#5796,.T.);
#11700=EDGE_CURVE('',#8846,#9077,#5797,.T.);
#11701=EDGE_CURVE('',#8847,#9076,#5798,.T.);
#11702=EDGE_CURVE('',#8848,#9075,#5799,.T.);
#11703=EDGE_CURVE('',#8849,#9074,#5800,.T.);
#11704=EDGE_CURVE('',#8850,#9073,#5801,.T.);
#11705=EDGE_CURVE('',#8851,#9072,#5802,.T.);
#11706=EDGE_CURVE('',#8852,#9071,#5803,.T.);
#11707=EDGE_CURVE('',#8853,#9070,#5804,.T.);
#11708=EDGE_CURVE('',#8854,#9069,#5805,.T.);
#11709=EDGE_CURVE('',#8855,#9068,#5806,.T.);
#11710=EDGE_CURVE('',#8856,#9067,#5807,.T.);
#11711=EDGE_CURVE('',#8857,#9066,#5808,.T.);
#11712=EDGE_CURVE('',#8858,#9065,#5809,.T.);
#11713=EDGE_CURVE('',#8859,#9064,#5810,.T.);
#11714=EDGE_CURVE('',#8860,#9063,#5811,.T.);
#11715=EDGE_CURVE('',#8861,#9062,#5812,.T.);
#11716=EDGE_CURVE('',#8862,#9061,#5813,.T.);
#11717=EDGE_CURVE('',#8863,#9060,#5814,.T.);
#11718=EDGE_CURVE('',#8864,#9059,#5815,.T.);
#11719=EDGE_CURVE('',#8865,#9058,#5816,.T.);
#11720=EDGE_CURVE('',#8866,#9057,#5817,.T.);
#11721=EDGE_CURVE('',#8867,#9056,#5818,.T.);
#11722=EDGE_CURVE('',#8868,#9055,#5819,.T.);
#11723=EDGE_CURVE('',#8869,#9054,#5820,.T.);
#11724=EDGE_CURVE('',#8870,#9053,#5821,.T.);
#11725=EDGE_CURVE('',#8871,#9052,#5822,.T.);
#11726=EDGE_CURVE('',#8872,#9051,#5823,.T.);
#11727=EDGE_CURVE('',#8873,#9050,#5824,.T.);
#11728=EDGE_CURVE('',#8874,#9049,#5825,.T.);
#11729=EDGE_CURVE('',#8875,#9048,#5826,.T.);
#11730=EDGE_CURVE('',#8876,#9047,#5827,.T.);
#11731=EDGE_CURVE('',#8877,#9046,#5828,.T.);
#11732=EDGE_CURVE('',#8878,#9045,#5829,.T.);
#11733=EDGE_CURVE('',#8879,#9044,#5830,.T.);
#11734=EDGE_CURVE('',#8880,#9043,#5831,.T.);
#11735=EDGE_CURVE('',#8881,#9042,#5832,.T.);
#11736=EDGE_CURVE('',#8882,#9041,#5833,.T.);
#11737=EDGE_CURVE('',#8883,#9040,#5834,.T.);
#11738=EDGE_CURVE('',#8884,#9039,#5835,.T.);
#11739=EDGE_CURVE('',#8885,#9038,#5836,.T.);
#11740=EDGE_CURVE('',#8886,#9037,#5837,.T.);
#11741=EDGE_CURVE('',#8887,#9036,#5838,.T.);
#11742=EDGE_CURVE('',#8888,#9035,#5839,.T.);
#11743=EDGE_CURVE('',#8889,#9034,#5840,.T.);
#11744=EDGE_CURVE('',#8890,#9033,#5841,.T.);
#11745=EDGE_CURVE('',#8891,#9032,#5842,.T.);
#11746=EDGE_CURVE('',#8892,#9031,#5843,.T.);
#11747=EDGE_CURVE('',#8893,#9030,#5844,.T.);
#11748=EDGE_CURVE('',#8894,#9029,#5845,.T.);
#11749=EDGE_CURVE('',#8895,#9028,#5846,.T.);
#11750=EDGE_CURVE('',#8896,#9027,#5847,.T.);
#11751=EDGE_CURVE('',#8897,#9026,#5848,.T.);
#11752=EDGE_CURVE('',#8898,#9025,#5849,.T.);
#11753=EDGE_CURVE('',#8899,#9024,#5850,.T.);
#11754=EDGE_CURVE('',#8900,#9023,#5851,.T.);
#11755=EDGE_CURVE('',#8901,#9022,#5852,.T.);
#11756=EDGE_CURVE('',#8902,#9021,#5853,.T.);
#11757=EDGE_CURVE('',#8903,#9020,#5854,.T.);
#11758=EDGE_CURVE('',#8904,#9019,#5855,.T.);
#11759=EDGE_CURVE('',#8905,#9018,#5856,.T.);
#11760=EDGE_CURVE('',#8906,#9017,#5857,.T.);
#11761=EDGE_CURVE('',#8907,#9016,#5858,.T.);
#11762=EDGE_CURVE('',#8908,#9015,#5859,.T.);
#11763=EDGE_CURVE('',#8909,#9014,#5860,.T.);
#11764=EDGE_CURVE('',#8910,#9013,#5861,.T.);
#11765=EDGE_CURVE('',#8911,#9012,#5862,.T.);
#11766=EDGE_CURVE('',#8912,#9011,#5863,.T.);
#11767=EDGE_CURVE('',#8913,#9010,#5864,.T.);
#11768=EDGE_CURVE('',#8914,#9009,#5865,.T.);
#11769=EDGE_CURVE('',#8915,#9008,#5866,.T.);
#11770=EDGE_CURVE('',#8916,#9007,#5867,.T.);
#11771=EDGE_CURVE('',#8917,#9006,#5868,.T.);
#11772=EDGE_CURVE('',#8918,#9005,#5869,.T.);
#11773=EDGE_CURVE('',#8919,#9004,#5870,.T.);
#11774=EDGE_CURVE('',#8920,#9003,#5871,.T.);
#11775=EDGE_CURVE('',#8921,#9002,#5872,.T.);
#11776=EDGE_CURVE('',#8922,#9001,#5873,.T.);
#11777=EDGE_CURVE('',#8923,#9000,#5874,.T.);
#11778=EDGE_CURVE('',#8924,#8999,#5875,.T.);
#11779=EDGE_CURVE('',#8925,#8998,#5876,.T.);
#11780=EDGE_CURVE('',#8926,#8997,#5877,.T.);
#11781=EDGE_CURVE('',#8927,#8996,#5878,.T.);
#11782=EDGE_CURVE('',#8928,#8995,#5879,.T.);
#11783=EDGE_CURVE('',#8929,#8994,#5880,.T.);
#11784=EDGE_CURVE('',#8930,#8993,#5881,.T.);
#11785=EDGE_CURVE('',#8931,#8992,#5882,.T.);
#11786=EDGE_CURVE('',#8932,#8991,#5883,.T.);
#11787=EDGE_CURVE('',#8933,#8990,#5884,.T.);
#11788=EDGE_CURVE('',#8934,#8989,#5885,.T.);
#11789=EDGE_CURVE('',#8935,#8988,#5886,.T.);
#11790=EDGE_CURVE('',#8936,#8987,#5887,.T.);
#11791=EDGE_CURVE('',#8937,#8986,#5888,.T.);
#11792=EDGE_CURVE('',#8938,#8985,#5889,.T.);
#11793=EDGE_CURVE('',#8939,#8984,#5890,.T.);
#11794=EDGE_CURVE('',#8940,#8983,#5891,.T.);
#11795=EDGE_CURVE('',#8941,#8982,#5892,.T.);
#11796=EDGE_CURVE('',#8942,#8981,#5893,.T.);
#11797=EDGE_CURVE('',#8943,#8980,#5894,.T.);
#11798=EDGE_CURVE('',#8944,#8979,#5895,.T.);
#11799=EDGE_CURVE('',#8945,#8978,#5896,.T.);
#11800=EDGE_CURVE('',#8946,#8977,#5897,.T.);
#11801=EDGE_CURVE('',#8947,#8976,#5898,.T.);
#11802=EDGE_CURVE('',#8948,#8975,#5899,.T.);
#11803=EDGE_CURVE('',#8949,#8974,#5900,.T.);
#11804=EDGE_CURVE('',#8950,#8973,#5901,.T.);
#11805=EDGE_CURVE('',#8951,#8972,#5902,.T.);
#11806=EDGE_CURVE('',#8952,#8971,#5903,.T.);
#11807=EDGE_CURVE('',#8953,#8970,#5904,.T.);
#11808=EDGE_CURVE('',#8954,#8969,#5905,.T.);
#11809=EDGE_CURVE('',#8955,#8968,#5906,.T.);
#11810=EDGE_CURVE('',#8956,#8967,#5907,.T.);
#11811=EDGE_CURVE('',#8957,#8966,#5908,.T.);
#11812=EDGE_CURVE('',#8958,#8965,#5909,.T.);
#11813=EDGE_CURVE('',#8959,#8964,#5910,.T.);
#11814=EDGE_CURVE('',#8811,#8963,#5911,.T.);
#11815=ORIENTED_EDGE('',*,*,#9115,.F.);
#11816=ORIENTED_EDGE('',*,*,#9116,.T.);
#11817=ORIENTED_EDGE('',*,*,#9117,.T.);
#11818=ORIENTED_EDGE('',*,*,#9118,.T.);
#11819=ORIENTED_EDGE('',*,*,#9119,.F.);
#11820=ORIENTED_EDGE('',*,*,#9120,.T.);
#11821=ORIENTED_EDGE('',*,*,#9115,.T.);
#11822=ORIENTED_EDGE('',*,*,#9121,.T.);
#11823=ORIENTED_EDGE('',*,*,#9122,.F.);
#11824=ORIENTED_EDGE('',*,*,#9123,.T.);
#11825=ORIENTED_EDGE('',*,*,#9119,.T.);
#11826=ORIENTED_EDGE('',*,*,#9124,.T.);
#11827=ORIENTED_EDGE('',*,*,#9125,.F.);
#11828=ORIENTED_EDGE('',*,*,#9126,.T.);
#11829=ORIENTED_EDGE('',*,*,#9122,.T.);
#11830=ORIENTED_EDGE('',*,*,#9127,.T.);
#11831=ORIENTED_EDGE('',*,*,#9128,.F.);
#11832=ORIENTED_EDGE('',*,*,#9129,.T.);
#11833=ORIENTED_EDGE('',*,*,#9125,.T.);
#11834=ORIENTED_EDGE('',*,*,#9130,.T.);
#11835=ORIENTED_EDGE('',*,*,#9131,.F.);
#11836=ORIENTED_EDGE('',*,*,#9132,.T.);
#11837=ORIENTED_EDGE('',*,*,#9128,.T.);
#11838=ORIENTED_EDGE('',*,*,#9133,.T.);
#11839=ORIENTED_EDGE('',*,*,#9134,.F.);
#11840=ORIENTED_EDGE('',*,*,#9135,.T.);
#11841=ORIENTED_EDGE('',*,*,#9131,.T.);
#11842=ORIENTED_EDGE('',*,*,#9136,.T.);
#11843=ORIENTED_EDGE('',*,*,#9137,.F.);
#11844=ORIENTED_EDGE('',*,*,#9138,.T.);
#11845=ORIENTED_EDGE('',*,*,#9134,.T.);
#11846=ORIENTED_EDGE('',*,*,#9139,.T.);
#11847=ORIENTED_EDGE('',*,*,#9140,.F.);
#11848=ORIENTED_EDGE('',*,*,#9141,.T.);
#11849=ORIENTED_EDGE('',*,*,#9137,.T.);
#11850=ORIENTED_EDGE('',*,*,#9142,.T.);
#11851=ORIENTED_EDGE('',*,*,#9143,.F.);
#11852=ORIENTED_EDGE('',*,*,#9144,.T.);
#11853=ORIENTED_EDGE('',*,*,#9140,.T.);
#11854=ORIENTED_EDGE('',*,*,#9145,.T.);
#11855=ORIENTED_EDGE('',*,*,#9146,.F.);
#11856=ORIENTED_EDGE('',*,*,#9147,.T.);
#11857=ORIENTED_EDGE('',*,*,#9143,.T.);
#11858=ORIENTED_EDGE('',*,*,#9148,.T.);
#11859=ORIENTED_EDGE('',*,*,#9149,.F.);
#11860=ORIENTED_EDGE('',*,*,#9150,.T.);
#11861=ORIENTED_EDGE('',*,*,#9146,.T.);
#11862=ORIENTED_EDGE('',*,*,#9151,.T.);
#11863=ORIENTED_EDGE('',*,*,#9152,.F.);
#11864=ORIENTED_EDGE('',*,*,#9153,.T.);
#11865=ORIENTED_EDGE('',*,*,#9149,.T.);
#11866=ORIENTED_EDGE('',*,*,#9154,.T.);
#11867=ORIENTED_EDGE('',*,*,#9155,.F.);
#11868=ORIENTED_EDGE('',*,*,#9156,.T.);
#11869=ORIENTED_EDGE('',*,*,#9152,.T.);
#11870=ORIENTED_EDGE('',*,*,#9157,.T.);
#11871=ORIENTED_EDGE('',*,*,#9158,.F.);
#11872=ORIENTED_EDGE('',*,*,#9159,.T.);
#11873=ORIENTED_EDGE('',*,*,#9155,.T.);
#11874=ORIENTED_EDGE('',*,*,#9160,.T.);
#11875=ORIENTED_EDGE('',*,*,#9161,.F.);
#11876=ORIENTED_EDGE('',*,*,#9162,.T.);
#11877=ORIENTED_EDGE('',*,*,#9158,.T.);
#11878=ORIENTED_EDGE('',*,*,#9163,.T.);
#11879=ORIENTED_EDGE('',*,*,#9164,.F.);
#11880=ORIENTED_EDGE('',*,*,#9165,.T.);
#11881=ORIENTED_EDGE('',*,*,#9166,.T.);
#11882=ORIENTED_EDGE('',*,*,#9167,.T.);
#11883=ORIENTED_EDGE('',*,*,#9168,.F.);
#11884=ORIENTED_EDGE('',*,*,#9169,.T.);
#11885=ORIENTED_EDGE('',*,*,#9168,.T.);
#11886=ORIENTED_EDGE('',*,*,#9170,.T.);
#11887=ORIENTED_EDGE('',*,*,#9171,.F.);
#11888=ORIENTED_EDGE('',*,*,#9172,.T.);
#11889=ORIENTED_EDGE('',*,*,#9173,.T.);
#11890=ORIENTED_EDGE('',*,*,#9174,.T.);
#11891=ORIENTED_EDGE('',*,*,#9175,.F.);
#11892=ORIENTED_EDGE('',*,*,#9176,.T.);
#11893=ORIENTED_EDGE('',*,*,#9177,.T.);
#11894=ORIENTED_EDGE('',*,*,#9178,.T.);
#11895=ORIENTED_EDGE('',*,*,#9179,.F.);
#11896=ORIENTED_EDGE('',*,*,#9180,.T.);
#11897=ORIENTED_EDGE('',*,*,#9181,.T.);
#11898=ORIENTED_EDGE('',*,*,#9182,.T.);
#11899=ORIENTED_EDGE('',*,*,#9183,.F.);
#11900=ORIENTED_EDGE('',*,*,#9184,.T.);
#11901=ORIENTED_EDGE('',*,*,#9185,.T.);
#11902=ORIENTED_EDGE('',*,*,#9186,.T.);
#11903=ORIENTED_EDGE('',*,*,#9187,.F.);
#11904=ORIENTED_EDGE('',*,*,#9188,.T.);
#11905=ORIENTED_EDGE('',*,*,#9189,.T.);
#11906=ORIENTED_EDGE('',*,*,#9190,.T.);
#11907=ORIENTED_EDGE('',*,*,#9191,.F.);
#11908=ORIENTED_EDGE('',*,*,#9192,.T.);
#11909=ORIENTED_EDGE('',*,*,#9193,.T.);
#11910=ORIENTED_EDGE('',*,*,#9194,.T.);
#11911=ORIENTED_EDGE('',*,*,#9195,.F.);
#11912=ORIENTED_EDGE('',*,*,#9196,.T.);
#11913=ORIENTED_EDGE('',*,*,#9197,.T.);
#11914=ORIENTED_EDGE('',*,*,#9198,.T.);
#11915=ORIENTED_EDGE('',*,*,#9199,.F.);
#11916=ORIENTED_EDGE('',*,*,#9200,.T.);
#11917=ORIENTED_EDGE('',*,*,#9201,.T.);
#11918=ORIENTED_EDGE('',*,*,#9202,.T.);
#11919=ORIENTED_EDGE('',*,*,#9203,.F.);
#11920=ORIENTED_EDGE('',*,*,#9204,.T.);
#11921=ORIENTED_EDGE('',*,*,#9205,.T.);
#11922=ORIENTED_EDGE('',*,*,#9206,.T.);
#11923=ORIENTED_EDGE('',*,*,#9207,.F.);
#11924=ORIENTED_EDGE('',*,*,#9208,.T.);
#11925=ORIENTED_EDGE('',*,*,#9209,.T.);
#11926=ORIENTED_EDGE('',*,*,#9210,.T.);
#11927=ORIENTED_EDGE('',*,*,#9211,.F.);
#11928=ORIENTED_EDGE('',*,*,#9212,.T.);
#11929=ORIENTED_EDGE('',*,*,#9213,.T.);
#11930=ORIENTED_EDGE('',*,*,#9214,.T.);
#11931=ORIENTED_EDGE('',*,*,#9215,.F.);
#11932=ORIENTED_EDGE('',*,*,#9216,.T.);
#11933=ORIENTED_EDGE('',*,*,#9217,.T.);
#11934=ORIENTED_EDGE('',*,*,#9218,.T.);
#11935=ORIENTED_EDGE('',*,*,#9219,.F.);
#11936=ORIENTED_EDGE('',*,*,#9220,.T.);
#11937=ORIENTED_EDGE('',*,*,#9221,.T.);
#11938=ORIENTED_EDGE('',*,*,#9222,.T.);
#11939=ORIENTED_EDGE('',*,*,#9223,.F.);
#11940=ORIENTED_EDGE('',*,*,#9224,.T.);
#11941=ORIENTED_EDGE('',*,*,#9225,.T.);
#11942=ORIENTED_EDGE('',*,*,#9226,.T.);
#11943=ORIENTED_EDGE('',*,*,#9227,.F.);
#11944=ORIENTED_EDGE('',*,*,#9228,.T.);
#11945=ORIENTED_EDGE('',*,*,#9229,.T.);
#11946=ORIENTED_EDGE('',*,*,#9230,.T.);
#11947=ORIENTED_EDGE('',*,*,#9231,.F.);
#11948=ORIENTED_EDGE('',*,*,#9232,.T.);
#11949=ORIENTED_EDGE('',*,*,#9233,.T.);
#11950=ORIENTED_EDGE('',*,*,#9234,.T.);
#11951=ORIENTED_EDGE('',*,*,#9235,.F.);
#11952=ORIENTED_EDGE('',*,*,#9236,.T.);
#11953=ORIENTED_EDGE('',*,*,#9237,.T.);
#11954=ORIENTED_EDGE('',*,*,#9238,.T.);
#11955=ORIENTED_EDGE('',*,*,#9239,.F.);
#11956=ORIENTED_EDGE('',*,*,#9240,.T.);
#11957=ORIENTED_EDGE('',*,*,#9241,.T.);
#11958=ORIENTED_EDGE('',*,*,#9242,.T.);
#11959=ORIENTED_EDGE('',*,*,#9243,.F.);
#11960=ORIENTED_EDGE('',*,*,#9244,.T.);
#11961=ORIENTED_EDGE('',*,*,#9245,.T.);
#11962=ORIENTED_EDGE('',*,*,#9246,.T.);
#11963=ORIENTED_EDGE('',*,*,#9247,.F.);
#11964=ORIENTED_EDGE('',*,*,#9248,.T.);
#11965=ORIENTED_EDGE('',*,*,#9249,.T.);
#11966=ORIENTED_EDGE('',*,*,#9250,.T.);
#11967=ORIENTED_EDGE('',*,*,#9251,.F.);
#11968=ORIENTED_EDGE('',*,*,#9252,.T.);
#11969=ORIENTED_EDGE('',*,*,#9253,.T.);
#11970=ORIENTED_EDGE('',*,*,#9254,.T.);
#11971=ORIENTED_EDGE('',*,*,#9255,.F.);
#11972=ORIENTED_EDGE('',*,*,#9256,.T.);
#11973=ORIENTED_EDGE('',*,*,#9257,.T.);
#11974=ORIENTED_EDGE('',*,*,#9258,.T.);
#11975=ORIENTED_EDGE('',*,*,#9259,.F.);
#11976=ORIENTED_EDGE('',*,*,#9260,.T.);
#11977=ORIENTED_EDGE('',*,*,#9261,.F.);
#11978=ORIENTED_EDGE('',*,*,#9262,.F.);
#11979=ORIENTED_EDGE('',*,*,#9263,.F.);
#11980=ORIENTED_EDGE('',*,*,#9264,.T.);
#11981=ORIENTED_EDGE('',*,*,#9259,.T.);
#11982=ORIENTED_EDGE('',*,*,#9265,.F.);
#11983=ORIENTED_EDGE('',*,*,#9266,.F.);
#11984=ORIENTED_EDGE('',*,*,#9267,.T.);
#11985=ORIENTED_EDGE('',*,*,#9263,.T.);
#11986=ORIENTED_EDGE('',*,*,#9268,.F.);
#11987=ORIENTED_EDGE('',*,*,#9269,.F.);
#11988=ORIENTED_EDGE('',*,*,#9270,.T.);
#11989=ORIENTED_EDGE('',*,*,#9266,.T.);
#11990=ORIENTED_EDGE('',*,*,#9271,.F.);
#11991=ORIENTED_EDGE('',*,*,#9272,.F.);
#11992=ORIENTED_EDGE('',*,*,#9273,.T.);
#11993=ORIENTED_EDGE('',*,*,#9269,.T.);
#11994=ORIENTED_EDGE('',*,*,#9274,.F.);
#11995=ORIENTED_EDGE('',*,*,#9275,.F.);
#11996=ORIENTED_EDGE('',*,*,#9276,.T.);
#11997=ORIENTED_EDGE('',*,*,#9272,.T.);
#11998=ORIENTED_EDGE('',*,*,#9277,.F.);
#11999=ORIENTED_EDGE('',*,*,#9278,.F.);
#12000=ORIENTED_EDGE('',*,*,#9279,.T.);
#12001=ORIENTED_EDGE('',*,*,#9275,.T.);
#12002=ORIENTED_EDGE('',*,*,#9280,.F.);
#12003=ORIENTED_EDGE('',*,*,#9281,.F.);
#12004=ORIENTED_EDGE('',*,*,#9282,.T.);
#12005=ORIENTED_EDGE('',*,*,#9278,.T.);
#12006=ORIENTED_EDGE('',*,*,#9283,.F.);
#12007=ORIENTED_EDGE('',*,*,#9284,.F.);
#12008=ORIENTED_EDGE('',*,*,#9285,.T.);
#12009=ORIENTED_EDGE('',*,*,#9281,.T.);
#12010=ORIENTED_EDGE('',*,*,#9286,.F.);
#12011=ORIENTED_EDGE('',*,*,#9287,.F.);
#12012=ORIENTED_EDGE('',*,*,#9288,.T.);
#12013=ORIENTED_EDGE('',*,*,#9284,.T.);
#12014=ORIENTED_EDGE('',*,*,#9289,.F.);
#12015=ORIENTED_EDGE('',*,*,#9290,.F.);
#12016=ORIENTED_EDGE('',*,*,#9291,.T.);
#12017=ORIENTED_EDGE('',*,*,#9287,.T.);
#12018=ORIENTED_EDGE('',*,*,#9292,.F.);
#12019=ORIENTED_EDGE('',*,*,#9293,.F.);
#12020=ORIENTED_EDGE('',*,*,#9294,.T.);
#12021=ORIENTED_EDGE('',*,*,#9290,.T.);
#12022=ORIENTED_EDGE('',*,*,#9295,.F.);
#12023=ORIENTED_EDGE('',*,*,#9296,.F.);
#12024=ORIENTED_EDGE('',*,*,#9297,.T.);
#12025=ORIENTED_EDGE('',*,*,#9293,.T.);
#12026=ORIENTED_EDGE('',*,*,#9298,.F.);
#12027=ORIENTED_EDGE('',*,*,#9299,.F.);
#12028=ORIENTED_EDGE('',*,*,#9300,.T.);
#12029=ORIENTED_EDGE('',*,*,#9296,.T.);
#12030=ORIENTED_EDGE('',*,*,#9301,.F.);
#12031=ORIENTED_EDGE('',*,*,#9302,.F.);
#12032=ORIENTED_EDGE('',*,*,#9303,.T.);
#12033=ORIENTED_EDGE('',*,*,#9299,.T.);
#12034=ORIENTED_EDGE('',*,*,#9304,.F.);
#12035=ORIENTED_EDGE('',*,*,#9305,.F.);
#12036=ORIENTED_EDGE('',*,*,#9306,.T.);
#12037=ORIENTED_EDGE('',*,*,#9302,.T.);
#12038=ORIENTED_EDGE('',*,*,#9307,.F.);
#12039=ORIENTED_EDGE('',*,*,#9308,.T.);
#12040=ORIENTED_EDGE('',*,*,#9309,.T.);
#12041=ORIENTED_EDGE('',*,*,#9310,.T.);
#12042=ORIENTED_EDGE('',*,*,#9311,.T.);
#12043=ORIENTED_EDGE('',*,*,#9309,.F.);
#12044=ORIENTED_EDGE('',*,*,#9310,.F.);
#12045=ORIENTED_EDGE('',*,*,#9311,.F.);
#12046=ORIENTED_EDGE('',*,*,#9312,.T.);
#12047=ORIENTED_EDGE('',*,*,#9313,.T.);
#12048=ORIENTED_EDGE('',*,*,#9312,.F.);
#12049=ORIENTED_EDGE('',*,*,#9308,.F.);
#12050=ORIENTED_EDGE('',*,*,#9314,.F.);
#12051=ORIENTED_EDGE('',*,*,#9315,.T.);
#12052=ORIENTED_EDGE('',*,*,#9316,.T.);
#12053=ORIENTED_EDGE('',*,*,#9317,.T.);
#12054=ORIENTED_EDGE('',*,*,#9318,.T.);
#12055=ORIENTED_EDGE('',*,*,#9319,.T.);
#12056=ORIENTED_EDGE('',*,*,#9316,.F.);
#12057=ORIENTED_EDGE('',*,*,#9320,.F.);
#12058=ORIENTED_EDGE('',*,*,#9321,.T.);
#12059=ORIENTED_EDGE('',*,*,#9322,.F.);
#12060=ORIENTED_EDGE('',*,*,#9315,.F.);
#12061=ORIENTED_EDGE('',*,*,#9323,.F.);
#12062=ORIENTED_EDGE('',*,*,#9324,.T.);
#12063=ORIENTED_EDGE('',*,*,#9325,.T.);
#12064=ORIENTED_EDGE('',*,*,#9320,.T.);
#12065=ORIENTED_EDGE('',*,*,#9319,.F.);
#12066=ORIENTED_EDGE('',*,*,#9326,.T.);
#12067=ORIENTED_EDGE('',*,*,#9327,.F.);
#12068=ORIENTED_EDGE('',*,*,#9328,.T.);
#12069=ORIENTED_EDGE('',*,*,#9323,.T.);
#12070=ORIENTED_EDGE('',*,*,#9329,.T.);
#12071=ORIENTED_EDGE('',*,*,#9330,.T.);
#12072=ORIENTED_EDGE('',*,*,#9331,.T.);
#12073=ORIENTED_EDGE('',*,*,#9332,.T.);
#12074=ORIENTED_EDGE('',*,*,#9333,.T.);
#12075=ORIENTED_EDGE('',*,*,#9330,.F.);
#12076=ORIENTED_EDGE('',*,*,#9334,.F.);
#12077=ORIENTED_EDGE('',*,*,#9335,.T.);
#12078=ORIENTED_EDGE('',*,*,#9336,.F.);
#12079=ORIENTED_EDGE('',*,*,#9329,.F.);
#12080=ORIENTED_EDGE('',*,*,#9337,.F.);
#12081=ORIENTED_EDGE('',*,*,#9338,.T.);
#12082=ORIENTED_EDGE('',*,*,#9339,.T.);
#12083=ORIENTED_EDGE('',*,*,#9334,.T.);
#12084=ORIENTED_EDGE('',*,*,#9333,.F.);
#12085=ORIENTED_EDGE('',*,*,#9340,.T.);
#12086=ORIENTED_EDGE('',*,*,#9325,.F.);
#12087=ORIENTED_EDGE('',*,*,#9341,.T.);
#12088=ORIENTED_EDGE('',*,*,#9337,.T.);
#12089=ORIENTED_EDGE('',*,*,#9342,.T.);
#12090=ORIENTED_EDGE('',*,*,#9343,.T.);
#12091=ORIENTED_EDGE('',*,*,#9344,.T.);
#12092=ORIENTED_EDGE('',*,*,#9345,.T.);
#12093=ORIENTED_EDGE('',*,*,#9346,.T.);
#12094=ORIENTED_EDGE('',*,*,#9343,.F.);
#12095=ORIENTED_EDGE('',*,*,#9347,.F.);
#12096=ORIENTED_EDGE('',*,*,#9348,.T.);
#12097=ORIENTED_EDGE('',*,*,#9349,.F.);
#12098=ORIENTED_EDGE('',*,*,#9342,.F.);
#12099=ORIENTED_EDGE('',*,*,#9350,.F.);
#12100=ORIENTED_EDGE('',*,*,#9351,.T.);
#12101=ORIENTED_EDGE('',*,*,#9352,.T.);
#12102=ORIENTED_EDGE('',*,*,#9347,.T.);
#12103=ORIENTED_EDGE('',*,*,#9346,.F.);
#12104=ORIENTED_EDGE('',*,*,#9353,.T.);
#12105=ORIENTED_EDGE('',*,*,#9339,.F.);
#12106=ORIENTED_EDGE('',*,*,#9354,.T.);
#12107=ORIENTED_EDGE('',*,*,#9350,.T.);
#12108=ORIENTED_EDGE('',*,*,#9355,.T.);
#12109=ORIENTED_EDGE('',*,*,#9356,.T.);
#12110=ORIENTED_EDGE('',*,*,#9357,.T.);
#12111=ORIENTED_EDGE('',*,*,#9358,.T.);
#12112=ORIENTED_EDGE('',*,*,#9359,.T.);
#12113=ORIENTED_EDGE('',*,*,#9356,.F.);
#12114=ORIENTED_EDGE('',*,*,#9360,.F.);
#12115=ORIENTED_EDGE('',*,*,#9361,.T.);
#12116=ORIENTED_EDGE('',*,*,#9362,.F.);
#12117=ORIENTED_EDGE('',*,*,#9355,.F.);
#12118=ORIENTED_EDGE('',*,*,#9363,.F.);
#12119=ORIENTED_EDGE('',*,*,#9364,.T.);
#12120=ORIENTED_EDGE('',*,*,#9365,.T.);
#12121=ORIENTED_EDGE('',*,*,#9360,.T.);
#12122=ORIENTED_EDGE('',*,*,#9359,.F.);
#12123=ORIENTED_EDGE('',*,*,#9366,.T.);
#12124=ORIENTED_EDGE('',*,*,#9352,.F.);
#12125=ORIENTED_EDGE('',*,*,#9367,.T.);
#12126=ORIENTED_EDGE('',*,*,#9363,.T.);
#12127=ORIENTED_EDGE('',*,*,#9368,.T.);
#12128=ORIENTED_EDGE('',*,*,#9369,.T.);
#12129=ORIENTED_EDGE('',*,*,#9370,.T.);
#12130=ORIENTED_EDGE('',*,*,#9371,.T.);
#12131=ORIENTED_EDGE('',*,*,#9372,.T.);
#12132=ORIENTED_EDGE('',*,*,#9369,.F.);
#12133=ORIENTED_EDGE('',*,*,#9373,.F.);
#12134=ORIENTED_EDGE('',*,*,#9374,.T.);
#12135=ORIENTED_EDGE('',*,*,#9375,.F.);
#12136=ORIENTED_EDGE('',*,*,#9368,.F.);
#12137=ORIENTED_EDGE('',*,*,#9376,.F.);
#12138=ORIENTED_EDGE('',*,*,#9377,.T.);
#12139=ORIENTED_EDGE('',*,*,#9378,.T.);
#12140=ORIENTED_EDGE('',*,*,#9373,.T.);
#12141=ORIENTED_EDGE('',*,*,#9372,.F.);
#12142=ORIENTED_EDGE('',*,*,#9379,.T.);
#12143=ORIENTED_EDGE('',*,*,#9365,.F.);
#12144=ORIENTED_EDGE('',*,*,#9380,.T.);
#12145=ORIENTED_EDGE('',*,*,#9376,.T.);
#12146=ORIENTED_EDGE('',*,*,#9381,.T.);
#12147=ORIENTED_EDGE('',*,*,#9382,.T.);
#12148=ORIENTED_EDGE('',*,*,#9383,.T.);
#12149=ORIENTED_EDGE('',*,*,#9384,.T.);
#12150=ORIENTED_EDGE('',*,*,#9385,.T.);
#12151=ORIENTED_EDGE('',*,*,#9382,.F.);
#12152=ORIENTED_EDGE('',*,*,#9386,.F.);
#12153=ORIENTED_EDGE('',*,*,#9387,.T.);
#12154=ORIENTED_EDGE('',*,*,#9388,.F.);
#12155=ORIENTED_EDGE('',*,*,#9381,.F.);
#12156=ORIENTED_EDGE('',*,*,#9389,.F.);
#12157=ORIENTED_EDGE('',*,*,#9390,.T.);
#12158=ORIENTED_EDGE('',*,*,#9327,.T.);
#12159=ORIENTED_EDGE('',*,*,#9386,.T.);
#12160=ORIENTED_EDGE('',*,*,#9385,.F.);
#12161=ORIENTED_EDGE('',*,*,#9391,.T.);
#12162=ORIENTED_EDGE('',*,*,#9392,.T.);
#12163=ORIENTED_EDGE('',*,*,#9393,.T.);
#12164=ORIENTED_EDGE('',*,*,#9389,.T.);
#12165=ORIENTED_EDGE('',*,*,#9394,.T.);
#12166=ORIENTED_EDGE('',*,*,#9395,.T.);
#12167=ORIENTED_EDGE('',*,*,#9396,.T.);
#12168=ORIENTED_EDGE('',*,*,#9397,.T.);
#12169=ORIENTED_EDGE('',*,*,#9398,.T.);
#12170=ORIENTED_EDGE('',*,*,#9395,.F.);
#12171=ORIENTED_EDGE('',*,*,#9399,.F.);
#12172=ORIENTED_EDGE('',*,*,#9400,.T.);
#12173=ORIENTED_EDGE('',*,*,#9401,.F.);
#12174=ORIENTED_EDGE('',*,*,#9394,.F.);
#12175=ORIENTED_EDGE('',*,*,#9402,.F.);
#12176=ORIENTED_EDGE('',*,*,#9403,.T.);
#12177=ORIENTED_EDGE('',*,*,#9392,.F.);
#12178=ORIENTED_EDGE('',*,*,#9399,.T.);
#12179=ORIENTED_EDGE('',*,*,#9404,.T.);
#12180=ORIENTED_EDGE('',*,*,#9405,.T.);
#12181=ORIENTED_EDGE('',*,*,#9406,.T.);
#12182=ORIENTED_EDGE('',*,*,#9407,.T.);
#12183=ORIENTED_EDGE('',*,*,#9408,.T.);
#12184=ORIENTED_EDGE('',*,*,#9405,.F.);
#12185=ORIENTED_EDGE('',*,*,#9409,.F.);
#12186=ORIENTED_EDGE('',*,*,#9410,.T.);
#12187=ORIENTED_EDGE('',*,*,#9411,.F.);
#12188=ORIENTED_EDGE('',*,*,#9404,.F.);
#12189=ORIENTED_EDGE('',*,*,#9412,.F.);
#12190=ORIENTED_EDGE('',*,*,#9413,.T.);
#12191=ORIENTED_EDGE('',*,*,#9414,.T.);
#12192=ORIENTED_EDGE('',*,*,#9409,.T.);
#12193=ORIENTED_EDGE('',*,*,#9408,.F.);
#12194=ORIENTED_EDGE('',*,*,#9415,.T.);
#12195=ORIENTED_EDGE('',*,*,#9416,.F.);
#12196=ORIENTED_EDGE('',*,*,#9417,.T.);
#12197=ORIENTED_EDGE('',*,*,#9412,.T.);
#12198=ORIENTED_EDGE('',*,*,#9418,.T.);
#12199=ORIENTED_EDGE('',*,*,#9419,.T.);
#12200=ORIENTED_EDGE('',*,*,#9420,.T.);
#12201=ORIENTED_EDGE('',*,*,#9421,.T.);
#12202=ORIENTED_EDGE('',*,*,#9422,.T.);
#12203=ORIENTED_EDGE('',*,*,#9419,.F.);
#12204=ORIENTED_EDGE('',*,*,#9423,.F.);
#12205=ORIENTED_EDGE('',*,*,#9424,.T.);
#12206=ORIENTED_EDGE('',*,*,#9425,.F.);
#12207=ORIENTED_EDGE('',*,*,#9418,.F.);
#12208=ORIENTED_EDGE('',*,*,#9426,.F.);
#12209=ORIENTED_EDGE('',*,*,#9427,.T.);
#12210=ORIENTED_EDGE('',*,*,#9416,.T.);
#12211=ORIENTED_EDGE('',*,*,#9423,.T.);
#12212=ORIENTED_EDGE('',*,*,#9422,.F.);
#12213=ORIENTED_EDGE('',*,*,#9428,.T.);
#12214=ORIENTED_EDGE('',*,*,#9429,.F.);
#12215=ORIENTED_EDGE('',*,*,#9430,.T.);
#12216=ORIENTED_EDGE('',*,*,#9426,.T.);
#12217=ORIENTED_EDGE('',*,*,#9431,.T.);
#12218=ORIENTED_EDGE('',*,*,#9432,.T.);
#12219=ORIENTED_EDGE('',*,*,#9433,.T.);
#12220=ORIENTED_EDGE('',*,*,#9434,.T.);
#12221=ORIENTED_EDGE('',*,*,#9435,.T.);
#12222=ORIENTED_EDGE('',*,*,#9432,.F.);
#12223=ORIENTED_EDGE('',*,*,#9436,.F.);
#12224=ORIENTED_EDGE('',*,*,#9437,.T.);
#12225=ORIENTED_EDGE('',*,*,#9438,.F.);
#12226=ORIENTED_EDGE('',*,*,#9431,.F.);
#12227=ORIENTED_EDGE('',*,*,#9439,.F.);
#12228=ORIENTED_EDGE('',*,*,#9440,.T.);
#12229=ORIENTED_EDGE('',*,*,#9429,.T.);
#12230=ORIENTED_EDGE('',*,*,#9436,.T.);
#12231=ORIENTED_EDGE('',*,*,#9435,.F.);
#12232=ORIENTED_EDGE('',*,*,#9441,.T.);
#12233=ORIENTED_EDGE('',*,*,#9442,.F.);
#12234=ORIENTED_EDGE('',*,*,#9443,.T.);
#12235=ORIENTED_EDGE('',*,*,#9439,.T.);
#12236=ORIENTED_EDGE('',*,*,#9444,.T.);
#12237=ORIENTED_EDGE('',*,*,#9445,.T.);
#12238=ORIENTED_EDGE('',*,*,#9446,.T.);
#12239=ORIENTED_EDGE('',*,*,#9447,.T.);
#12240=ORIENTED_EDGE('',*,*,#9448,.T.);
#12241=ORIENTED_EDGE('',*,*,#9445,.F.);
#12242=ORIENTED_EDGE('',*,*,#9449,.F.);
#12243=ORIENTED_EDGE('',*,*,#9450,.T.);
#12244=ORIENTED_EDGE('',*,*,#9451,.F.);
#12245=ORIENTED_EDGE('',*,*,#9444,.F.);
#12246=ORIENTED_EDGE('',*,*,#9452,.F.);
#12247=ORIENTED_EDGE('',*,*,#9453,.T.);
#12248=ORIENTED_EDGE('',*,*,#9442,.T.);
#12249=ORIENTED_EDGE('',*,*,#9449,.T.);
#12250=ORIENTED_EDGE('',*,*,#9448,.F.);
#12251=ORIENTED_EDGE('',*,*,#9454,.T.);
#12252=ORIENTED_EDGE('',*,*,#9455,.F.);
#12253=ORIENTED_EDGE('',*,*,#9456,.T.);
#12254=ORIENTED_EDGE('',*,*,#9452,.T.);
#12255=ORIENTED_EDGE('',*,*,#9457,.T.);
#12256=ORIENTED_EDGE('',*,*,#9458,.T.);
#12257=ORIENTED_EDGE('',*,*,#9459,.T.);
#12258=ORIENTED_EDGE('',*,*,#9460,.T.);
#12259=ORIENTED_EDGE('',*,*,#9461,.T.);
#12260=ORIENTED_EDGE('',*,*,#9458,.F.);
#12261=ORIENTED_EDGE('',*,*,#9462,.F.);
#12262=ORIENTED_EDGE('',*,*,#9463,.T.);
#12263=ORIENTED_EDGE('',*,*,#9464,.F.);
#12264=ORIENTED_EDGE('',*,*,#9457,.F.);
#12265=ORIENTED_EDGE('',*,*,#9465,.F.);
#12266=ORIENTED_EDGE('',*,*,#9466,.T.);
#12267=ORIENTED_EDGE('',*,*,#9455,.T.);
#12268=ORIENTED_EDGE('',*,*,#9462,.T.);
#12269=ORIENTED_EDGE('',*,*,#9461,.F.);
#12270=ORIENTED_EDGE('',*,*,#9467,.T.);
#12271=ORIENTED_EDGE('',*,*,#9378,.F.);
#12272=ORIENTED_EDGE('',*,*,#9468,.T.);
#12273=ORIENTED_EDGE('',*,*,#9465,.T.);
#12274=ORIENTED_EDGE('',*,*,#9469,.T.);
#12275=ORIENTED_EDGE('',*,*,#9470,.T.);
#12276=ORIENTED_EDGE('',*,*,#9471,.T.);
#12277=ORIENTED_EDGE('',*,*,#9472,.T.);
#12278=ORIENTED_EDGE('',*,*,#9472,.F.);
#12279=ORIENTED_EDGE('',*,*,#9473,.T.);
#12280=ORIENTED_EDGE('',*,*,#9474,.T.);
#12281=ORIENTED_EDGE('',*,*,#9475,.T.);
#12282=ORIENTED_EDGE('',*,*,#9471,.F.);
#12283=ORIENTED_EDGE('',*,*,#9476,.F.);
#12284=ORIENTED_EDGE('',*,*,#9477,.F.);
#12285=ORIENTED_EDGE('',*,*,#9478,.F.);
#12286=ORIENTED_EDGE('',*,*,#9479,.F.);
#12287=ORIENTED_EDGE('',*,*,#9258,.F.);
#12288=ORIENTED_EDGE('',*,*,#9480,.F.);
#12289=ORIENTED_EDGE('',*,*,#9481,.F.);
#12290=ORIENTED_EDGE('',*,*,#9482,.F.);
#12291=ORIENTED_EDGE('',*,*,#9473,.F.);
#12292=ORIENTED_EDGE('',*,*,#9483,.T.);
#12293=ORIENTED_EDGE('',*,*,#9484,.T.);
#12294=ORIENTED_EDGE('',*,*,#9485,.T.);
#12295=ORIENTED_EDGE('',*,*,#9486,.T.);
#12296=ORIENTED_EDGE('',*,*,#9486,.F.);
#12297=ORIENTED_EDGE('',*,*,#9487,.T.);
#12298=ORIENTED_EDGE('',*,*,#9488,.T.);
#12299=ORIENTED_EDGE('',*,*,#9489,.T.);
#12300=ORIENTED_EDGE('',*,*,#9485,.F.);
#12301=ORIENTED_EDGE('',*,*,#9490,.F.);
#12302=ORIENTED_EDGE('',*,*,#9491,.F.);
#12303=ORIENTED_EDGE('',*,*,#9492,.F.);
#12304=ORIENTED_EDGE('',*,*,#9250,.F.);
#12305=ORIENTED_EDGE('',*,*,#9493,.F.);
#12306=ORIENTED_EDGE('',*,*,#9494,.F.);
#12307=ORIENTED_EDGE('',*,*,#9495,.F.);
#12308=ORIENTED_EDGE('',*,*,#9487,.F.);
#12309=ORIENTED_EDGE('',*,*,#9496,.T.);
#12310=ORIENTED_EDGE('',*,*,#9497,.T.);
#12311=ORIENTED_EDGE('',*,*,#9498,.T.);
#12312=ORIENTED_EDGE('',*,*,#9499,.T.);
#12313=ORIENTED_EDGE('',*,*,#9499,.F.);
#12314=ORIENTED_EDGE('',*,*,#9500,.T.);
#12315=ORIENTED_EDGE('',*,*,#9501,.T.);
#12316=ORIENTED_EDGE('',*,*,#9502,.T.);
#12317=ORIENTED_EDGE('',*,*,#9498,.F.);
#12318=ORIENTED_EDGE('',*,*,#9503,.F.);
#12319=ORIENTED_EDGE('',*,*,#9504,.F.);
#12320=ORIENTED_EDGE('',*,*,#9505,.F.);
#12321=ORIENTED_EDGE('',*,*,#9242,.F.);
#12322=ORIENTED_EDGE('',*,*,#9506,.F.);
#12323=ORIENTED_EDGE('',*,*,#9507,.F.);
#12324=ORIENTED_EDGE('',*,*,#9508,.F.);
#12325=ORIENTED_EDGE('',*,*,#9500,.F.);
#12326=ORIENTED_EDGE('',*,*,#9509,.T.);
#12327=ORIENTED_EDGE('',*,*,#9510,.T.);
#12328=ORIENTED_EDGE('',*,*,#9511,.T.);
#12329=ORIENTED_EDGE('',*,*,#9512,.T.);
#12330=ORIENTED_EDGE('',*,*,#9512,.F.);
#12331=ORIENTED_EDGE('',*,*,#9513,.T.);
#12332=ORIENTED_EDGE('',*,*,#9514,.T.);
#12333=ORIENTED_EDGE('',*,*,#9515,.T.);
#12334=ORIENTED_EDGE('',*,*,#9511,.F.);
#12335=ORIENTED_EDGE('',*,*,#9516,.F.);
#12336=ORIENTED_EDGE('',*,*,#9517,.F.);
#12337=ORIENTED_EDGE('',*,*,#9518,.F.);
#12338=ORIENTED_EDGE('',*,*,#9234,.F.);
#12339=ORIENTED_EDGE('',*,*,#9519,.F.);
#12340=ORIENTED_EDGE('',*,*,#9520,.F.);
#12341=ORIENTED_EDGE('',*,*,#9521,.F.);
#12342=ORIENTED_EDGE('',*,*,#9513,.F.);
#12343=ORIENTED_EDGE('',*,*,#9522,.T.);
#12344=ORIENTED_EDGE('',*,*,#9523,.T.);
#12345=ORIENTED_EDGE('',*,*,#9524,.T.);
#12346=ORIENTED_EDGE('',*,*,#9525,.T.);
#12347=ORIENTED_EDGE('',*,*,#9525,.F.);
#12348=ORIENTED_EDGE('',*,*,#9526,.T.);
#12349=ORIENTED_EDGE('',*,*,#9527,.T.);
#12350=ORIENTED_EDGE('',*,*,#9528,.T.);
#12351=ORIENTED_EDGE('',*,*,#9524,.F.);
#12352=ORIENTED_EDGE('',*,*,#9529,.F.);
#12353=ORIENTED_EDGE('',*,*,#9530,.F.);
#12354=ORIENTED_EDGE('',*,*,#9531,.F.);
#12355=ORIENTED_EDGE('',*,*,#9226,.F.);
#12356=ORIENTED_EDGE('',*,*,#9532,.F.);
#12357=ORIENTED_EDGE('',*,*,#9533,.F.);
#12358=ORIENTED_EDGE('',*,*,#9534,.F.);
#12359=ORIENTED_EDGE('',*,*,#9526,.F.);
#12360=ORIENTED_EDGE('',*,*,#9535,.T.);
#12361=ORIENTED_EDGE('',*,*,#9536,.T.);
#12362=ORIENTED_EDGE('',*,*,#9537,.T.);
#12363=ORIENTED_EDGE('',*,*,#9538,.T.);
#12364=ORIENTED_EDGE('',*,*,#9538,.F.);
#12365=ORIENTED_EDGE('',*,*,#9539,.T.);
#12366=ORIENTED_EDGE('',*,*,#9540,.T.);
#12367=ORIENTED_EDGE('',*,*,#9541,.T.);
#12368=ORIENTED_EDGE('',*,*,#9537,.F.);
#12369=ORIENTED_EDGE('',*,*,#9542,.F.);
#12370=ORIENTED_EDGE('',*,*,#9543,.F.);
#12371=ORIENTED_EDGE('',*,*,#9544,.F.);
#12372=ORIENTED_EDGE('',*,*,#9218,.F.);
#12373=ORIENTED_EDGE('',*,*,#9545,.F.);
#12374=ORIENTED_EDGE('',*,*,#9546,.F.);
#12375=ORIENTED_EDGE('',*,*,#9547,.F.);
#12376=ORIENTED_EDGE('',*,*,#9539,.F.);
#12377=ORIENTED_EDGE('',*,*,#9548,.T.);
#12378=ORIENTED_EDGE('',*,*,#9549,.T.);
#12379=ORIENTED_EDGE('',*,*,#9550,.T.);
#12380=ORIENTED_EDGE('',*,*,#9551,.T.);
#12381=ORIENTED_EDGE('',*,*,#9551,.F.);
#12382=ORIENTED_EDGE('',*,*,#9552,.T.);
#12383=ORIENTED_EDGE('',*,*,#9553,.T.);
#12384=ORIENTED_EDGE('',*,*,#9554,.T.);
#12385=ORIENTED_EDGE('',*,*,#9550,.F.);
#12386=ORIENTED_EDGE('',*,*,#9555,.F.);
#12387=ORIENTED_EDGE('',*,*,#9556,.F.);
#12388=ORIENTED_EDGE('',*,*,#9557,.F.);
#12389=ORIENTED_EDGE('',*,*,#9210,.F.);
#12390=ORIENTED_EDGE('',*,*,#9558,.F.);
#12391=ORIENTED_EDGE('',*,*,#9559,.F.);
#12392=ORIENTED_EDGE('',*,*,#9560,.F.);
#12393=ORIENTED_EDGE('',*,*,#9552,.F.);
#12394=ORIENTED_EDGE('',*,*,#9561,.T.);
#12395=ORIENTED_EDGE('',*,*,#9562,.T.);
#12396=ORIENTED_EDGE('',*,*,#9563,.T.);
#12397=ORIENTED_EDGE('',*,*,#9564,.T.);
#12398=ORIENTED_EDGE('',*,*,#9564,.F.);
#12399=ORIENTED_EDGE('',*,*,#9565,.T.);
#12400=ORIENTED_EDGE('',*,*,#9566,.T.);
#12401=ORIENTED_EDGE('',*,*,#9567,.T.);
#12402=ORIENTED_EDGE('',*,*,#9563,.F.);
#12403=ORIENTED_EDGE('',*,*,#9568,.F.);
#12404=ORIENTED_EDGE('',*,*,#9569,.F.);
#12405=ORIENTED_EDGE('',*,*,#9570,.F.);
#12406=ORIENTED_EDGE('',*,*,#9202,.F.);
#12407=ORIENTED_EDGE('',*,*,#9571,.F.);
#12408=ORIENTED_EDGE('',*,*,#9572,.F.);
#12409=ORIENTED_EDGE('',*,*,#9573,.F.);
#12410=ORIENTED_EDGE('',*,*,#9565,.F.);
#12411=ORIENTED_EDGE('',*,*,#9574,.T.);
#12412=ORIENTED_EDGE('',*,*,#9575,.T.);
#12413=ORIENTED_EDGE('',*,*,#9576,.T.);
#12414=ORIENTED_EDGE('',*,*,#9577,.T.);
#12415=ORIENTED_EDGE('',*,*,#9577,.F.);
#12416=ORIENTED_EDGE('',*,*,#9578,.T.);
#12417=ORIENTED_EDGE('',*,*,#9579,.T.);
#12418=ORIENTED_EDGE('',*,*,#9580,.T.);
#12419=ORIENTED_EDGE('',*,*,#9576,.F.);
#12420=ORIENTED_EDGE('',*,*,#9581,.F.);
#12421=ORIENTED_EDGE('',*,*,#9582,.F.);
#12422=ORIENTED_EDGE('',*,*,#9583,.F.);
#12423=ORIENTED_EDGE('',*,*,#9194,.F.);
#12424=ORIENTED_EDGE('',*,*,#9584,.F.);
#12425=ORIENTED_EDGE('',*,*,#9585,.F.);
#12426=ORIENTED_EDGE('',*,*,#9586,.F.);
#12427=ORIENTED_EDGE('',*,*,#9578,.F.);
#12428=ORIENTED_EDGE('',*,*,#9587,.T.);
#12429=ORIENTED_EDGE('',*,*,#9588,.T.);
#12430=ORIENTED_EDGE('',*,*,#9589,.T.);
#12431=ORIENTED_EDGE('',*,*,#9590,.T.);
#12432=ORIENTED_EDGE('',*,*,#9590,.F.);
#12433=ORIENTED_EDGE('',*,*,#9591,.T.);
#12434=ORIENTED_EDGE('',*,*,#9592,.T.);
#12435=ORIENTED_EDGE('',*,*,#9593,.T.);
#12436=ORIENTED_EDGE('',*,*,#9589,.F.);
#12437=ORIENTED_EDGE('',*,*,#9594,.F.);
#12438=ORIENTED_EDGE('',*,*,#9595,.F.);
#12439=ORIENTED_EDGE('',*,*,#9596,.F.);
#12440=ORIENTED_EDGE('',*,*,#9186,.F.);
#12441=ORIENTED_EDGE('',*,*,#9597,.F.);
#12442=ORIENTED_EDGE('',*,*,#9598,.F.);
#12443=ORIENTED_EDGE('',*,*,#9599,.F.);
#12444=ORIENTED_EDGE('',*,*,#9591,.F.);
#12445=ORIENTED_EDGE('',*,*,#9600,.T.);
#12446=ORIENTED_EDGE('',*,*,#9601,.T.);
#12447=ORIENTED_EDGE('',*,*,#9602,.T.);
#12448=ORIENTED_EDGE('',*,*,#9603,.T.);
#12449=ORIENTED_EDGE('',*,*,#9603,.F.);
#12450=ORIENTED_EDGE('',*,*,#9604,.T.);
#12451=ORIENTED_EDGE('',*,*,#9605,.T.);
#12452=ORIENTED_EDGE('',*,*,#9606,.T.);
#12453=ORIENTED_EDGE('',*,*,#9602,.F.);
#12454=ORIENTED_EDGE('',*,*,#9607,.F.);
#12455=ORIENTED_EDGE('',*,*,#9608,.F.);
#12456=ORIENTED_EDGE('',*,*,#9609,.F.);
#12457=ORIENTED_EDGE('',*,*,#9178,.F.);
#12458=ORIENTED_EDGE('',*,*,#9610,.F.);
#12459=ORIENTED_EDGE('',*,*,#9611,.F.);
#12460=ORIENTED_EDGE('',*,*,#9612,.F.);
#12461=ORIENTED_EDGE('',*,*,#9604,.F.);
#12462=ORIENTED_EDGE('',*,*,#9613,.T.);
#12463=ORIENTED_EDGE('',*,*,#9614,.T.);
#12464=ORIENTED_EDGE('',*,*,#9615,.T.);
#12465=ORIENTED_EDGE('',*,*,#9616,.T.);
#12466=ORIENTED_EDGE('',*,*,#9616,.F.);
#12467=ORIENTED_EDGE('',*,*,#9617,.T.);
#12468=ORIENTED_EDGE('',*,*,#9618,.T.);
#12469=ORIENTED_EDGE('',*,*,#9619,.T.);
#12470=ORIENTED_EDGE('',*,*,#9615,.F.);
#12471=ORIENTED_EDGE('',*,*,#9620,.F.);
#12472=ORIENTED_EDGE('',*,*,#9621,.F.);
#12473=ORIENTED_EDGE('',*,*,#9622,.F.);
#12474=ORIENTED_EDGE('',*,*,#9170,.F.);
#12475=ORIENTED_EDGE('',*,*,#9167,.F.);
#12476=ORIENTED_EDGE('',*,*,#9623,.F.);
#12477=ORIENTED_EDGE('',*,*,#9624,.F.);
#12478=ORIENTED_EDGE('',*,*,#9625,.F.);
#12479=ORIENTED_EDGE('',*,*,#9617,.F.);
#12480=ORIENTED_EDGE('',*,*,#9626,.T.);
#12481=ORIENTED_EDGE('',*,*,#9627,.T.);
#12482=ORIENTED_EDGE('',*,*,#9628,.T.);
#12483=ORIENTED_EDGE('',*,*,#9627,.F.);
#12484=ORIENTED_EDGE('',*,*,#9628,.F.);
#12485=ORIENTED_EDGE('',*,*,#9629,.T.);
#12486=ORIENTED_EDGE('',*,*,#9630,.T.);
#12487=ORIENTED_EDGE('',*,*,#9631,.T.);
#12488=ORIENTED_EDGE('',*,*,#9626,.F.);
#12489=ORIENTED_EDGE('',*,*,#9631,.F.);
#12490=ORIENTED_EDGE('',*,*,#9632,.T.);
#12491=ORIENTED_EDGE('',*,*,#9633,.T.);
#12492=ORIENTED_EDGE('',*,*,#9634,.T.);
#12493=ORIENTED_EDGE('',*,*,#9633,.F.);
#12494=ORIENTED_EDGE('',*,*,#9634,.F.);
#12495=ORIENTED_EDGE('',*,*,#9635,.F.);
#12496=ORIENTED_EDGE('',*,*,#9632,.F.);
#12497=ORIENTED_EDGE('',*,*,#9636,.T.);
#12498=ORIENTED_EDGE('',*,*,#9637,.T.);
#12499=ORIENTED_EDGE('',*,*,#9636,.F.);
#12500=ORIENTED_EDGE('',*,*,#9638,.T.);
#12501=ORIENTED_EDGE('',*,*,#9639,.T.);
#12502=ORIENTED_EDGE('',*,*,#9640,.T.);
#12503=ORIENTED_EDGE('',*,*,#9641,.T.);
#12504=ORIENTED_EDGE('',*,*,#9642,.T.);
#12505=ORIENTED_EDGE('',*,*,#9641,.F.);
#12506=ORIENTED_EDGE('',*,*,#9643,.T.);
#12507=ORIENTED_EDGE('',*,*,#9644,.T.);
#12508=ORIENTED_EDGE('',*,*,#9645,.T.);
#12509=ORIENTED_EDGE('',*,*,#9646,.T.);
#12510=ORIENTED_EDGE('',*,*,#9647,.T.);
#12511=ORIENTED_EDGE('',*,*,#9640,.F.);
#12512=ORIENTED_EDGE('',*,*,#9648,.T.);
#12513=ORIENTED_EDGE('',*,*,#9649,.F.);
#12514=ORIENTED_EDGE('',*,*,#9650,.F.);
#12515=ORIENTED_EDGE('',*,*,#9651,.F.);
#12516=ORIENTED_EDGE('',*,*,#9643,.F.);
#12517=ORIENTED_EDGE('',*,*,#9639,.F.);
#12518=ORIENTED_EDGE('',*,*,#9652,.T.);
#12519=ORIENTED_EDGE('',*,*,#9491,.T.);
#12520=ORIENTED_EDGE('',*,*,#9653,.T.);
#12521=ORIENTED_EDGE('',*,*,#9654,.T.);
#12522=ORIENTED_EDGE('',*,*,#9655,.T.);
#12523=ORIENTED_EDGE('',*,*,#9656,.F.);
#12524=ORIENTED_EDGE('',*,*,#9648,.F.);
#12525=ORIENTED_EDGE('',*,*,#9649,.T.);
#12526=ORIENTED_EDGE('',*,*,#9656,.T.);
#12527=ORIENTED_EDGE('',*,*,#9657,.T.);
#12528=ORIENTED_EDGE('',*,*,#9658,.T.);
#12529=ORIENTED_EDGE('',*,*,#9659,.T.);
#12530=ORIENTED_EDGE('',*,*,#9659,.F.);
#12531=ORIENTED_EDGE('',*,*,#9660,.T.);
#12532=ORIENTED_EDGE('',*,*,#9661,.F.);
#12533=ORIENTED_EDGE('',*,*,#9662,.T.);
#12534=ORIENTED_EDGE('',*,*,#9663,.T.);
#12535=ORIENTED_EDGE('',*,*,#9650,.T.);
#12536=ORIENTED_EDGE('',*,*,#9664,.T.);
#12537=ORIENTED_EDGE('',*,*,#9665,.T.);
#12538=ORIENTED_EDGE('',*,*,#9666,.T.);
#12539=ORIENTED_EDGE('',*,*,#9661,.T.);
#12540=ORIENTED_EDGE('',*,*,#9667,.T.);
#12541=ORIENTED_EDGE('',*,*,#9666,.F.);
#12542=ORIENTED_EDGE('',*,*,#9668,.T.);
#12543=ORIENTED_EDGE('',*,*,#9669,.F.);
#12544=ORIENTED_EDGE('',*,*,#9670,.F.);
#12545=ORIENTED_EDGE('',*,*,#9671,.F.);
#12546=ORIENTED_EDGE('',*,*,#9662,.F.);
#12547=ORIENTED_EDGE('',*,*,#9665,.F.);
#12548=ORIENTED_EDGE('',*,*,#9672,.T.);
#12549=ORIENTED_EDGE('',*,*,#9504,.T.);
#12550=ORIENTED_EDGE('',*,*,#9673,.T.);
#12551=ORIENTED_EDGE('',*,*,#9674,.T.);
#12552=ORIENTED_EDGE('',*,*,#9675,.T.);
#12553=ORIENTED_EDGE('',*,*,#9676,.F.);
#12554=ORIENTED_EDGE('',*,*,#9668,.F.);
#12555=ORIENTED_EDGE('',*,*,#9669,.T.);
#12556=ORIENTED_EDGE('',*,*,#9676,.T.);
#12557=ORIENTED_EDGE('',*,*,#9677,.T.);
#12558=ORIENTED_EDGE('',*,*,#9678,.T.);
#12559=ORIENTED_EDGE('',*,*,#9679,.T.);
#12560=ORIENTED_EDGE('',*,*,#9679,.F.);
#12561=ORIENTED_EDGE('',*,*,#9680,.T.);
#12562=ORIENTED_EDGE('',*,*,#9681,.F.);
#12563=ORIENTED_EDGE('',*,*,#9682,.T.);
#12564=ORIENTED_EDGE('',*,*,#9683,.T.);
#12565=ORIENTED_EDGE('',*,*,#9670,.T.);
#12566=ORIENTED_EDGE('',*,*,#9684,.T.);
#12567=ORIENTED_EDGE('',*,*,#9685,.T.);
#12568=ORIENTED_EDGE('',*,*,#9686,.T.);
#12569=ORIENTED_EDGE('',*,*,#9681,.T.);
#12570=ORIENTED_EDGE('',*,*,#9687,.T.);
#12571=ORIENTED_EDGE('',*,*,#9686,.F.);
#12572=ORIENTED_EDGE('',*,*,#9688,.T.);
#12573=ORIENTED_EDGE('',*,*,#9689,.F.);
#12574=ORIENTED_EDGE('',*,*,#9690,.F.);
#12575=ORIENTED_EDGE('',*,*,#9691,.F.);
#12576=ORIENTED_EDGE('',*,*,#9682,.F.);
#12577=ORIENTED_EDGE('',*,*,#9685,.F.);
#12578=ORIENTED_EDGE('',*,*,#9692,.T.);
#12579=ORIENTED_EDGE('',*,*,#9517,.T.);
#12580=ORIENTED_EDGE('',*,*,#9693,.T.);
#12581=ORIENTED_EDGE('',*,*,#9694,.T.);
#12582=ORIENTED_EDGE('',*,*,#9695,.T.);
#12583=ORIENTED_EDGE('',*,*,#9696,.F.);
#12584=ORIENTED_EDGE('',*,*,#9688,.F.);
#12585=ORIENTED_EDGE('',*,*,#9689,.T.);
#12586=ORIENTED_EDGE('',*,*,#9696,.T.);
#12587=ORIENTED_EDGE('',*,*,#9697,.T.);
#12588=ORIENTED_EDGE('',*,*,#9698,.T.);
#12589=ORIENTED_EDGE('',*,*,#9699,.T.);
#12590=ORIENTED_EDGE('',*,*,#9699,.F.);
#12591=ORIENTED_EDGE('',*,*,#9700,.T.);
#12592=ORIENTED_EDGE('',*,*,#9701,.F.);
#12593=ORIENTED_EDGE('',*,*,#9702,.T.);
#12594=ORIENTED_EDGE('',*,*,#9703,.T.);
#12595=ORIENTED_EDGE('',*,*,#9690,.T.);
#12596=ORIENTED_EDGE('',*,*,#9704,.T.);
#12597=ORIENTED_EDGE('',*,*,#9705,.T.);
#12598=ORIENTED_EDGE('',*,*,#9706,.T.);
#12599=ORIENTED_EDGE('',*,*,#9701,.T.);
#12600=ORIENTED_EDGE('',*,*,#9707,.T.);
#12601=ORIENTED_EDGE('',*,*,#9706,.F.);
#12602=ORIENTED_EDGE('',*,*,#9708,.T.);
#12603=ORIENTED_EDGE('',*,*,#9709,.F.);
#12604=ORIENTED_EDGE('',*,*,#9710,.F.);
#12605=ORIENTED_EDGE('',*,*,#9711,.F.);
#12606=ORIENTED_EDGE('',*,*,#9702,.F.);
#12607=ORIENTED_EDGE('',*,*,#9705,.F.);
#12608=ORIENTED_EDGE('',*,*,#9712,.T.);
#12609=ORIENTED_EDGE('',*,*,#9530,.T.);
#12610=ORIENTED_EDGE('',*,*,#9713,.T.);
#12611=ORIENTED_EDGE('',*,*,#9714,.T.);
#12612=ORIENTED_EDGE('',*,*,#9715,.T.);
#12613=ORIENTED_EDGE('',*,*,#9716,.F.);
#12614=ORIENTED_EDGE('',*,*,#9708,.F.);
#12615=ORIENTED_EDGE('',*,*,#9709,.T.);
#12616=ORIENTED_EDGE('',*,*,#9716,.T.);
#12617=ORIENTED_EDGE('',*,*,#9717,.T.);
#12618=ORIENTED_EDGE('',*,*,#9718,.T.);
#12619=ORIENTED_EDGE('',*,*,#9719,.T.);
#12620=ORIENTED_EDGE('',*,*,#9719,.F.);
#12621=ORIENTED_EDGE('',*,*,#9720,.T.);
#12622=ORIENTED_EDGE('',*,*,#9721,.F.);
#12623=ORIENTED_EDGE('',*,*,#9722,.T.);
#12624=ORIENTED_EDGE('',*,*,#9723,.T.);
#12625=ORIENTED_EDGE('',*,*,#9710,.T.);
#12626=ORIENTED_EDGE('',*,*,#9724,.T.);
#12627=ORIENTED_EDGE('',*,*,#9725,.T.);
#12628=ORIENTED_EDGE('',*,*,#9726,.T.);
#12629=ORIENTED_EDGE('',*,*,#9721,.T.);
#12630=ORIENTED_EDGE('',*,*,#9727,.T.);
#12631=ORIENTED_EDGE('',*,*,#9726,.F.);
#12632=ORIENTED_EDGE('',*,*,#9728,.T.);
#12633=ORIENTED_EDGE('',*,*,#9729,.F.);
#12634=ORIENTED_EDGE('',*,*,#9730,.F.);
#12635=ORIENTED_EDGE('',*,*,#9731,.F.);
#12636=ORIENTED_EDGE('',*,*,#9722,.F.);
#12637=ORIENTED_EDGE('',*,*,#9725,.F.);
#12638=ORIENTED_EDGE('',*,*,#9732,.T.);
#12639=ORIENTED_EDGE('',*,*,#9543,.T.);
#12640=ORIENTED_EDGE('',*,*,#9733,.T.);
#12641=ORIENTED_EDGE('',*,*,#9734,.T.);
#12642=ORIENTED_EDGE('',*,*,#9735,.T.);
#12643=ORIENTED_EDGE('',*,*,#9736,.F.);
#12644=ORIENTED_EDGE('',*,*,#9728,.F.);
#12645=ORIENTED_EDGE('',*,*,#9729,.T.);
#12646=ORIENTED_EDGE('',*,*,#9736,.T.);
#12647=ORIENTED_EDGE('',*,*,#9737,.T.);
#12648=ORIENTED_EDGE('',*,*,#9738,.T.);
#12649=ORIENTED_EDGE('',*,*,#9739,.T.);
#12650=ORIENTED_EDGE('',*,*,#9739,.F.);
#12651=ORIENTED_EDGE('',*,*,#9740,.T.);
#12652=ORIENTED_EDGE('',*,*,#9741,.T.);
#12653=ORIENTED_EDGE('',*,*,#9742,.T.);
#12654=ORIENTED_EDGE('',*,*,#9743,.T.);
#12655=ORIENTED_EDGE('',*,*,#9730,.T.);
#12656=ORIENTED_EDGE('',*,*,#9743,.F.);
#12657=ORIENTED_EDGE('',*,*,#9744,.T.);
#12658=ORIENTED_EDGE('',*,*,#9745,.F.);
#12659=ORIENTED_EDGE('',*,*,#9746,.T.);
#12660=ORIENTED_EDGE('',*,*,#9747,.F.);
#12661=ORIENTED_EDGE('',*,*,#9748,.T.);
#12662=ORIENTED_EDGE('',*,*,#9749,.F.);
#12663=ORIENTED_EDGE('',*,*,#9750,.T.);
#12664=ORIENTED_EDGE('',*,*,#9751,.F.);
#12665=ORIENTED_EDGE('',*,*,#9752,.T.);
#12666=ORIENTED_EDGE('',*,*,#9753,.F.);
#12667=ORIENTED_EDGE('',*,*,#9754,.T.);
#12668=ORIENTED_EDGE('',*,*,#9755,.F.);
#12669=ORIENTED_EDGE('',*,*,#9756,.T.);
#12670=ORIENTED_EDGE('',*,*,#9644,.F.);
#12671=ORIENTED_EDGE('',*,*,#9651,.T.);
#12672=ORIENTED_EDGE('',*,*,#9663,.F.);
#12673=ORIENTED_EDGE('',*,*,#9671,.T.);
#12674=ORIENTED_EDGE('',*,*,#9683,.F.);
#12675=ORIENTED_EDGE('',*,*,#9691,.T.);
#12676=ORIENTED_EDGE('',*,*,#9703,.F.);
#12677=ORIENTED_EDGE('',*,*,#9711,.T.);
#12678=ORIENTED_EDGE('',*,*,#9723,.F.);
#12679=ORIENTED_EDGE('',*,*,#9731,.T.);
#12680=ORIENTED_EDGE('',*,*,#9757,.F.);
#12681=ORIENTED_EDGE('',*,*,#9742,.F.);
#12682=ORIENTED_EDGE('',*,*,#9758,.F.);
#12683=ORIENTED_EDGE('',*,*,#9759,.T.);
#12684=ORIENTED_EDGE('',*,*,#9760,.F.);
#12685=ORIENTED_EDGE('',*,*,#9761,.F.);
#12686=ORIENTED_EDGE('',*,*,#9744,.F.);
#12687=ORIENTED_EDGE('',*,*,#9741,.F.);
#12688=ORIENTED_EDGE('',*,*,#9762,.T.);
#12689=ORIENTED_EDGE('',*,*,#9763,.T.);
#12690=ORIENTED_EDGE('',*,*,#9764,.T.);
#12691=ORIENTED_EDGE('',*,*,#9758,.T.);
#12692=ORIENTED_EDGE('',*,*,#9658,.F.);
#12693=ORIENTED_EDGE('',*,*,#9765,.F.);
#12694=ORIENTED_EDGE('',*,*,#9246,.F.);
#12695=ORIENTED_EDGE('',*,*,#9766,.F.);
#12696=ORIENTED_EDGE('',*,*,#9244,.F.);
#12697=ORIENTED_EDGE('',*,*,#9767,.F.);
#12698=ORIENTED_EDGE('',*,*,#9667,.F.);
#12699=ORIENTED_EDGE('',*,*,#9660,.F.);
#12700=ORIENTED_EDGE('',*,*,#9642,.F.);
#12701=ORIENTED_EDGE('',*,*,#9647,.F.);
#12702=ORIENTED_EDGE('',*,*,#9768,.F.);
#12703=ORIENTED_EDGE('',*,*,#9769,.F.);
#12704=ORIENTED_EDGE('',*,*,#9254,.F.);
#12705=ORIENTED_EDGE('',*,*,#9770,.F.);
#12706=ORIENTED_EDGE('',*,*,#9252,.F.);
#12707=ORIENTED_EDGE('',*,*,#9771,.F.);
#12708=ORIENTED_EDGE('',*,*,#9646,.F.);
#12709=ORIENTED_EDGE('',*,*,#9772,.T.);
#12710=ORIENTED_EDGE('',*,*,#9773,.T.);
#12711=ORIENTED_EDGE('',*,*,#9774,.T.);
#12712=ORIENTED_EDGE('',*,*,#9768,.T.);
#12713=ORIENTED_EDGE('',*,*,#9764,.F.);
#12714=ORIENTED_EDGE('',*,*,#9775,.T.);
#12715=ORIENTED_EDGE('',*,*,#9556,.T.);
#12716=ORIENTED_EDGE('',*,*,#9776,.T.);
#12717=ORIENTED_EDGE('',*,*,#9777,.T.);
#12718=ORIENTED_EDGE('',*,*,#9778,.T.);
#12719=ORIENTED_EDGE('',*,*,#9779,.F.);
#12720=ORIENTED_EDGE('',*,*,#9759,.F.);
#12721=ORIENTED_EDGE('',*,*,#9760,.T.);
#12722=ORIENTED_EDGE('',*,*,#9779,.T.);
#12723=ORIENTED_EDGE('',*,*,#9780,.T.);
#12724=ORIENTED_EDGE('',*,*,#9781,.T.);
#12725=ORIENTED_EDGE('',*,*,#9782,.T.);
#12726=ORIENTED_EDGE('',*,*,#9782,.F.);
#12727=ORIENTED_EDGE('',*,*,#9783,.T.);
#12728=ORIENTED_EDGE('',*,*,#9784,.T.);
#12729=ORIENTED_EDGE('',*,*,#9785,.T.);
#12730=ORIENTED_EDGE('',*,*,#9745,.T.);
#12731=ORIENTED_EDGE('',*,*,#9761,.T.);
#12732=ORIENTED_EDGE('',*,*,#9785,.F.);
#12733=ORIENTED_EDGE('',*,*,#9786,.F.);
#12734=ORIENTED_EDGE('',*,*,#9787,.T.);
#12735=ORIENTED_EDGE('',*,*,#9788,.F.);
#12736=ORIENTED_EDGE('',*,*,#9789,.F.);
#12737=ORIENTED_EDGE('',*,*,#9746,.F.);
#12738=ORIENTED_EDGE('',*,*,#9784,.F.);
#12739=ORIENTED_EDGE('',*,*,#9790,.T.);
#12740=ORIENTED_EDGE('',*,*,#9791,.T.);
#12741=ORIENTED_EDGE('',*,*,#9792,.T.);
#12742=ORIENTED_EDGE('',*,*,#9786,.T.);
#12743=ORIENTED_EDGE('',*,*,#9792,.F.);
#12744=ORIENTED_EDGE('',*,*,#9793,.T.);
#12745=ORIENTED_EDGE('',*,*,#9569,.T.);
#12746=ORIENTED_EDGE('',*,*,#9794,.T.);
#12747=ORIENTED_EDGE('',*,*,#9795,.T.);
#12748=ORIENTED_EDGE('',*,*,#9796,.T.);
#12749=ORIENTED_EDGE('',*,*,#9797,.F.);
#12750=ORIENTED_EDGE('',*,*,#9787,.F.);
#12751=ORIENTED_EDGE('',*,*,#9788,.T.);
#12752=ORIENTED_EDGE('',*,*,#9797,.T.);
#12753=ORIENTED_EDGE('',*,*,#9798,.T.);
#12754=ORIENTED_EDGE('',*,*,#9799,.T.);
#12755=ORIENTED_EDGE('',*,*,#9800,.T.);
#12756=ORIENTED_EDGE('',*,*,#9800,.F.);
#12757=ORIENTED_EDGE('',*,*,#9801,.T.);
#12758=ORIENTED_EDGE('',*,*,#9802,.T.);
#12759=ORIENTED_EDGE('',*,*,#9803,.T.);
#12760=ORIENTED_EDGE('',*,*,#9747,.T.);
#12761=ORIENTED_EDGE('',*,*,#9789,.T.);
#12762=ORIENTED_EDGE('',*,*,#9803,.F.);
#12763=ORIENTED_EDGE('',*,*,#9804,.F.);
#12764=ORIENTED_EDGE('',*,*,#9805,.T.);
#12765=ORIENTED_EDGE('',*,*,#9806,.F.);
#12766=ORIENTED_EDGE('',*,*,#9807,.F.);
#12767=ORIENTED_EDGE('',*,*,#9748,.F.);
#12768=ORIENTED_EDGE('',*,*,#9802,.F.);
#12769=ORIENTED_EDGE('',*,*,#9808,.T.);
#12770=ORIENTED_EDGE('',*,*,#9809,.T.);
#12771=ORIENTED_EDGE('',*,*,#9810,.T.);
#12772=ORIENTED_EDGE('',*,*,#9804,.T.);
#12773=ORIENTED_EDGE('',*,*,#9810,.F.);
#12774=ORIENTED_EDGE('',*,*,#9811,.T.);
#12775=ORIENTED_EDGE('',*,*,#9582,.T.);
#12776=ORIENTED_EDGE('',*,*,#9812,.T.);
#12777=ORIENTED_EDGE('',*,*,#9813,.T.);
#12778=ORIENTED_EDGE('',*,*,#9814,.T.);
#12779=ORIENTED_EDGE('',*,*,#9815,.F.);
#12780=ORIENTED_EDGE('',*,*,#9805,.F.);
#12781=ORIENTED_EDGE('',*,*,#9806,.T.);
#12782=ORIENTED_EDGE('',*,*,#9815,.T.);
#12783=ORIENTED_EDGE('',*,*,#9816,.T.);
#12784=ORIENTED_EDGE('',*,*,#9817,.T.);
#12785=ORIENTED_EDGE('',*,*,#9818,.T.);
#12786=ORIENTED_EDGE('',*,*,#9818,.F.);
#12787=ORIENTED_EDGE('',*,*,#9819,.T.);
#12788=ORIENTED_EDGE('',*,*,#9820,.T.);
#12789=ORIENTED_EDGE('',*,*,#9821,.T.);
#12790=ORIENTED_EDGE('',*,*,#9749,.T.);
#12791=ORIENTED_EDGE('',*,*,#9807,.T.);
#12792=ORIENTED_EDGE('',*,*,#9821,.F.);
#12793=ORIENTED_EDGE('',*,*,#9822,.F.);
#12794=ORIENTED_EDGE('',*,*,#9823,.T.);
#12795=ORIENTED_EDGE('',*,*,#9824,.F.);
#12796=ORIENTED_EDGE('',*,*,#9825,.F.);
#12797=ORIENTED_EDGE('',*,*,#9750,.F.);
#12798=ORIENTED_EDGE('',*,*,#9820,.F.);
#12799=ORIENTED_EDGE('',*,*,#9826,.T.);
#12800=ORIENTED_EDGE('',*,*,#9827,.T.);
#12801=ORIENTED_EDGE('',*,*,#9828,.T.);
#12802=ORIENTED_EDGE('',*,*,#9822,.T.);
#12803=ORIENTED_EDGE('',*,*,#9828,.F.);
#12804=ORIENTED_EDGE('',*,*,#9829,.T.);
#12805=ORIENTED_EDGE('',*,*,#9595,.T.);
#12806=ORIENTED_EDGE('',*,*,#9830,.T.);
#12807=ORIENTED_EDGE('',*,*,#9831,.T.);
#12808=ORIENTED_EDGE('',*,*,#9832,.T.);
#12809=ORIENTED_EDGE('',*,*,#9833,.F.);
#12810=ORIENTED_EDGE('',*,*,#9823,.F.);
#12811=ORIENTED_EDGE('',*,*,#9824,.T.);
#12812=ORIENTED_EDGE('',*,*,#9833,.T.);
#12813=ORIENTED_EDGE('',*,*,#9834,.T.);
#12814=ORIENTED_EDGE('',*,*,#9835,.T.);
#12815=ORIENTED_EDGE('',*,*,#9836,.T.);
#12816=ORIENTED_EDGE('',*,*,#9836,.F.);
#12817=ORIENTED_EDGE('',*,*,#9837,.T.);
#12818=ORIENTED_EDGE('',*,*,#9838,.T.);
#12819=ORIENTED_EDGE('',*,*,#9839,.T.);
#12820=ORIENTED_EDGE('',*,*,#9751,.T.);
#12821=ORIENTED_EDGE('',*,*,#9825,.T.);
#12822=ORIENTED_EDGE('',*,*,#9839,.F.);
#12823=ORIENTED_EDGE('',*,*,#9840,.F.);
#12824=ORIENTED_EDGE('',*,*,#9841,.T.);
#12825=ORIENTED_EDGE('',*,*,#9842,.F.);
#12826=ORIENTED_EDGE('',*,*,#9843,.F.);
#12827=ORIENTED_EDGE('',*,*,#9752,.F.);
#12828=ORIENTED_EDGE('',*,*,#9838,.F.);
#12829=ORIENTED_EDGE('',*,*,#9844,.T.);
#12830=ORIENTED_EDGE('',*,*,#9845,.T.);
#12831=ORIENTED_EDGE('',*,*,#9846,.T.);
#12832=ORIENTED_EDGE('',*,*,#9840,.T.);
#12833=ORIENTED_EDGE('',*,*,#9846,.F.);
#12834=ORIENTED_EDGE('',*,*,#9847,.T.);
#12835=ORIENTED_EDGE('',*,*,#9608,.T.);
#12836=ORIENTED_EDGE('',*,*,#9848,.T.);
#12837=ORIENTED_EDGE('',*,*,#9849,.T.);
#12838=ORIENTED_EDGE('',*,*,#9850,.T.);
#12839=ORIENTED_EDGE('',*,*,#9851,.F.);
#12840=ORIENTED_EDGE('',*,*,#9841,.F.);
#12841=ORIENTED_EDGE('',*,*,#9842,.T.);
#12842=ORIENTED_EDGE('',*,*,#9851,.T.);
#12843=ORIENTED_EDGE('',*,*,#9852,.T.);
#12844=ORIENTED_EDGE('',*,*,#9853,.T.);
#12845=ORIENTED_EDGE('',*,*,#9854,.T.);
#12846=ORIENTED_EDGE('',*,*,#9854,.F.);
#12847=ORIENTED_EDGE('',*,*,#9855,.T.);
#12848=ORIENTED_EDGE('',*,*,#9856,.T.);
#12849=ORIENTED_EDGE('',*,*,#9857,.T.);
#12850=ORIENTED_EDGE('',*,*,#9753,.T.);
#12851=ORIENTED_EDGE('',*,*,#9843,.T.);
#12852=ORIENTED_EDGE('',*,*,#9857,.F.);
#12853=ORIENTED_EDGE('',*,*,#9858,.F.);
#12854=ORIENTED_EDGE('',*,*,#9859,.T.);
#12855=ORIENTED_EDGE('',*,*,#9860,.F.);
#12856=ORIENTED_EDGE('',*,*,#9861,.F.);
#12857=ORIENTED_EDGE('',*,*,#9754,.F.);
#12858=ORIENTED_EDGE('',*,*,#9856,.F.);
#12859=ORIENTED_EDGE('',*,*,#9862,.T.);
#12860=ORIENTED_EDGE('',*,*,#9863,.T.);
#12861=ORIENTED_EDGE('',*,*,#9864,.T.);
#12862=ORIENTED_EDGE('',*,*,#9858,.T.);
#12863=ORIENTED_EDGE('',*,*,#9773,.F.);
#12864=ORIENTED_EDGE('',*,*,#9865,.F.);
#12865=ORIENTED_EDGE('',*,*,#9866,.F.);
#12866=ORIENTED_EDGE('',*,*,#9867,.T.);
#12867=ORIENTED_EDGE('',*,*,#9477,.T.);
#12868=ORIENTED_EDGE('',*,*,#9868,.T.);
#12869=ORIENTED_EDGE('',*,*,#9869,.T.);
#12870=ORIENTED_EDGE('',*,*,#9870,.T.);
#12871=ORIENTED_EDGE('',*,*,#9645,.F.);
#12872=ORIENTED_EDGE('',*,*,#9756,.F.);
#12873=ORIENTED_EDGE('',*,*,#9871,.F.);
#12874=ORIENTED_EDGE('',*,*,#9872,.F.);
#12875=ORIENTED_EDGE('',*,*,#9865,.T.);
#12876=ORIENTED_EDGE('',*,*,#9772,.F.);
#12877=ORIENTED_EDGE('',*,*,#9864,.F.);
#12878=ORIENTED_EDGE('',*,*,#9873,.T.);
#12879=ORIENTED_EDGE('',*,*,#9621,.T.);
#12880=ORIENTED_EDGE('',*,*,#9874,.T.);
#12881=ORIENTED_EDGE('',*,*,#9875,.T.);
#12882=ORIENTED_EDGE('',*,*,#9876,.T.);
#12883=ORIENTED_EDGE('',*,*,#9877,.F.);
#12884=ORIENTED_EDGE('',*,*,#9859,.F.);
#12885=ORIENTED_EDGE('',*,*,#9860,.T.);
#12886=ORIENTED_EDGE('',*,*,#9877,.T.);
#12887=ORIENTED_EDGE('',*,*,#9878,.T.);
#12888=ORIENTED_EDGE('',*,*,#9879,.T.);
#12889=ORIENTED_EDGE('',*,*,#9880,.T.);
#12890=ORIENTED_EDGE('',*,*,#9880,.F.);
#12891=ORIENTED_EDGE('',*,*,#9881,.T.);
#12892=ORIENTED_EDGE('',*,*,#9882,.T.);
#12893=ORIENTED_EDGE('',*,*,#9871,.T.);
#12894=ORIENTED_EDGE('',*,*,#9755,.T.);
#12895=ORIENTED_EDGE('',*,*,#9861,.T.);
#12896=ORIENTED_EDGE('',*,*,#9882,.F.);
#12897=ORIENTED_EDGE('',*,*,#9883,.T.);
#12898=ORIENTED_EDGE('',*,*,#9884,.T.);
#12899=ORIENTED_EDGE('',*,*,#9866,.T.);
#12900=ORIENTED_EDGE('',*,*,#9872,.T.);
#12901=ORIENTED_EDGE('',*,*,#9884,.F.);
#12902=ORIENTED_EDGE('',*,*,#9885,.T.);
#12903=ORIENTED_EDGE('',*,*,#9886,.T.);
#12904=ORIENTED_EDGE('',*,*,#9478,.T.);
#12905=ORIENTED_EDGE('',*,*,#9867,.F.);
#12906=ORIENTED_EDGE('',*,*,#9879,.F.);
#12907=ORIENTED_EDGE('',*,*,#9887,.F.);
#12908=ORIENTED_EDGE('',*,*,#9888,.F.);
#12909=ORIENTED_EDGE('',*,*,#9889,.F.);
#12910=ORIENTED_EDGE('',*,*,#9890,.F.);
#12911=ORIENTED_EDGE('',*,*,#9885,.F.);
#12912=ORIENTED_EDGE('',*,*,#9883,.F.);
#12913=ORIENTED_EDGE('',*,*,#9881,.F.);
#12914=ORIENTED_EDGE('',*,*,#9261,.T.);
#12915=ORIENTED_EDGE('',*,*,#9891,.T.);
#12916=ORIENTED_EDGE('',*,*,#9892,.F.);
#12917=ORIENTED_EDGE('',*,*,#9893,.F.);
#12918=ORIENTED_EDGE('',*,*,#9894,.T.);
#12919=ORIENTED_EDGE('',*,*,#9894,.F.);
#12920=ORIENTED_EDGE('',*,*,#9895,.F.);
#12921=ORIENTED_EDGE('',*,*,#9163,.F.);
#12922=ORIENTED_EDGE('',*,*,#9160,.F.);
#12923=ORIENTED_EDGE('',*,*,#9157,.F.);
#12924=ORIENTED_EDGE('',*,*,#9154,.F.);
#12925=ORIENTED_EDGE('',*,*,#9151,.F.);
#12926=ORIENTED_EDGE('',*,*,#9148,.F.);
#12927=ORIENTED_EDGE('',*,*,#9145,.F.);
#12928=ORIENTED_EDGE('',*,*,#9142,.F.);
#12929=ORIENTED_EDGE('',*,*,#9139,.F.);
#12930=ORIENTED_EDGE('',*,*,#9136,.F.);
#12931=ORIENTED_EDGE('',*,*,#9133,.F.);
#12932=ORIENTED_EDGE('',*,*,#9130,.F.);
#12933=ORIENTED_EDGE('',*,*,#9127,.F.);
#12934=ORIENTED_EDGE('',*,*,#9124,.F.);
#12935=ORIENTED_EDGE('',*,*,#9121,.F.);
#12936=ORIENTED_EDGE('',*,*,#9118,.F.);
#12937=ORIENTED_EDGE('',*,*,#9896,.F.);
#12938=ORIENTED_EDGE('',*,*,#9897,.T.);
#12939=ORIENTED_EDGE('',*,*,#9307,.T.);
#12940=ORIENTED_EDGE('',*,*,#9304,.T.);
#12941=ORIENTED_EDGE('',*,*,#9301,.T.);
#12942=ORIENTED_EDGE('',*,*,#9298,.T.);
#12943=ORIENTED_EDGE('',*,*,#9295,.T.);
#12944=ORIENTED_EDGE('',*,*,#9292,.T.);
#12945=ORIENTED_EDGE('',*,*,#9289,.T.);
#12946=ORIENTED_EDGE('',*,*,#9286,.T.);
#12947=ORIENTED_EDGE('',*,*,#9283,.T.);
#12948=ORIENTED_EDGE('',*,*,#9280,.T.);
#12949=ORIENTED_EDGE('',*,*,#9277,.T.);
#12950=ORIENTED_EDGE('',*,*,#9274,.T.);
#12951=ORIENTED_EDGE('',*,*,#9271,.T.);
#12952=ORIENTED_EDGE('',*,*,#9268,.T.);
#12953=ORIENTED_EDGE('',*,*,#9265,.T.);
#12954=ORIENTED_EDGE('',*,*,#9262,.T.);
#12955=ORIENTED_EDGE('',*,*,#9898,.T.);
#12956=ORIENTED_EDGE('',*,*,#9899,.T.);
#12957=ORIENTED_EDGE('',*,*,#9900,.T.);
#12958=ORIENTED_EDGE('',*,*,#9901,.T.);
#12959=ORIENTED_EDGE('',*,*,#9896,.T.);
#12960=ORIENTED_EDGE('',*,*,#9305,.T.);
#12961=ORIENTED_EDGE('',*,*,#9897,.F.);
#12962=ORIENTED_EDGE('',*,*,#9901,.F.);
#12963=ORIENTED_EDGE('',*,*,#9902,.T.);
#12964=ORIENTED_EDGE('',*,*,#9891,.F.);
#12965=ORIENTED_EDGE('',*,*,#9260,.F.);
#12966=ORIENTED_EDGE('',*,*,#9264,.F.);
#12967=ORIENTED_EDGE('',*,*,#9267,.F.);
#12968=ORIENTED_EDGE('',*,*,#9270,.F.);
#12969=ORIENTED_EDGE('',*,*,#9273,.F.);
#12970=ORIENTED_EDGE('',*,*,#9276,.F.);
#12971=ORIENTED_EDGE('',*,*,#9279,.F.);
#12972=ORIENTED_EDGE('',*,*,#9282,.F.);
#12973=ORIENTED_EDGE('',*,*,#9285,.F.);
#12974=ORIENTED_EDGE('',*,*,#9288,.F.);
#12975=ORIENTED_EDGE('',*,*,#9291,.F.);
#12976=ORIENTED_EDGE('',*,*,#9294,.F.);
#12977=ORIENTED_EDGE('',*,*,#9297,.F.);
#12978=ORIENTED_EDGE('',*,*,#9300,.F.);
#12979=ORIENTED_EDGE('',*,*,#9303,.F.);
#12980=ORIENTED_EDGE('',*,*,#9306,.F.);
#12981=ORIENTED_EDGE('',*,*,#9902,.F.);
#12982=ORIENTED_EDGE('',*,*,#9900,.F.);
#12983=ORIENTED_EDGE('',*,*,#9116,.F.);
#12984=ORIENTED_EDGE('',*,*,#9120,.F.);
#12985=ORIENTED_EDGE('',*,*,#9123,.F.);
#12986=ORIENTED_EDGE('',*,*,#9126,.F.);
#12987=ORIENTED_EDGE('',*,*,#9129,.F.);
#12988=ORIENTED_EDGE('',*,*,#9132,.F.);
#12989=ORIENTED_EDGE('',*,*,#9135,.F.);
#12990=ORIENTED_EDGE('',*,*,#9138,.F.);
#12991=ORIENTED_EDGE('',*,*,#9141,.F.);
#12992=ORIENTED_EDGE('',*,*,#9144,.F.);
#12993=ORIENTED_EDGE('',*,*,#9147,.F.);
#12994=ORIENTED_EDGE('',*,*,#9150,.F.);
#12995=ORIENTED_EDGE('',*,*,#9153,.F.);
#12996=ORIENTED_EDGE('',*,*,#9156,.F.);
#12997=ORIENTED_EDGE('',*,*,#9159,.F.);
#12998=ORIENTED_EDGE('',*,*,#9162,.F.);
#12999=ORIENTED_EDGE('',*,*,#9903,.F.);
#13000=ORIENTED_EDGE('',*,*,#9904,.F.);
#13001=ORIENTED_EDGE('',*,*,#9889,.T.);
#13002=ORIENTED_EDGE('',*,*,#9164,.T.);
#13003=ORIENTED_EDGE('',*,*,#9479,.T.);
#13004=ORIENTED_EDGE('',*,*,#9886,.F.);
#13005=ORIENTED_EDGE('',*,*,#9890,.T.);
#13006=ORIENTED_EDGE('',*,*,#9904,.T.);
#13007=ORIENTED_EDGE('',*,*,#9888,.T.);
#13008=ORIENTED_EDGE('',*,*,#9905,.F.);
#13009=ORIENTED_EDGE('',*,*,#9906,.T.);
#13010=ORIENTED_EDGE('',*,*,#9878,.F.);
#13011=ORIENTED_EDGE('',*,*,#9876,.F.);
#13012=ORIENTED_EDGE('',*,*,#9907,.T.);
#13013=ORIENTED_EDGE('',*,*,#9905,.T.);
#13014=ORIENTED_EDGE('',*,*,#9887,.T.);
#13015=ORIENTED_EDGE('',*,*,#9173,.F.);
#13016=ORIENTED_EDGE('',*,*,#9908,.T.);
#13017=ORIENTED_EDGE('',*,*,#9853,.F.);
#13018=ORIENTED_EDGE('',*,*,#9909,.F.);
#13019=ORIENTED_EDGE('',*,*,#9174,.F.);
#13020=ORIENTED_EDGE('',*,*,#9908,.F.);
#13021=ORIENTED_EDGE('',*,*,#9172,.F.);
#13022=ORIENTED_EDGE('',*,*,#9910,.F.);
#13023=ORIENTED_EDGE('',*,*,#9862,.F.);
#13024=ORIENTED_EDGE('',*,*,#9855,.F.);
#13025=ORIENTED_EDGE('',*,*,#9852,.F.);
#13026=ORIENTED_EDGE('',*,*,#9850,.F.);
#13027=ORIENTED_EDGE('',*,*,#9911,.T.);
#13028=ORIENTED_EDGE('',*,*,#9175,.T.);
#13029=ORIENTED_EDGE('',*,*,#9909,.T.);
#13030=ORIENTED_EDGE('',*,*,#9863,.F.);
#13031=ORIENTED_EDGE('',*,*,#9910,.T.);
#13032=ORIENTED_EDGE('',*,*,#9171,.T.);
#13033=ORIENTED_EDGE('',*,*,#9622,.T.);
#13034=ORIENTED_EDGE('',*,*,#9873,.F.);
#13035=ORIENTED_EDGE('',*,*,#9181,.F.);
#13036=ORIENTED_EDGE('',*,*,#9912,.T.);
#13037=ORIENTED_EDGE('',*,*,#9835,.F.);
#13038=ORIENTED_EDGE('',*,*,#9913,.F.);
#13039=ORIENTED_EDGE('',*,*,#9182,.F.);
#13040=ORIENTED_EDGE('',*,*,#9912,.F.);
#13041=ORIENTED_EDGE('',*,*,#9180,.F.);
#13042=ORIENTED_EDGE('',*,*,#9914,.F.);
#13043=ORIENTED_EDGE('',*,*,#9844,.F.);
#13044=ORIENTED_EDGE('',*,*,#9837,.F.);
#13045=ORIENTED_EDGE('',*,*,#9834,.F.);
#13046=ORIENTED_EDGE('',*,*,#9832,.F.);
#13047=ORIENTED_EDGE('',*,*,#9915,.T.);
#13048=ORIENTED_EDGE('',*,*,#9183,.T.);
#13049=ORIENTED_EDGE('',*,*,#9913,.T.);
#13050=ORIENTED_EDGE('',*,*,#9845,.F.);
#13051=ORIENTED_EDGE('',*,*,#9914,.T.);
#13052=ORIENTED_EDGE('',*,*,#9179,.T.);
#13053=ORIENTED_EDGE('',*,*,#9609,.T.);
#13054=ORIENTED_EDGE('',*,*,#9847,.F.);
#13055=ORIENTED_EDGE('',*,*,#9189,.F.);
#13056=ORIENTED_EDGE('',*,*,#9916,.T.);
#13057=ORIENTED_EDGE('',*,*,#9817,.F.);
#13058=ORIENTED_EDGE('',*,*,#9917,.F.);
#13059=ORIENTED_EDGE('',*,*,#9190,.F.);
#13060=ORIENTED_EDGE('',*,*,#9916,.F.);
#13061=ORIENTED_EDGE('',*,*,#9188,.F.);
#13062=ORIENTED_EDGE('',*,*,#9918,.F.);
#13063=ORIENTED_EDGE('',*,*,#9826,.F.);
#13064=ORIENTED_EDGE('',*,*,#9819,.F.);
#13065=ORIENTED_EDGE('',*,*,#9816,.F.);
#13066=ORIENTED_EDGE('',*,*,#9814,.F.);
#13067=ORIENTED_EDGE('',*,*,#9919,.T.);
#13068=ORIENTED_EDGE('',*,*,#9191,.T.);
#13069=ORIENTED_EDGE('',*,*,#9917,.T.);
#13070=ORIENTED_EDGE('',*,*,#9827,.F.);
#13071=ORIENTED_EDGE('',*,*,#9918,.T.);
#13072=ORIENTED_EDGE('',*,*,#9187,.T.);
#13073=ORIENTED_EDGE('',*,*,#9596,.T.);
#13074=ORIENTED_EDGE('',*,*,#9829,.F.);
#13075=ORIENTED_EDGE('',*,*,#9197,.F.);
#13076=ORIENTED_EDGE('',*,*,#9920,.T.);
#13077=ORIENTED_EDGE('',*,*,#9799,.F.);
#13078=ORIENTED_EDGE('',*,*,#9921,.F.);
#13079=ORIENTED_EDGE('',*,*,#9198,.F.);
#13080=ORIENTED_EDGE('',*,*,#9920,.F.);
#13081=ORIENTED_EDGE('',*,*,#9196,.F.);
#13082=ORIENTED_EDGE('',*,*,#9922,.F.);
#13083=ORIENTED_EDGE('',*,*,#9808,.F.);
#13084=ORIENTED_EDGE('',*,*,#9801,.F.);
#13085=ORIENTED_EDGE('',*,*,#9798,.F.);
#13086=ORIENTED_EDGE('',*,*,#9796,.F.);
#13087=ORIENTED_EDGE('',*,*,#9923,.T.);
#13088=ORIENTED_EDGE('',*,*,#9199,.T.);
#13089=ORIENTED_EDGE('',*,*,#9921,.T.);
#13090=ORIENTED_EDGE('',*,*,#9809,.F.);
#13091=ORIENTED_EDGE('',*,*,#9922,.T.);
#13092=ORIENTED_EDGE('',*,*,#9195,.T.);
#13093=ORIENTED_EDGE('',*,*,#9583,.T.);
#13094=ORIENTED_EDGE('',*,*,#9811,.F.);
#13095=ORIENTED_EDGE('',*,*,#9205,.F.);
#13096=ORIENTED_EDGE('',*,*,#9924,.T.);
#13097=ORIENTED_EDGE('',*,*,#9781,.F.);
#13098=ORIENTED_EDGE('',*,*,#9925,.F.);
#13099=ORIENTED_EDGE('',*,*,#9206,.F.);
#13100=ORIENTED_EDGE('',*,*,#9924,.F.);
#13101=ORIENTED_EDGE('',*,*,#9204,.F.);
#13102=ORIENTED_EDGE('',*,*,#9926,.F.);
#13103=ORIENTED_EDGE('',*,*,#9790,.F.);
#13104=ORIENTED_EDGE('',*,*,#9783,.F.);
#13105=ORIENTED_EDGE('',*,*,#9780,.F.);
#13106=ORIENTED_EDGE('',*,*,#9778,.F.);
#13107=ORIENTED_EDGE('',*,*,#9927,.T.);
#13108=ORIENTED_EDGE('',*,*,#9207,.T.);
#13109=ORIENTED_EDGE('',*,*,#9925,.T.);
#13110=ORIENTED_EDGE('',*,*,#9791,.F.);
#13111=ORIENTED_EDGE('',*,*,#9926,.T.);
#13112=ORIENTED_EDGE('',*,*,#9203,.T.);
#13113=ORIENTED_EDGE('',*,*,#9570,.T.);
#13114=ORIENTED_EDGE('',*,*,#9793,.F.);
#13115=ORIENTED_EDGE('',*,*,#9213,.F.);
#13116=ORIENTED_EDGE('',*,*,#9928,.T.);
#13117=ORIENTED_EDGE('',*,*,#9738,.F.);
#13118=ORIENTED_EDGE('',*,*,#9929,.F.);
#13119=ORIENTED_EDGE('',*,*,#9214,.F.);
#13120=ORIENTED_EDGE('',*,*,#9928,.F.);
#13121=ORIENTED_EDGE('',*,*,#9212,.F.);
#13122=ORIENTED_EDGE('',*,*,#9930,.F.);
#13123=ORIENTED_EDGE('',*,*,#9762,.F.);
#13124=ORIENTED_EDGE('',*,*,#9740,.F.);
#13125=ORIENTED_EDGE('',*,*,#9737,.F.);
#13126=ORIENTED_EDGE('',*,*,#9735,.F.);
#13127=ORIENTED_EDGE('',*,*,#9931,.T.);
#13128=ORIENTED_EDGE('',*,*,#9215,.T.);
#13129=ORIENTED_EDGE('',*,*,#9929,.T.);
#13130=ORIENTED_EDGE('',*,*,#9763,.F.);
#13131=ORIENTED_EDGE('',*,*,#9930,.T.);
#13132=ORIENTED_EDGE('',*,*,#9211,.T.);
#13133=ORIENTED_EDGE('',*,*,#9557,.T.);
#13134=ORIENTED_EDGE('',*,*,#9775,.F.);
#13135=ORIENTED_EDGE('',*,*,#9221,.F.);
#13136=ORIENTED_EDGE('',*,*,#9932,.T.);
#13137=ORIENTED_EDGE('',*,*,#9718,.F.);
#13138=ORIENTED_EDGE('',*,*,#9933,.F.);
#13139=ORIENTED_EDGE('',*,*,#9222,.F.);
#13140=ORIENTED_EDGE('',*,*,#9932,.F.);
#13141=ORIENTED_EDGE('',*,*,#9220,.F.);
#13142=ORIENTED_EDGE('',*,*,#9934,.F.);
#13143=ORIENTED_EDGE('',*,*,#9727,.F.);
#13144=ORIENTED_EDGE('',*,*,#9720,.F.);
#13145=ORIENTED_EDGE('',*,*,#9717,.F.);
#13146=ORIENTED_EDGE('',*,*,#9715,.F.);
#13147=ORIENTED_EDGE('',*,*,#9935,.T.);
#13148=ORIENTED_EDGE('',*,*,#9223,.T.);
#13149=ORIENTED_EDGE('',*,*,#9933,.T.);
#13150=ORIENTED_EDGE('',*,*,#9724,.F.);
#13151=ORIENTED_EDGE('',*,*,#9934,.T.);
#13152=ORIENTED_EDGE('',*,*,#9219,.T.);
#13153=ORIENTED_EDGE('',*,*,#9544,.T.);
#13154=ORIENTED_EDGE('',*,*,#9732,.F.);
#13155=ORIENTED_EDGE('',*,*,#9229,.F.);
#13156=ORIENTED_EDGE('',*,*,#9936,.T.);
#13157=ORIENTED_EDGE('',*,*,#9698,.F.);
#13158=ORIENTED_EDGE('',*,*,#9937,.F.);
#13159=ORIENTED_EDGE('',*,*,#9230,.F.);
#13160=ORIENTED_EDGE('',*,*,#9936,.F.);
#13161=ORIENTED_EDGE('',*,*,#9228,.F.);
#13162=ORIENTED_EDGE('',*,*,#9938,.F.);
#13163=ORIENTED_EDGE('',*,*,#9707,.F.);
#13164=ORIENTED_EDGE('',*,*,#9700,.F.);
#13165=ORIENTED_EDGE('',*,*,#9697,.F.);
#13166=ORIENTED_EDGE('',*,*,#9695,.F.);
#13167=ORIENTED_EDGE('',*,*,#9939,.T.);
#13168=ORIENTED_EDGE('',*,*,#9231,.T.);
#13169=ORIENTED_EDGE('',*,*,#9937,.T.);
#13170=ORIENTED_EDGE('',*,*,#9704,.F.);
#13171=ORIENTED_EDGE('',*,*,#9938,.T.);
#13172=ORIENTED_EDGE('',*,*,#9227,.T.);
#13173=ORIENTED_EDGE('',*,*,#9531,.T.);
#13174=ORIENTED_EDGE('',*,*,#9712,.F.);
#13175=ORIENTED_EDGE('',*,*,#9237,.F.);
#13176=ORIENTED_EDGE('',*,*,#9940,.T.);
#13177=ORIENTED_EDGE('',*,*,#9678,.F.);
#13178=ORIENTED_EDGE('',*,*,#9941,.F.);
#13179=ORIENTED_EDGE('',*,*,#9238,.F.);
#13180=ORIENTED_EDGE('',*,*,#9940,.F.);
#13181=ORIENTED_EDGE('',*,*,#9236,.F.);
#13182=ORIENTED_EDGE('',*,*,#9942,.F.);
#13183=ORIENTED_EDGE('',*,*,#9687,.F.);
#13184=ORIENTED_EDGE('',*,*,#9680,.F.);
#13185=ORIENTED_EDGE('',*,*,#9677,.F.);
#13186=ORIENTED_EDGE('',*,*,#9675,.F.);
#13187=ORIENTED_EDGE('',*,*,#9943,.T.);
#13188=ORIENTED_EDGE('',*,*,#9239,.T.);
#13189=ORIENTED_EDGE('',*,*,#9941,.T.);
#13190=ORIENTED_EDGE('',*,*,#9684,.F.);
#13191=ORIENTED_EDGE('',*,*,#9942,.T.);
#13192=ORIENTED_EDGE('',*,*,#9235,.T.);
#13193=ORIENTED_EDGE('',*,*,#9518,.T.);
#13194=ORIENTED_EDGE('',*,*,#9692,.F.);
#13195=ORIENTED_EDGE('',*,*,#9245,.F.);
#13196=ORIENTED_EDGE('',*,*,#9766,.T.);
#13197=ORIENTED_EDGE('',*,*,#9657,.F.);
#13198=ORIENTED_EDGE('',*,*,#9655,.F.);
#13199=ORIENTED_EDGE('',*,*,#9944,.T.);
#13200=ORIENTED_EDGE('',*,*,#9247,.T.);
#13201=ORIENTED_EDGE('',*,*,#9765,.T.);
#13202=ORIENTED_EDGE('',*,*,#9664,.F.);
#13203=ORIENTED_EDGE('',*,*,#9767,.T.);
#13204=ORIENTED_EDGE('',*,*,#9243,.T.);
#13205=ORIENTED_EDGE('',*,*,#9505,.T.);
#13206=ORIENTED_EDGE('',*,*,#9672,.F.);
#13207=ORIENTED_EDGE('',*,*,#9253,.F.);
#13208=ORIENTED_EDGE('',*,*,#9770,.T.);
#13209=ORIENTED_EDGE('',*,*,#9774,.F.);
#13210=ORIENTED_EDGE('',*,*,#9870,.F.);
#13211=ORIENTED_EDGE('',*,*,#9945,.T.);
#13212=ORIENTED_EDGE('',*,*,#9255,.T.);
#13213=ORIENTED_EDGE('',*,*,#9769,.T.);
#13214=ORIENTED_EDGE('',*,*,#9638,.F.);
#13215=ORIENTED_EDGE('',*,*,#9771,.T.);
#13216=ORIENTED_EDGE('',*,*,#9251,.T.);
#13217=ORIENTED_EDGE('',*,*,#9492,.T.);
#13218=ORIENTED_EDGE('',*,*,#9652,.F.);
#13219=ORIENTED_EDGE('',*,*,#9946,.T.);
#13220=ORIENTED_EDGE('',*,*,#9947,.T.);
#13221=ORIENTED_EDGE('',*,*,#9948,.F.);
#13222=ORIENTED_EDGE('',*,*,#9947,.F.);
#13223=ORIENTED_EDGE('',*,*,#9630,.F.);
#13224=ORIENTED_EDGE('',*,*,#9946,.F.);
#13225=ORIENTED_EDGE('',*,*,#9949,.F.);
#13226=ORIENTED_EDGE('',*,*,#9948,.T.);
#13227=ORIENTED_EDGE('',*,*,#9950,.F.);
#13228=ORIENTED_EDGE('',*,*,#9951,.T.);
#13229=ORIENTED_EDGE('',*,*,#9949,.T.);
#13230=ORIENTED_EDGE('',*,*,#9951,.F.);
#13231=ORIENTED_EDGE('',*,*,#9635,.T.);
#13232=ORIENTED_EDGE('',*,*,#9952,.T.);
#13233=ORIENTED_EDGE('',*,*,#9629,.F.);
#13234=ORIENTED_EDGE('',*,*,#9952,.F.);
#13235=ORIENTED_EDGE('',*,*,#9166,.F.);
#13236=ORIENTED_EDGE('',*,*,#9953,.T.);
#13237=ORIENTED_EDGE('',*,*,#9954,.F.);
#13238=ORIENTED_EDGE('',*,*,#9623,.T.);
#13239=ORIENTED_EDGE('',*,*,#9614,.F.);
#13240=ORIENTED_EDGE('',*,*,#9955,.T.);
#13241=ORIENTED_EDGE('',*,*,#9874,.F.);
#13242=ORIENTED_EDGE('',*,*,#9620,.T.);
#13243=ORIENTED_EDGE('',*,*,#9956,.T.);
#13244=ORIENTED_EDGE('',*,*,#9618,.F.);
#13245=ORIENTED_EDGE('',*,*,#9625,.T.);
#13246=ORIENTED_EDGE('',*,*,#9624,.T.);
#13247=ORIENTED_EDGE('',*,*,#9954,.T.);
#13248=ORIENTED_EDGE('',*,*,#9613,.F.);
#13249=ORIENTED_EDGE('',*,*,#9619,.F.);
#13250=ORIENTED_EDGE('',*,*,#9956,.F.);
#13251=ORIENTED_EDGE('',*,*,#9953,.F.);
#13252=ORIENTED_EDGE('',*,*,#9165,.F.);
#13253=ORIENTED_EDGE('',*,*,#9906,.F.);
#13254=ORIENTED_EDGE('',*,*,#9907,.F.);
#13255=ORIENTED_EDGE('',*,*,#9875,.F.);
#13256=ORIENTED_EDGE('',*,*,#9955,.F.);
#13257=ORIENTED_EDGE('',*,*,#9177,.F.);
#13258=ORIENTED_EDGE('',*,*,#9957,.T.);
#13259=ORIENTED_EDGE('',*,*,#9958,.F.);
#13260=ORIENTED_EDGE('',*,*,#9610,.T.);
#13261=ORIENTED_EDGE('',*,*,#9601,.F.);
#13262=ORIENTED_EDGE('',*,*,#9959,.T.);
#13263=ORIENTED_EDGE('',*,*,#9848,.F.);
#13264=ORIENTED_EDGE('',*,*,#9607,.T.);
#13265=ORIENTED_EDGE('',*,*,#9960,.T.);
#13266=ORIENTED_EDGE('',*,*,#9605,.F.);
#13267=ORIENTED_EDGE('',*,*,#9612,.T.);
#13268=ORIENTED_EDGE('',*,*,#9611,.T.);
#13269=ORIENTED_EDGE('',*,*,#9958,.T.);
#13270=ORIENTED_EDGE('',*,*,#9600,.F.);
#13271=ORIENTED_EDGE('',*,*,#9606,.F.);
#13272=ORIENTED_EDGE('',*,*,#9960,.F.);
#13273=ORIENTED_EDGE('',*,*,#9957,.F.);
#13274=ORIENTED_EDGE('',*,*,#9176,.F.);
#13275=ORIENTED_EDGE('',*,*,#9911,.F.);
#13276=ORIENTED_EDGE('',*,*,#9849,.F.);
#13277=ORIENTED_EDGE('',*,*,#9959,.F.);
#13278=ORIENTED_EDGE('',*,*,#9185,.F.);
#13279=ORIENTED_EDGE('',*,*,#9961,.T.);
#13280=ORIENTED_EDGE('',*,*,#9962,.F.);
#13281=ORIENTED_EDGE('',*,*,#9597,.T.);
#13282=ORIENTED_EDGE('',*,*,#9588,.F.);
#13283=ORIENTED_EDGE('',*,*,#9963,.T.);
#13284=ORIENTED_EDGE('',*,*,#9830,.F.);
#13285=ORIENTED_EDGE('',*,*,#9594,.T.);
#13286=ORIENTED_EDGE('',*,*,#9964,.T.);
#13287=ORIENTED_EDGE('',*,*,#9592,.F.);
#13288=ORIENTED_EDGE('',*,*,#9599,.T.);
#13289=ORIENTED_EDGE('',*,*,#9598,.T.);
#13290=ORIENTED_EDGE('',*,*,#9962,.T.);
#13291=ORIENTED_EDGE('',*,*,#9587,.F.);
#13292=ORIENTED_EDGE('',*,*,#9593,.F.);
#13293=ORIENTED_EDGE('',*,*,#9964,.F.);
#13294=ORIENTED_EDGE('',*,*,#9961,.F.);
#13295=ORIENTED_EDGE('',*,*,#9184,.F.);
#13296=ORIENTED_EDGE('',*,*,#9915,.F.);
#13297=ORIENTED_EDGE('',*,*,#9831,.F.);
#13298=ORIENTED_EDGE('',*,*,#9963,.F.);
#13299=ORIENTED_EDGE('',*,*,#9193,.F.);
#13300=ORIENTED_EDGE('',*,*,#9965,.T.);
#13301=ORIENTED_EDGE('',*,*,#9966,.F.);
#13302=ORIENTED_EDGE('',*,*,#9584,.T.);
#13303=ORIENTED_EDGE('',*,*,#9575,.F.);
#13304=ORIENTED_EDGE('',*,*,#9967,.T.);
#13305=ORIENTED_EDGE('',*,*,#9812,.F.);
#13306=ORIENTED_EDGE('',*,*,#9581,.T.);
#13307=ORIENTED_EDGE('',*,*,#9968,.T.);
#13308=ORIENTED_EDGE('',*,*,#9579,.F.);
#13309=ORIENTED_EDGE('',*,*,#9586,.T.);
#13310=ORIENTED_EDGE('',*,*,#9585,.T.);
#13311=ORIENTED_EDGE('',*,*,#9966,.T.);
#13312=ORIENTED_EDGE('',*,*,#9574,.F.);
#13313=ORIENTED_EDGE('',*,*,#9580,.F.);
#13314=ORIENTED_EDGE('',*,*,#9968,.F.);
#13315=ORIENTED_EDGE('',*,*,#9965,.F.);
#13316=ORIENTED_EDGE('',*,*,#9192,.F.);
#13317=ORIENTED_EDGE('',*,*,#9919,.F.);
#13318=ORIENTED_EDGE('',*,*,#9813,.F.);
#13319=ORIENTED_EDGE('',*,*,#9967,.F.);
#13320=ORIENTED_EDGE('',*,*,#9201,.F.);
#13321=ORIENTED_EDGE('',*,*,#9969,.T.);
#13322=ORIENTED_EDGE('',*,*,#9970,.F.);
#13323=ORIENTED_EDGE('',*,*,#9571,.T.);
#13324=ORIENTED_EDGE('',*,*,#9562,.F.);
#13325=ORIENTED_EDGE('',*,*,#9971,.T.);
#13326=ORIENTED_EDGE('',*,*,#9794,.F.);
#13327=ORIENTED_EDGE('',*,*,#9568,.T.);
#13328=ORIENTED_EDGE('',*,*,#9972,.T.);
#13329=ORIENTED_EDGE('',*,*,#9566,.F.);
#13330=ORIENTED_EDGE('',*,*,#9573,.T.);
#13331=ORIENTED_EDGE('',*,*,#9572,.T.);
#13332=ORIENTED_EDGE('',*,*,#9970,.T.);
#13333=ORIENTED_EDGE('',*,*,#9561,.F.);
#13334=ORIENTED_EDGE('',*,*,#9567,.F.);
#13335=ORIENTED_EDGE('',*,*,#9972,.F.);
#13336=ORIENTED_EDGE('',*,*,#9969,.F.);
#13337=ORIENTED_EDGE('',*,*,#9200,.F.);
#13338=ORIENTED_EDGE('',*,*,#9923,.F.);
#13339=ORIENTED_EDGE('',*,*,#9795,.F.);
#13340=ORIENTED_EDGE('',*,*,#9971,.F.);
#13341=ORIENTED_EDGE('',*,*,#9209,.F.);
#13342=ORIENTED_EDGE('',*,*,#9973,.T.);
#13343=ORIENTED_EDGE('',*,*,#9974,.F.);
#13344=ORIENTED_EDGE('',*,*,#9558,.T.);
#13345=ORIENTED_EDGE('',*,*,#9549,.F.);
#13346=ORIENTED_EDGE('',*,*,#9975,.T.);
#13347=ORIENTED_EDGE('',*,*,#9776,.F.);
#13348=ORIENTED_EDGE('',*,*,#9555,.T.);
#13349=ORIENTED_EDGE('',*,*,#9976,.T.);
#13350=ORIENTED_EDGE('',*,*,#9553,.F.);
#13351=ORIENTED_EDGE('',*,*,#9560,.T.);
#13352=ORIENTED_EDGE('',*,*,#9559,.T.);
#13353=ORIENTED_EDGE('',*,*,#9974,.T.);
#13354=ORIENTED_EDGE('',*,*,#9548,.F.);
#13355=ORIENTED_EDGE('',*,*,#9554,.F.);
#13356=ORIENTED_EDGE('',*,*,#9976,.F.);
#13357=ORIENTED_EDGE('',*,*,#9973,.F.);
#13358=ORIENTED_EDGE('',*,*,#9208,.F.);
#13359=ORIENTED_EDGE('',*,*,#9927,.F.);
#13360=ORIENTED_EDGE('',*,*,#9777,.F.);
#13361=ORIENTED_EDGE('',*,*,#9975,.F.);
#13362=ORIENTED_EDGE('',*,*,#9217,.F.);
#13363=ORIENTED_EDGE('',*,*,#9977,.T.);
#13364=ORIENTED_EDGE('',*,*,#9978,.F.);
#13365=ORIENTED_EDGE('',*,*,#9545,.T.);
#13366=ORIENTED_EDGE('',*,*,#9536,.F.);
#13367=ORIENTED_EDGE('',*,*,#9979,.T.);
#13368=ORIENTED_EDGE('',*,*,#9733,.F.);
#13369=ORIENTED_EDGE('',*,*,#9542,.T.);
#13370=ORIENTED_EDGE('',*,*,#9980,.T.);
#13371=ORIENTED_EDGE('',*,*,#9540,.F.);
#13372=ORIENTED_EDGE('',*,*,#9547,.T.);
#13373=ORIENTED_EDGE('',*,*,#9546,.T.);
#13374=ORIENTED_EDGE('',*,*,#9978,.T.);
#13375=ORIENTED_EDGE('',*,*,#9535,.F.);
#13376=ORIENTED_EDGE('',*,*,#9541,.F.);
#13377=ORIENTED_EDGE('',*,*,#9980,.F.);
#13378=ORIENTED_EDGE('',*,*,#9977,.F.);
#13379=ORIENTED_EDGE('',*,*,#9216,.F.);
#13380=ORIENTED_EDGE('',*,*,#9931,.F.);
#13381=ORIENTED_EDGE('',*,*,#9734,.F.);
#13382=ORIENTED_EDGE('',*,*,#9979,.F.);
#13383=ORIENTED_EDGE('',*,*,#9225,.F.);
#13384=ORIENTED_EDGE('',*,*,#9981,.T.);
#13385=ORIENTED_EDGE('',*,*,#9982,.F.);
#13386=ORIENTED_EDGE('',*,*,#9532,.T.);
#13387=ORIENTED_EDGE('',*,*,#9523,.F.);
#13388=ORIENTED_EDGE('',*,*,#9983,.T.);
#13389=ORIENTED_EDGE('',*,*,#9713,.F.);
#13390=ORIENTED_EDGE('',*,*,#9529,.T.);
#13391=ORIENTED_EDGE('',*,*,#9984,.T.);
#13392=ORIENTED_EDGE('',*,*,#9527,.F.);
#13393=ORIENTED_EDGE('',*,*,#9534,.T.);
#13394=ORIENTED_EDGE('',*,*,#9533,.T.);
#13395=ORIENTED_EDGE('',*,*,#9982,.T.);
#13396=ORIENTED_EDGE('',*,*,#9522,.F.);
#13397=ORIENTED_EDGE('',*,*,#9528,.F.);
#13398=ORIENTED_EDGE('',*,*,#9984,.F.);
#13399=ORIENTED_EDGE('',*,*,#9981,.F.);
#13400=ORIENTED_EDGE('',*,*,#9224,.F.);
#13401=ORIENTED_EDGE('',*,*,#9935,.F.);
#13402=ORIENTED_EDGE('',*,*,#9714,.F.);
#13403=ORIENTED_EDGE('',*,*,#9983,.F.);
#13404=ORIENTED_EDGE('',*,*,#9233,.F.);
#13405=ORIENTED_EDGE('',*,*,#9985,.T.);
#13406=ORIENTED_EDGE('',*,*,#9986,.F.);
#13407=ORIENTED_EDGE('',*,*,#9519,.T.);
#13408=ORIENTED_EDGE('',*,*,#9510,.F.);
#13409=ORIENTED_EDGE('',*,*,#9987,.T.);
#13410=ORIENTED_EDGE('',*,*,#9693,.F.);
#13411=ORIENTED_EDGE('',*,*,#9516,.T.);
#13412=ORIENTED_EDGE('',*,*,#9988,.T.);
#13413=ORIENTED_EDGE('',*,*,#9514,.F.);
#13414=ORIENTED_EDGE('',*,*,#9521,.T.);
#13415=ORIENTED_EDGE('',*,*,#9520,.T.);
#13416=ORIENTED_EDGE('',*,*,#9986,.T.);
#13417=ORIENTED_EDGE('',*,*,#9509,.F.);
#13418=ORIENTED_EDGE('',*,*,#9515,.F.);
#13419=ORIENTED_EDGE('',*,*,#9988,.F.);
#13420=ORIENTED_EDGE('',*,*,#9985,.F.);
#13421=ORIENTED_EDGE('',*,*,#9232,.F.);
#13422=ORIENTED_EDGE('',*,*,#9939,.F.);
#13423=ORIENTED_EDGE('',*,*,#9694,.F.);
#13424=ORIENTED_EDGE('',*,*,#9987,.F.);
#13425=ORIENTED_EDGE('',*,*,#9241,.F.);
#13426=ORIENTED_EDGE('',*,*,#9989,.T.);
#13427=ORIENTED_EDGE('',*,*,#9990,.F.);
#13428=ORIENTED_EDGE('',*,*,#9506,.T.);
#13429=ORIENTED_EDGE('',*,*,#9497,.F.);
#13430=ORIENTED_EDGE('',*,*,#9991,.T.);
#13431=ORIENTED_EDGE('',*,*,#9673,.F.);
#13432=ORIENTED_EDGE('',*,*,#9503,.T.);
#13433=ORIENTED_EDGE('',*,*,#9992,.T.);
#13434=ORIENTED_EDGE('',*,*,#9501,.F.);
#13435=ORIENTED_EDGE('',*,*,#9508,.T.);
#13436=ORIENTED_EDGE('',*,*,#9507,.T.);
#13437=ORIENTED_EDGE('',*,*,#9990,.T.);
#13438=ORIENTED_EDGE('',*,*,#9496,.F.);
#13439=ORIENTED_EDGE('',*,*,#9502,.F.);
#13440=ORIENTED_EDGE('',*,*,#9992,.F.);
#13441=ORIENTED_EDGE('',*,*,#9989,.F.);
#13442=ORIENTED_EDGE('',*,*,#9240,.F.);
#13443=ORIENTED_EDGE('',*,*,#9943,.F.);
#13444=ORIENTED_EDGE('',*,*,#9674,.F.);
#13445=ORIENTED_EDGE('',*,*,#9991,.F.);
#13446=ORIENTED_EDGE('',*,*,#9249,.F.);
#13447=ORIENTED_EDGE('',*,*,#9993,.T.);
#13448=ORIENTED_EDGE('',*,*,#9994,.F.);
#13449=ORIENTED_EDGE('',*,*,#9493,.T.);
#13450=ORIENTED_EDGE('',*,*,#9484,.F.);
#13451=ORIENTED_EDGE('',*,*,#9995,.T.);
#13452=ORIENTED_EDGE('',*,*,#9653,.F.);
#13453=ORIENTED_EDGE('',*,*,#9490,.T.);
#13454=ORIENTED_EDGE('',*,*,#9996,.T.);
#13455=ORIENTED_EDGE('',*,*,#9488,.F.);
#13456=ORIENTED_EDGE('',*,*,#9495,.T.);
#13457=ORIENTED_EDGE('',*,*,#9494,.T.);
#13458=ORIENTED_EDGE('',*,*,#9994,.T.);
#13459=ORIENTED_EDGE('',*,*,#9483,.F.);
#13460=ORIENTED_EDGE('',*,*,#9489,.F.);
#13461=ORIENTED_EDGE('',*,*,#9996,.F.);
#13462=ORIENTED_EDGE('',*,*,#9993,.F.);
#13463=ORIENTED_EDGE('',*,*,#9248,.F.);
#13464=ORIENTED_EDGE('',*,*,#9944,.F.);
#13465=ORIENTED_EDGE('',*,*,#9654,.F.);
#13466=ORIENTED_EDGE('',*,*,#9995,.F.);
#13467=ORIENTED_EDGE('',*,*,#9257,.F.);
#13468=ORIENTED_EDGE('',*,*,#9997,.T.);
#13469=ORIENTED_EDGE('',*,*,#9998,.F.);
#13470=ORIENTED_EDGE('',*,*,#9480,.T.);
#13471=ORIENTED_EDGE('',*,*,#9470,.F.);
#13472=ORIENTED_EDGE('',*,*,#9999,.T.);
#13473=ORIENTED_EDGE('',*,*,#9868,.F.);
#13474=ORIENTED_EDGE('',*,*,#9476,.T.);
#13475=ORIENTED_EDGE('',*,*,#10000,.T.);
#13476=ORIENTED_EDGE('',*,*,#9474,.F.);
#13477=ORIENTED_EDGE('',*,*,#9482,.T.);
#13478=ORIENTED_EDGE('',*,*,#9481,.T.);
#13479=ORIENTED_EDGE('',*,*,#9998,.T.);
#13480=ORIENTED_EDGE('',*,*,#9469,.F.);
#13481=ORIENTED_EDGE('',*,*,#9475,.F.);
#13482=ORIENTED_EDGE('',*,*,#10000,.F.);
#13483=ORIENTED_EDGE('',*,*,#9997,.F.);
#13484=ORIENTED_EDGE('',*,*,#9256,.F.);
#13485=ORIENTED_EDGE('',*,*,#9945,.F.);
#13486=ORIENTED_EDGE('',*,*,#9869,.F.);
#13487=ORIENTED_EDGE('',*,*,#9999,.F.);
#13488=ORIENTED_EDGE('',*,*,#9398,.F.);
#13489=ORIENTED_EDGE('',*,*,#10001,.T.);
#13490=ORIENTED_EDGE('',*,*,#9414,.F.);
#13491=ORIENTED_EDGE('',*,*,#10002,.T.);
#13492=ORIENTED_EDGE('',*,*,#9402,.T.);
#13493=ORIENTED_EDGE('',*,*,#9447,.F.);
#13494=ORIENTED_EDGE('',*,*,#10003,.F.);
#13495=ORIENTED_EDGE('',*,*,#9463,.F.);
#13496=ORIENTED_EDGE('',*,*,#9454,.F.);
#13497=ORIENTED_EDGE('',*,*,#9434,.F.);
#13498=ORIENTED_EDGE('',*,*,#10004,.F.);
#13499=ORIENTED_EDGE('',*,*,#9450,.F.);
#13500=ORIENTED_EDGE('',*,*,#9441,.F.);
#13501=ORIENTED_EDGE('',*,*,#9421,.F.);
#13502=ORIENTED_EDGE('',*,*,#10005,.F.);
#13503=ORIENTED_EDGE('',*,*,#9437,.F.);
#13504=ORIENTED_EDGE('',*,*,#9428,.F.);
#13505=ORIENTED_EDGE('',*,*,#9407,.F.);
#13506=ORIENTED_EDGE('',*,*,#10006,.F.);
#13507=ORIENTED_EDGE('',*,*,#9424,.F.);
#13508=ORIENTED_EDGE('',*,*,#9415,.F.);
#13509=ORIENTED_EDGE('',*,*,#9397,.F.);
#13510=ORIENTED_EDGE('',*,*,#10007,.F.);
#13511=ORIENTED_EDGE('',*,*,#9410,.F.);
#13512=ORIENTED_EDGE('',*,*,#10001,.F.);
#13513=ORIENTED_EDGE('',*,*,#9384,.F.);
#13514=ORIENTED_EDGE('',*,*,#10008,.F.);
#13515=ORIENTED_EDGE('',*,*,#9400,.F.);
#13516=ORIENTED_EDGE('',*,*,#9391,.F.);
#13517=ORIENTED_EDGE('',*,*,#9393,.F.);
#13518=ORIENTED_EDGE('',*,*,#9403,.F.);
#13519=ORIENTED_EDGE('',*,*,#10002,.F.);
#13520=ORIENTED_EDGE('',*,*,#9413,.F.);
#13521=ORIENTED_EDGE('',*,*,#9417,.F.);
#13522=ORIENTED_EDGE('',*,*,#9427,.F.);
#13523=ORIENTED_EDGE('',*,*,#9430,.F.);
#13524=ORIENTED_EDGE('',*,*,#9440,.F.);
#13525=ORIENTED_EDGE('',*,*,#9443,.F.);
#13526=ORIENTED_EDGE('',*,*,#9453,.F.);
#13527=ORIENTED_EDGE('',*,*,#9456,.F.);
#13528=ORIENTED_EDGE('',*,*,#9466,.F.);
#13529=ORIENTED_EDGE('',*,*,#9468,.F.);
#13530=ORIENTED_EDGE('',*,*,#9377,.F.);
#13531=ORIENTED_EDGE('',*,*,#9380,.F.);
#13532=ORIENTED_EDGE('',*,*,#9364,.F.);
#13533=ORIENTED_EDGE('',*,*,#9367,.F.);
#13534=ORIENTED_EDGE('',*,*,#9351,.F.);
#13535=ORIENTED_EDGE('',*,*,#9354,.F.);
#13536=ORIENTED_EDGE('',*,*,#9338,.F.);
#13537=ORIENTED_EDGE('',*,*,#9341,.F.);
#13538=ORIENTED_EDGE('',*,*,#9324,.F.);
#13539=ORIENTED_EDGE('',*,*,#9328,.F.);
#13540=ORIENTED_EDGE('',*,*,#9390,.F.);
#13541=ORIENTED_EDGE('',*,*,#9371,.F.);
#13542=ORIENTED_EDGE('',*,*,#10009,.F.);
#13543=ORIENTED_EDGE('',*,*,#9361,.F.);
#13544=ORIENTED_EDGE('',*,*,#9379,.F.);
#13545=ORIENTED_EDGE('',*,*,#9358,.F.);
#13546=ORIENTED_EDGE('',*,*,#10010,.F.);
#13547=ORIENTED_EDGE('',*,*,#9348,.F.);
#13548=ORIENTED_EDGE('',*,*,#9366,.F.);
#13549=ORIENTED_EDGE('',*,*,#9345,.F.);
#13550=ORIENTED_EDGE('',*,*,#10011,.F.);
#13551=ORIENTED_EDGE('',*,*,#9335,.F.);
#13552=ORIENTED_EDGE('',*,*,#9353,.F.);
#13553=ORIENTED_EDGE('',*,*,#9332,.F.);
#13554=ORIENTED_EDGE('',*,*,#10012,.F.);
#13555=ORIENTED_EDGE('',*,*,#9321,.F.);
#13556=ORIENTED_EDGE('',*,*,#9340,.F.);
#13557=ORIENTED_EDGE('',*,*,#9318,.F.);
#13558=ORIENTED_EDGE('',*,*,#10013,.F.);
#13559=ORIENTED_EDGE('',*,*,#9387,.F.);
#13560=ORIENTED_EDGE('',*,*,#9326,.F.);
#13561=ORIENTED_EDGE('',*,*,#9460,.F.);
#13562=ORIENTED_EDGE('',*,*,#10014,.F.);
#13563=ORIENTED_EDGE('',*,*,#9374,.F.);
#13564=ORIENTED_EDGE('',*,*,#9467,.F.);
#13565=ORIENTED_EDGE('',*,*,#9169,.F.);
#13566=ORIENTED_EDGE('',*,*,#9401,.T.);
#13567=ORIENTED_EDGE('',*,*,#10008,.T.);
#13568=ORIENTED_EDGE('',*,*,#9383,.F.);
#13569=ORIENTED_EDGE('',*,*,#9388,.T.);
#13570=ORIENTED_EDGE('',*,*,#10013,.T.);
#13571=ORIENTED_EDGE('',*,*,#9317,.F.);
#13572=ORIENTED_EDGE('',*,*,#9322,.T.);
#13573=ORIENTED_EDGE('',*,*,#10012,.T.);
#13574=ORIENTED_EDGE('',*,*,#9331,.F.);
#13575=ORIENTED_EDGE('',*,*,#9336,.T.);
#13576=ORIENTED_EDGE('',*,*,#10011,.T.);
#13577=ORIENTED_EDGE('',*,*,#9344,.F.);
#13578=ORIENTED_EDGE('',*,*,#9349,.T.);
#13579=ORIENTED_EDGE('',*,*,#10010,.T.);
#13580=ORIENTED_EDGE('',*,*,#9357,.F.);
#13581=ORIENTED_EDGE('',*,*,#9362,.T.);
#13582=ORIENTED_EDGE('',*,*,#10009,.T.);
#13583=ORIENTED_EDGE('',*,*,#9370,.F.);
#13584=ORIENTED_EDGE('',*,*,#9375,.T.);
#13585=ORIENTED_EDGE('',*,*,#10014,.T.);
#13586=ORIENTED_EDGE('',*,*,#9459,.F.);
#13587=ORIENTED_EDGE('',*,*,#9464,.T.);
#13588=ORIENTED_EDGE('',*,*,#10003,.T.);
#13589=ORIENTED_EDGE('',*,*,#9446,.F.);
#13590=ORIENTED_EDGE('',*,*,#9451,.T.);
#13591=ORIENTED_EDGE('',*,*,#10004,.T.);
#13592=ORIENTED_EDGE('',*,*,#9433,.F.);
#13593=ORIENTED_EDGE('',*,*,#9438,.T.);
#13594=ORIENTED_EDGE('',*,*,#10005,.T.);
#13595=ORIENTED_EDGE('',*,*,#9420,.F.);
#13596=ORIENTED_EDGE('',*,*,#9425,.T.);
#13597=ORIENTED_EDGE('',*,*,#10006,.T.);
#13598=ORIENTED_EDGE('',*,*,#9406,.F.);
#13599=ORIENTED_EDGE('',*,*,#9411,.T.);
#13600=ORIENTED_EDGE('',*,*,#10007,.T.);
#13601=ORIENTED_EDGE('',*,*,#9396,.F.);
#13602=ORIENTED_EDGE('',*,*,#10015,.F.);
#13603=ORIENTED_EDGE('',*,*,#10016,.T.);
#13604=ORIENTED_EDGE('',*,*,#9757,.T.);
#13605=ORIENTED_EDGE('',*,*,#10016,.F.);
#13606=ORIENTED_EDGE('',*,*,#9313,.F.);
#13607=ORIENTED_EDGE('',*,*,#10017,.T.);
#13608=ORIENTED_EDGE('',*,*,#10015,.T.);
#13609=ORIENTED_EDGE('',*,*,#10017,.F.);
#13610=ORIENTED_EDGE('',*,*,#9637,.F.);
#13611=ORIENTED_EDGE('',*,*,#10018,.T.);
#13612=ORIENTED_EDGE('',*,*,#9314,.T.);
#13613=ORIENTED_EDGE('',*,*,#10018,.F.);
#13614=ORIENTED_EDGE('',*,*,#10019,.F.);
#13615=ORIENTED_EDGE('',*,*,#10020,.T.);
#13616=ORIENTED_EDGE('',*,*,#9950,.T.);
#13617=ORIENTED_EDGE('',*,*,#10020,.F.);
#13618=ORIENTED_EDGE('',*,*,#10019,.T.);
#13619=ORIENTED_EDGE('',*,*,#10021,.F.);
#13620=ORIENTED_EDGE('',*,*,#10022,.F.);
#13621=ORIENTED_EDGE('',*,*,#10023,.T.);
#13622=ORIENTED_EDGE('',*,*,#10021,.T.);
#13623=ORIENTED_EDGE('',*,*,#10023,.F.);
#13624=ORIENTED_EDGE('',*,*,#10024,.F.);
#13625=ORIENTED_EDGE('',*,*,#10025,.T.);
#13626=ORIENTED_EDGE('',*,*,#10022,.T.);
#13627=ORIENTED_EDGE('',*,*,#10025,.F.);
#13628=ORIENTED_EDGE('',*,*,#10026,.F.);
#13629=ORIENTED_EDGE('',*,*,#10027,.T.);
#13630=ORIENTED_EDGE('',*,*,#10024,.T.);
#13631=ORIENTED_EDGE('',*,*,#10027,.F.);
#13632=ORIENTED_EDGE('',*,*,#10028,.F.);
#13633=ORIENTED_EDGE('',*,*,#10029,.T.);
#13634=ORIENTED_EDGE('',*,*,#10026,.T.);
#13635=ORIENTED_EDGE('',*,*,#10029,.F.);
#13636=ORIENTED_EDGE('',*,*,#10028,.T.);
#13637=ORIENTED_EDGE('',*,*,#10030,.F.);
#13638=ORIENTED_EDGE('',*,*,#10031,.F.);
#13639=ORIENTED_EDGE('',*,*,#10032,.T.);
#13640=ORIENTED_EDGE('',*,*,#10030,.T.);
#13641=ORIENTED_EDGE('',*,*,#10032,.F.);
#13642=ORIENTED_EDGE('',*,*,#10033,.F.);
#13643=ORIENTED_EDGE('',*,*,#10034,.T.);
#13644=ORIENTED_EDGE('',*,*,#10031,.T.);
#13645=ORIENTED_EDGE('',*,*,#10034,.F.);
#13646=ORIENTED_EDGE('',*,*,#10035,.F.);
#13647=ORIENTED_EDGE('',*,*,#10036,.T.);
#13648=ORIENTED_EDGE('',*,*,#10033,.T.);
#13649=ORIENTED_EDGE('',*,*,#10036,.F.);
#13650=ORIENTED_EDGE('',*,*,#10037,.F.);
#13651=ORIENTED_EDGE('',*,*,#10038,.T.);
#13652=ORIENTED_EDGE('',*,*,#10035,.T.);
#13653=ORIENTED_EDGE('',*,*,#10038,.F.);
#13654=ORIENTED_EDGE('',*,*,#10039,.F.);
#13655=ORIENTED_EDGE('',*,*,#10040,.T.);
#13656=ORIENTED_EDGE('',*,*,#10037,.T.);
#13657=ORIENTED_EDGE('',*,*,#10040,.F.);
#13658=ORIENTED_EDGE('',*,*,#9898,.F.);
#13659=ORIENTED_EDGE('',*,*,#9117,.F.);
#13660=ORIENTED_EDGE('',*,*,#9899,.F.);
#13661=ORIENTED_EDGE('',*,*,#10041,.T.);
#13662=ORIENTED_EDGE('',*,*,#10039,.T.);
#13663=ORIENTED_EDGE('',*,*,#10041,.F.);
#13664=ORIENTED_EDGE('',*,*,#9161,.T.);
#13665=ORIENTED_EDGE('',*,*,#9895,.T.);
#13666=ORIENTED_EDGE('',*,*,#10042,.F.);
#13667=ORIENTED_EDGE('',*,*,#9903,.T.);
#13668=ORIENTED_EDGE('',*,*,#10043,.F.);
#13669=ORIENTED_EDGE('',*,*,#10044,.T.);
#13670=ORIENTED_EDGE('',*,*,#9892,.T.);
#13671=ORIENTED_EDGE('',*,*,#10042,.T.);
#13672=ORIENTED_EDGE('',*,*,#9893,.T.);
#13673=ORIENTED_EDGE('',*,*,#10044,.F.);
#13674=ORIENTED_EDGE('',*,*,#10043,.T.);
#13675=ORIENTED_EDGE('',*,*,#10045,.T.);
#13676=ORIENTED_EDGE('',*,*,#10046,.T.);
#13677=ORIENTED_EDGE('',*,*,#10047,.T.);
#13678=ORIENTED_EDGE('',*,*,#10048,.T.);
#13679=ORIENTED_EDGE('',*,*,#10045,.F.);
#13680=ORIENTED_EDGE('',*,*,#10049,.F.);
#13681=ORIENTED_EDGE('',*,*,#10050,.F.);
#13682=ORIENTED_EDGE('',*,*,#10051,.T.);
#13683=ORIENTED_EDGE('',*,*,#10052,.F.);
#13684=ORIENTED_EDGE('',*,*,#10053,.T.);
#13685=ORIENTED_EDGE('',*,*,#10054,.F.);
#13686=ORIENTED_EDGE('',*,*,#10055,.F.);
#13687=ORIENTED_EDGE('',*,*,#10048,.F.);
#13688=ORIENTED_EDGE('',*,*,#10056,.F.);
#13689=ORIENTED_EDGE('',*,*,#10057,.F.);
#13690=ORIENTED_EDGE('',*,*,#10049,.T.);
#13691=ORIENTED_EDGE('',*,*,#10050,.T.);
#13692=ORIENTED_EDGE('',*,*,#10057,.T.);
#13693=ORIENTED_EDGE('',*,*,#10058,.T.);
#13694=ORIENTED_EDGE('',*,*,#10059,.T.);
#13695=ORIENTED_EDGE('',*,*,#10060,.T.);
#13696=ORIENTED_EDGE('',*,*,#10061,.T.);
#13697=ORIENTED_EDGE('',*,*,#10054,.T.);
#13698=ORIENTED_EDGE('',*,*,#10062,.T.);
#13699=ORIENTED_EDGE('',*,*,#10062,.F.);
#13700=ORIENTED_EDGE('',*,*,#10053,.F.);
#13701=ORIENTED_EDGE('',*,*,#10063,.F.);
#13702=ORIENTED_EDGE('',*,*,#10064,.T.);
#13703=ORIENTED_EDGE('',*,*,#10065,.T.);
#13704=ORIENTED_EDGE('',*,*,#10063,.T.);
#13705=ORIENTED_EDGE('',*,*,#10052,.T.);
#13706=ORIENTED_EDGE('',*,*,#10066,.T.);
#13707=ORIENTED_EDGE('',*,*,#10047,.F.);
#13708=ORIENTED_EDGE('',*,*,#10067,.F.);
#13709=ORIENTED_EDGE('',*,*,#10060,.F.);
#13710=ORIENTED_EDGE('',*,*,#10064,.F.);
#13711=ORIENTED_EDGE('',*,*,#10065,.F.);
#13712=ORIENTED_EDGE('',*,*,#10068,.T.);
#13713=ORIENTED_EDGE('',*,*,#10058,.F.);
#13714=ORIENTED_EDGE('',*,*,#10056,.T.);
#13715=ORIENTED_EDGE('',*,*,#10046,.F.);
#13716=ORIENTED_EDGE('',*,*,#10055,.T.);
#13717=ORIENTED_EDGE('',*,*,#10061,.F.);
#13718=ORIENTED_EDGE('',*,*,#10067,.T.);
#13719=ORIENTED_EDGE('',*,*,#10059,.F.);
#13720=ORIENTED_EDGE('',*,*,#10068,.F.);
#13721=ORIENTED_EDGE('',*,*,#10066,.F.);
#13722=ORIENTED_EDGE('',*,*,#10051,.F.);
#13723=ORIENTED_EDGE('',*,*,#10069,.F.);
#13724=ORIENTED_EDGE('',*,*,#10070,.T.);
#13725=ORIENTED_EDGE('',*,*,#10071,.T.);
#13726=ORIENTED_EDGE('',*,*,#10070,.F.);
#13727=ORIENTED_EDGE('',*,*,#10072,.F.);
#13728=ORIENTED_EDGE('',*,*,#10073,.T.);
#13729=ORIENTED_EDGE('',*,*,#10069,.T.);
#13730=ORIENTED_EDGE('',*,*,#10073,.F.);
#13731=ORIENTED_EDGE('',*,*,#10074,.F.);
#13732=ORIENTED_EDGE('',*,*,#10075,.T.);
#13733=ORIENTED_EDGE('',*,*,#10072,.T.);
#13734=ORIENTED_EDGE('',*,*,#10075,.F.);
#13735=ORIENTED_EDGE('',*,*,#10074,.T.);
#13736=ORIENTED_EDGE('',*,*,#10076,.F.);
#13737=ORIENTED_EDGE('',*,*,#10076,.T.);
#13738=ORIENTED_EDGE('',*,*,#10077,.T.);
#13739=ORIENTED_EDGE('',*,*,#10078,.F.);
#13740=ORIENTED_EDGE('',*,*,#10077,.F.);
#13741=ORIENTED_EDGE('',*,*,#10078,.T.);
#13742=ORIENTED_EDGE('',*,*,#10079,.T.);
#13743=ORIENTED_EDGE('',*,*,#10080,.F.);
#13744=ORIENTED_EDGE('',*,*,#10079,.F.);
#13745=ORIENTED_EDGE('',*,*,#10080,.T.);
#13746=ORIENTED_EDGE('',*,*,#10081,.T.);
#13747=ORIENTED_EDGE('',*,*,#10082,.F.);
#13748=ORIENTED_EDGE('',*,*,#10081,.F.);
#13749=ORIENTED_EDGE('',*,*,#10071,.F.);
#13750=ORIENTED_EDGE('',*,*,#10082,.T.);
#13751=ORIENTED_EDGE('',*,*,#10083,.T.);
#13752=ORIENTED_EDGE('',*,*,#10084,.T.);
#13753=ORIENTED_EDGE('',*,*,#10085,.T.);
#13754=ORIENTED_EDGE('',*,*,#10086,.T.);
#13755=ORIENTED_EDGE('',*,*,#10084,.F.);
#13756=ORIENTED_EDGE('',*,*,#10087,.F.);
#13757=ORIENTED_EDGE('',*,*,#10088,.F.);
#13758=ORIENTED_EDGE('',*,*,#10089,.T.);
#13759=ORIENTED_EDGE('',*,*,#10090,.F.);
#13760=ORIENTED_EDGE('',*,*,#10091,.T.);
#13761=ORIENTED_EDGE('',*,*,#10092,.T.);
#13762=ORIENTED_EDGE('',*,*,#10093,.T.);
#13763=ORIENTED_EDGE('',*,*,#10088,.T.);
#13764=ORIENTED_EDGE('',*,*,#10094,.F.);
#13765=ORIENTED_EDGE('',*,*,#10092,.F.);
#13766=ORIENTED_EDGE('',*,*,#10095,.F.);
#13767=ORIENTED_EDGE('',*,*,#10096,.F.);
#13768=ORIENTED_EDGE('',*,*,#10097,.F.);
#13769=ORIENTED_EDGE('',*,*,#10098,.F.);
#13770=ORIENTED_EDGE('',*,*,#10099,.F.);
#13771=ORIENTED_EDGE('',*,*,#10100,.T.);
#13772=ORIENTED_EDGE('',*,*,#10101,.T.);
#13773=ORIENTED_EDGE('',*,*,#10102,.T.);
#13774=ORIENTED_EDGE('',*,*,#10103,.T.);
#13775=ORIENTED_EDGE('',*,*,#10104,.T.);
#13776=ORIENTED_EDGE('',*,*,#10105,.T.);
#13777=ORIENTED_EDGE('',*,*,#10106,.T.);
#13778=ORIENTED_EDGE('',*,*,#10107,.T.);
#13779=ORIENTED_EDGE('',*,*,#10108,.T.);
#13780=ORIENTED_EDGE('',*,*,#10109,.T.);
#13781=ORIENTED_EDGE('',*,*,#10110,.T.);
#13782=ORIENTED_EDGE('',*,*,#10111,.T.);
#13783=ORIENTED_EDGE('',*,*,#10112,.T.);
#13784=ORIENTED_EDGE('',*,*,#10113,.T.);
#13785=ORIENTED_EDGE('',*,*,#10114,.T.);
#13786=ORIENTED_EDGE('',*,*,#10115,.T.);
#13787=ORIENTED_EDGE('',*,*,#10116,.T.);
#13788=ORIENTED_EDGE('',*,*,#10117,.T.);
#13789=ORIENTED_EDGE('',*,*,#10118,.T.);
#13790=ORIENTED_EDGE('',*,*,#10119,.T.);
#13791=ORIENTED_EDGE('',*,*,#10120,.T.);
#13792=ORIENTED_EDGE('',*,*,#10121,.T.);
#13793=ORIENTED_EDGE('',*,*,#10122,.T.);
#13794=ORIENTED_EDGE('',*,*,#10123,.T.);
#13795=ORIENTED_EDGE('',*,*,#10124,.T.);
#13796=ORIENTED_EDGE('',*,*,#10125,.T.);
#13797=ORIENTED_EDGE('',*,*,#10126,.T.);
#13798=ORIENTED_EDGE('',*,*,#10127,.T.);
#13799=ORIENTED_EDGE('',*,*,#10128,.T.);
#13800=ORIENTED_EDGE('',*,*,#10129,.T.);
#13801=ORIENTED_EDGE('',*,*,#10130,.T.);
#13802=ORIENTED_EDGE('',*,*,#10131,.T.);
#13803=ORIENTED_EDGE('',*,*,#10132,.T.);
#13804=ORIENTED_EDGE('',*,*,#10133,.T.);
#13805=ORIENTED_EDGE('',*,*,#10134,.T.);
#13806=ORIENTED_EDGE('',*,*,#10135,.T.);
#13807=ORIENTED_EDGE('',*,*,#10136,.T.);
#13808=ORIENTED_EDGE('',*,*,#10137,.T.);
#13809=ORIENTED_EDGE('',*,*,#10138,.T.);
#13810=ORIENTED_EDGE('',*,*,#10139,.T.);
#13811=ORIENTED_EDGE('',*,*,#10140,.T.);
#13812=ORIENTED_EDGE('',*,*,#10141,.T.);
#13813=ORIENTED_EDGE('',*,*,#10142,.T.);
#13814=ORIENTED_EDGE('',*,*,#10143,.T.);
#13815=ORIENTED_EDGE('',*,*,#10144,.T.);
#13816=ORIENTED_EDGE('',*,*,#10145,.T.);
#13817=ORIENTED_EDGE('',*,*,#10146,.T.);
#13818=ORIENTED_EDGE('',*,*,#10147,.T.);
#13819=ORIENTED_EDGE('',*,*,#10148,.T.);
#13820=ORIENTED_EDGE('',*,*,#10149,.T.);
#13821=ORIENTED_EDGE('',*,*,#10150,.T.);
#13822=ORIENTED_EDGE('',*,*,#10151,.T.);
#13823=ORIENTED_EDGE('',*,*,#10152,.T.);
#13824=ORIENTED_EDGE('',*,*,#10153,.T.);
#13825=ORIENTED_EDGE('',*,*,#10154,.T.);
#13826=ORIENTED_EDGE('',*,*,#10155,.T.);
#13827=ORIENTED_EDGE('',*,*,#10156,.T.);
#13828=ORIENTED_EDGE('',*,*,#10157,.T.);
#13829=ORIENTED_EDGE('',*,*,#10158,.T.);
#13830=ORIENTED_EDGE('',*,*,#10159,.T.);
#13831=ORIENTED_EDGE('',*,*,#10160,.T.);
#13832=ORIENTED_EDGE('',*,*,#10161,.T.);
#13833=ORIENTED_EDGE('',*,*,#10162,.T.);
#13834=ORIENTED_EDGE('',*,*,#10163,.T.);
#13835=ORIENTED_EDGE('',*,*,#10164,.T.);
#13836=ORIENTED_EDGE('',*,*,#10165,.T.);
#13837=ORIENTED_EDGE('',*,*,#10166,.T.);
#13838=ORIENTED_EDGE('',*,*,#10167,.T.);
#13839=ORIENTED_EDGE('',*,*,#10168,.T.);
#13840=ORIENTED_EDGE('',*,*,#10169,.T.);
#13841=ORIENTED_EDGE('',*,*,#10170,.T.);
#13842=ORIENTED_EDGE('',*,*,#10171,.T.);
#13843=ORIENTED_EDGE('',*,*,#10172,.T.);
#13844=ORIENTED_EDGE('',*,*,#10173,.T.);
#13845=ORIENTED_EDGE('',*,*,#10174,.T.);
#13846=ORIENTED_EDGE('',*,*,#10175,.T.);
#13847=ORIENTED_EDGE('',*,*,#10176,.T.);
#13848=ORIENTED_EDGE('',*,*,#10177,.T.);
#13849=ORIENTED_EDGE('',*,*,#10178,.T.);
#13850=ORIENTED_EDGE('',*,*,#10179,.T.);
#13851=ORIENTED_EDGE('',*,*,#10180,.T.);
#13852=ORIENTED_EDGE('',*,*,#10181,.T.);
#13853=ORIENTED_EDGE('',*,*,#10182,.T.);
#13854=ORIENTED_EDGE('',*,*,#10183,.T.);
#13855=ORIENTED_EDGE('',*,*,#10184,.F.);
#13856=ORIENTED_EDGE('',*,*,#10096,.T.);
#13857=ORIENTED_EDGE('',*,*,#10185,.T.);
#13858=ORIENTED_EDGE('',*,*,#10186,.T.);
#13859=ORIENTED_EDGE('',*,*,#10187,.T.);
#13860=ORIENTED_EDGE('',*,*,#10188,.T.);
#13861=ORIENTED_EDGE('',*,*,#10189,.T.);
#13862=ORIENTED_EDGE('',*,*,#10190,.T.);
#13863=ORIENTED_EDGE('',*,*,#10186,.F.);
#13864=ORIENTED_EDGE('',*,*,#10191,.T.);
#13865=ORIENTED_EDGE('',*,*,#10192,.T.);
#13866=ORIENTED_EDGE('',*,*,#10193,.T.);
#13867=ORIENTED_EDGE('',*,*,#10192,.F.);
#13868=ORIENTED_EDGE('',*,*,#10194,.T.);
#13869=ORIENTED_EDGE('',*,*,#10195,.T.);
#13870=ORIENTED_EDGE('',*,*,#10196,.T.);
#13871=ORIENTED_EDGE('',*,*,#10197,.F.);
#13872=ORIENTED_EDGE('',*,*,#10198,.T.);
#13873=ORIENTED_EDGE('',*,*,#10188,.F.);
#13874=ORIENTED_EDGE('',*,*,#10199,.T.);
#13875=ORIENTED_EDGE('',*,*,#10197,.T.);
#13876=ORIENTED_EDGE('',*,*,#10189,.F.);
#13877=ORIENTED_EDGE('',*,*,#10198,.F.);
#13878=ORIENTED_EDGE('',*,*,#10196,.F.);
#13879=ORIENTED_EDGE('',*,*,#10200,.F.);
#13880=ORIENTED_EDGE('',*,*,#10085,.F.);
#13881=ORIENTED_EDGE('',*,*,#10089,.F.);
#13882=ORIENTED_EDGE('',*,*,#10093,.F.);
#13883=ORIENTED_EDGE('',*,*,#10094,.T.);
#13884=ORIENTED_EDGE('',*,*,#10200,.T.);
#13885=ORIENTED_EDGE('',*,*,#10195,.F.);
#13886=ORIENTED_EDGE('',*,*,#10201,.T.);
#13887=ORIENTED_EDGE('',*,*,#10086,.F.);
#13888=ORIENTED_EDGE('',*,*,#10202,.F.);
#13889=ORIENTED_EDGE('',*,*,#10203,.F.);
#13890=ORIENTED_EDGE('',*,*,#10204,.T.);
#13891=ORIENTED_EDGE('',*,*,#10205,.T.);
#13892=ORIENTED_EDGE('',*,*,#10206,.T.);
#13893=ORIENTED_EDGE('',*,*,#10207,.T.);
#13894=ORIENTED_EDGE('',*,*,#10208,.T.);
#13895=ORIENTED_EDGE('',*,*,#10209,.T.);
#13896=ORIENTED_EDGE('',*,*,#10210,.T.);
#13897=ORIENTED_EDGE('',*,*,#10211,.T.);
#13898=ORIENTED_EDGE('',*,*,#10212,.T.);
#13899=ORIENTED_EDGE('',*,*,#10213,.T.);
#13900=ORIENTED_EDGE('',*,*,#10214,.T.);
#13901=ORIENTED_EDGE('',*,*,#10215,.T.);
#13902=ORIENTED_EDGE('',*,*,#10216,.T.);
#13903=ORIENTED_EDGE('',*,*,#10217,.T.);
#13904=ORIENTED_EDGE('',*,*,#10218,.T.);
#13905=ORIENTED_EDGE('',*,*,#10219,.T.);
#13906=ORIENTED_EDGE('',*,*,#10220,.T.);
#13907=ORIENTED_EDGE('',*,*,#10221,.T.);
#13908=ORIENTED_EDGE('',*,*,#10222,.T.);
#13909=ORIENTED_EDGE('',*,*,#10223,.T.);
#13910=ORIENTED_EDGE('',*,*,#10224,.T.);
#13911=ORIENTED_EDGE('',*,*,#10225,.T.);
#13912=ORIENTED_EDGE('',*,*,#10226,.T.);
#13913=ORIENTED_EDGE('',*,*,#10227,.T.);
#13914=ORIENTED_EDGE('',*,*,#10228,.T.);
#13915=ORIENTED_EDGE('',*,*,#10229,.T.);
#13916=ORIENTED_EDGE('',*,*,#10230,.T.);
#13917=ORIENTED_EDGE('',*,*,#10231,.T.);
#13918=ORIENTED_EDGE('',*,*,#10232,.T.);
#13919=ORIENTED_EDGE('',*,*,#10233,.T.);
#13920=ORIENTED_EDGE('',*,*,#10234,.T.);
#13921=ORIENTED_EDGE('',*,*,#10235,.T.);
#13922=ORIENTED_EDGE('',*,*,#10236,.T.);
#13923=ORIENTED_EDGE('',*,*,#10237,.T.);
#13924=ORIENTED_EDGE('',*,*,#10238,.T.);
#13925=ORIENTED_EDGE('',*,*,#10239,.T.);
#13926=ORIENTED_EDGE('',*,*,#10240,.T.);
#13927=ORIENTED_EDGE('',*,*,#10241,.T.);
#13928=ORIENTED_EDGE('',*,*,#10242,.T.);
#13929=ORIENTED_EDGE('',*,*,#10243,.T.);
#13930=ORIENTED_EDGE('',*,*,#10244,.T.);
#13931=ORIENTED_EDGE('',*,*,#10245,.T.);
#13932=ORIENTED_EDGE('',*,*,#10246,.T.);
#13933=ORIENTED_EDGE('',*,*,#10247,.T.);
#13934=ORIENTED_EDGE('',*,*,#10248,.T.);
#13935=ORIENTED_EDGE('',*,*,#10249,.T.);
#13936=ORIENTED_EDGE('',*,*,#10250,.T.);
#13937=ORIENTED_EDGE('',*,*,#10251,.T.);
#13938=ORIENTED_EDGE('',*,*,#10252,.T.);
#13939=ORIENTED_EDGE('',*,*,#10253,.T.);
#13940=ORIENTED_EDGE('',*,*,#10254,.T.);
#13941=ORIENTED_EDGE('',*,*,#10255,.T.);
#13942=ORIENTED_EDGE('',*,*,#10256,.T.);
#13943=ORIENTED_EDGE('',*,*,#10257,.T.);
#13944=ORIENTED_EDGE('',*,*,#10258,.T.);
#13945=ORIENTED_EDGE('',*,*,#10259,.T.);
#13946=ORIENTED_EDGE('',*,*,#10260,.T.);
#13947=ORIENTED_EDGE('',*,*,#10261,.T.);
#13948=ORIENTED_EDGE('',*,*,#10262,.T.);
#13949=ORIENTED_EDGE('',*,*,#10263,.T.);
#13950=ORIENTED_EDGE('',*,*,#10264,.T.);
#13951=ORIENTED_EDGE('',*,*,#10265,.T.);
#13952=ORIENTED_EDGE('',*,*,#10266,.T.);
#13953=ORIENTED_EDGE('',*,*,#10267,.T.);
#13954=ORIENTED_EDGE('',*,*,#10268,.T.);
#13955=ORIENTED_EDGE('',*,*,#10269,.T.);
#13956=ORIENTED_EDGE('',*,*,#10270,.T.);
#13957=ORIENTED_EDGE('',*,*,#10271,.T.);
#13958=ORIENTED_EDGE('',*,*,#10272,.T.);
#13959=ORIENTED_EDGE('',*,*,#10273,.T.);
#13960=ORIENTED_EDGE('',*,*,#10274,.T.);
#13961=ORIENTED_EDGE('',*,*,#10275,.T.);
#13962=ORIENTED_EDGE('',*,*,#10276,.T.);
#13963=ORIENTED_EDGE('',*,*,#10277,.T.);
#13964=ORIENTED_EDGE('',*,*,#10278,.T.);
#13965=ORIENTED_EDGE('',*,*,#10279,.T.);
#13966=ORIENTED_EDGE('',*,*,#10280,.T.);
#13967=ORIENTED_EDGE('',*,*,#10281,.T.);
#13968=ORIENTED_EDGE('',*,*,#10282,.T.);
#13969=ORIENTED_EDGE('',*,*,#10283,.T.);
#13970=ORIENTED_EDGE('',*,*,#10284,.T.);
#13971=ORIENTED_EDGE('',*,*,#10285,.T.);
#13972=ORIENTED_EDGE('',*,*,#10286,.T.);
#13973=ORIENTED_EDGE('',*,*,#10287,.T.);
#13974=ORIENTED_EDGE('',*,*,#10288,.T.);
#13975=ORIENTED_EDGE('',*,*,#10289,.F.);
#13976=ORIENTED_EDGE('',*,*,#10187,.F.);
#13977=ORIENTED_EDGE('',*,*,#10190,.F.);
#13978=ORIENTED_EDGE('',*,*,#10193,.F.);
#13979=ORIENTED_EDGE('',*,*,#10199,.F.);
#13980=ORIENTED_EDGE('',*,*,#10097,.T.);
#13981=ORIENTED_EDGE('',*,*,#10290,.T.);
#13982=ORIENTED_EDGE('',*,*,#10291,.T.);
#13983=ORIENTED_EDGE('',*,*,#10290,.F.);
#13984=ORIENTED_EDGE('',*,*,#10291,.F.);
#13985=ORIENTED_EDGE('',*,*,#10292,.T.);
#13986=ORIENTED_EDGE('',*,*,#10293,.F.);
#13987=ORIENTED_EDGE('',*,*,#10292,.F.);
#13988=ORIENTED_EDGE('',*,*,#10202,.T.);
#13989=ORIENTED_EDGE('',*,*,#10294,.T.);
#13990=ORIENTED_EDGE('',*,*,#10293,.T.);
#13991=ORIENTED_EDGE('',*,*,#10294,.F.);
#13992=ORIENTED_EDGE('',*,*,#10184,.T.);
#13993=ORIENTED_EDGE('',*,*,#10295,.T.);
#13994=ORIENTED_EDGE('',*,*,#10296,.T.);
#13995=ORIENTED_EDGE('',*,*,#10295,.F.);
#13996=ORIENTED_EDGE('',*,*,#10296,.F.);
#13997=ORIENTED_EDGE('',*,*,#10297,.T.);
#13998=ORIENTED_EDGE('',*,*,#10298,.F.);
#13999=ORIENTED_EDGE('',*,*,#10297,.F.);
#14000=ORIENTED_EDGE('',*,*,#10289,.T.);
#14001=ORIENTED_EDGE('',*,*,#10299,.T.);
#14002=ORIENTED_EDGE('',*,*,#10298,.T.);
#14003=ORIENTED_EDGE('',*,*,#10299,.F.);
#14004=ORIENTED_EDGE('',*,*,#10098,.T.);
#14005=ORIENTED_EDGE('',*,*,#10300,.T.);
#14006=ORIENTED_EDGE('',*,*,#10301,.T.);
#14007=ORIENTED_EDGE('',*,*,#10300,.F.);
#14008=ORIENTED_EDGE('',*,*,#10301,.F.);
#14009=ORIENTED_EDGE('',*,*,#10302,.T.);
#14010=ORIENTED_EDGE('',*,*,#10303,.F.);
#14011=ORIENTED_EDGE('',*,*,#10302,.F.);
#14012=ORIENTED_EDGE('',*,*,#10203,.T.);
#14013=ORIENTED_EDGE('',*,*,#10304,.T.);
#14014=ORIENTED_EDGE('',*,*,#10303,.T.);
#14015=ORIENTED_EDGE('',*,*,#10304,.F.);
#14016=ORIENTED_EDGE('',*,*,#10090,.T.);
#14017=ORIENTED_EDGE('',*,*,#10305,.T.);
#14018=ORIENTED_EDGE('',*,*,#10306,.T.);
#14019=ORIENTED_EDGE('',*,*,#10305,.F.);
#14020=ORIENTED_EDGE('',*,*,#10306,.F.);
#14021=ORIENTED_EDGE('',*,*,#10307,.T.);
#14022=ORIENTED_EDGE('',*,*,#10308,.F.);
#14023=ORIENTED_EDGE('',*,*,#10309,.F.);
#14024=ORIENTED_EDGE('',*,*,#10310,.F.);
#14025=ORIENTED_EDGE('',*,*,#10307,.F.);
#14026=ORIENTED_EDGE('',*,*,#10275,.F.);
#14027=ORIENTED_EDGE('',*,*,#10311,.T.);
#14028=ORIENTED_EDGE('',*,*,#10312,.T.);
#14029=ORIENTED_EDGE('',*,*,#10313,.F.);
#14030=ORIENTED_EDGE('',*,*,#10288,.F.);
#14031=ORIENTED_EDGE('',*,*,#10314,.T.);
#14032=ORIENTED_EDGE('',*,*,#10315,.T.);
#14033=ORIENTED_EDGE('',*,*,#10311,.F.);
#14034=ORIENTED_EDGE('',*,*,#10287,.F.);
#14035=ORIENTED_EDGE('',*,*,#10316,.T.);
#14036=ORIENTED_EDGE('',*,*,#10317,.T.);
#14037=ORIENTED_EDGE('',*,*,#10314,.F.);
#14038=ORIENTED_EDGE('',*,*,#10286,.F.);
#14039=ORIENTED_EDGE('',*,*,#10318,.T.);
#14040=ORIENTED_EDGE('',*,*,#10319,.T.);
#14041=ORIENTED_EDGE('',*,*,#10316,.F.);
#14042=ORIENTED_EDGE('',*,*,#10285,.F.);
#14043=ORIENTED_EDGE('',*,*,#10320,.T.);
#14044=ORIENTED_EDGE('',*,*,#10321,.T.);
#14045=ORIENTED_EDGE('',*,*,#10318,.F.);
#14046=ORIENTED_EDGE('',*,*,#10284,.F.);
#14047=ORIENTED_EDGE('',*,*,#10322,.T.);
#14048=ORIENTED_EDGE('',*,*,#10323,.T.);
#14049=ORIENTED_EDGE('',*,*,#10320,.F.);
#14050=ORIENTED_EDGE('',*,*,#10283,.F.);
#14051=ORIENTED_EDGE('',*,*,#10324,.T.);
#14052=ORIENTED_EDGE('',*,*,#10325,.T.);
#14053=ORIENTED_EDGE('',*,*,#10322,.F.);
#14054=ORIENTED_EDGE('',*,*,#10282,.F.);
#14055=ORIENTED_EDGE('',*,*,#10326,.T.);
#14056=ORIENTED_EDGE('',*,*,#10327,.T.);
#14057=ORIENTED_EDGE('',*,*,#10324,.F.);
#14058=ORIENTED_EDGE('',*,*,#10281,.F.);
#14059=ORIENTED_EDGE('',*,*,#10328,.T.);
#14060=ORIENTED_EDGE('',*,*,#10329,.T.);
#14061=ORIENTED_EDGE('',*,*,#10326,.F.);
#14062=ORIENTED_EDGE('',*,*,#10280,.F.);
#14063=ORIENTED_EDGE('',*,*,#10330,.T.);
#14064=ORIENTED_EDGE('',*,*,#10331,.T.);
#14065=ORIENTED_EDGE('',*,*,#10328,.F.);
#14066=ORIENTED_EDGE('',*,*,#10279,.F.);
#14067=ORIENTED_EDGE('',*,*,#10332,.T.);
#14068=ORIENTED_EDGE('',*,*,#10333,.T.);
#14069=ORIENTED_EDGE('',*,*,#10330,.F.);
#14070=ORIENTED_EDGE('',*,*,#10278,.F.);
#14071=ORIENTED_EDGE('',*,*,#10334,.T.);
#14072=ORIENTED_EDGE('',*,*,#10335,.T.);
#14073=ORIENTED_EDGE('',*,*,#10332,.F.);
#14074=ORIENTED_EDGE('',*,*,#10277,.F.);
#14075=ORIENTED_EDGE('',*,*,#10336,.T.);
#14076=ORIENTED_EDGE('',*,*,#10337,.T.);
#14077=ORIENTED_EDGE('',*,*,#10334,.F.);
#14078=ORIENTED_EDGE('',*,*,#10276,.F.);
#14079=ORIENTED_EDGE('',*,*,#10313,.T.);
#14080=ORIENTED_EDGE('',*,*,#10338,.T.);
#14081=ORIENTED_EDGE('',*,*,#10336,.F.);
#14082=ORIENTED_EDGE('',*,*,#10338,.F.);
#14083=ORIENTED_EDGE('',*,*,#10312,.F.);
#14084=ORIENTED_EDGE('',*,*,#10315,.F.);
#14085=ORIENTED_EDGE('',*,*,#10317,.F.);
#14086=ORIENTED_EDGE('',*,*,#10319,.F.);
#14087=ORIENTED_EDGE('',*,*,#10321,.F.);
#14088=ORIENTED_EDGE('',*,*,#10323,.F.);
#14089=ORIENTED_EDGE('',*,*,#10325,.F.);
#14090=ORIENTED_EDGE('',*,*,#10327,.F.);
#14091=ORIENTED_EDGE('',*,*,#10329,.F.);
#14092=ORIENTED_EDGE('',*,*,#10331,.F.);
#14093=ORIENTED_EDGE('',*,*,#10333,.F.);
#14094=ORIENTED_EDGE('',*,*,#10335,.F.);
#14095=ORIENTED_EDGE('',*,*,#10337,.F.);
#14096=ORIENTED_EDGE('',*,*,#10261,.F.);
#14097=ORIENTED_EDGE('',*,*,#10339,.T.);
#14098=ORIENTED_EDGE('',*,*,#10340,.T.);
#14099=ORIENTED_EDGE('',*,*,#10341,.F.);
#14100=ORIENTED_EDGE('',*,*,#10274,.F.);
#14101=ORIENTED_EDGE('',*,*,#10342,.T.);
#14102=ORIENTED_EDGE('',*,*,#10343,.T.);
#14103=ORIENTED_EDGE('',*,*,#10339,.F.);
#14104=ORIENTED_EDGE('',*,*,#10273,.F.);
#14105=ORIENTED_EDGE('',*,*,#10344,.T.);
#14106=ORIENTED_EDGE('',*,*,#10345,.T.);
#14107=ORIENTED_EDGE('',*,*,#10342,.F.);
#14108=ORIENTED_EDGE('',*,*,#10272,.F.);
#14109=ORIENTED_EDGE('',*,*,#10346,.T.);
#14110=ORIENTED_EDGE('',*,*,#10347,.T.);
#14111=ORIENTED_EDGE('',*,*,#10344,.F.);
#14112=ORIENTED_EDGE('',*,*,#10271,.F.);
#14113=ORIENTED_EDGE('',*,*,#10348,.T.);
#14114=ORIENTED_EDGE('',*,*,#10349,.T.);
#14115=ORIENTED_EDGE('',*,*,#10346,.F.);
#14116=ORIENTED_EDGE('',*,*,#10270,.F.);
#14117=ORIENTED_EDGE('',*,*,#10350,.T.);
#14118=ORIENTED_EDGE('',*,*,#10351,.T.);
#14119=ORIENTED_EDGE('',*,*,#10348,.F.);
#14120=ORIENTED_EDGE('',*,*,#10269,.F.);
#14121=ORIENTED_EDGE('',*,*,#10352,.T.);
#14122=ORIENTED_EDGE('',*,*,#10353,.T.);
#14123=ORIENTED_EDGE('',*,*,#10350,.F.);
#14124=ORIENTED_EDGE('',*,*,#10268,.F.);
#14125=ORIENTED_EDGE('',*,*,#10354,.T.);
#14126=ORIENTED_EDGE('',*,*,#10355,.T.);
#14127=ORIENTED_EDGE('',*,*,#10352,.F.);
#14128=ORIENTED_EDGE('',*,*,#10267,.F.);
#14129=ORIENTED_EDGE('',*,*,#10356,.T.);
#14130=ORIENTED_EDGE('',*,*,#10357,.T.);
#14131=ORIENTED_EDGE('',*,*,#10354,.F.);
#14132=ORIENTED_EDGE('',*,*,#10266,.F.);
#14133=ORIENTED_EDGE('',*,*,#10358,.T.);
#14134=ORIENTED_EDGE('',*,*,#10359,.T.);
#14135=ORIENTED_EDGE('',*,*,#10356,.F.);
#14136=ORIENTED_EDGE('',*,*,#10265,.F.);
#14137=ORIENTED_EDGE('',*,*,#10360,.T.);
#14138=ORIENTED_EDGE('',*,*,#10361,.T.);
#14139=ORIENTED_EDGE('',*,*,#10358,.F.);
#14140=ORIENTED_EDGE('',*,*,#10264,.F.);
#14141=ORIENTED_EDGE('',*,*,#10362,.T.);
#14142=ORIENTED_EDGE('',*,*,#10363,.T.);
#14143=ORIENTED_EDGE('',*,*,#10360,.F.);
#14144=ORIENTED_EDGE('',*,*,#10263,.F.);
#14145=ORIENTED_EDGE('',*,*,#10364,.T.);
#14146=ORIENTED_EDGE('',*,*,#10365,.T.);
#14147=ORIENTED_EDGE('',*,*,#10362,.F.);
#14148=ORIENTED_EDGE('',*,*,#10262,.F.);
#14149=ORIENTED_EDGE('',*,*,#10341,.T.);
#14150=ORIENTED_EDGE('',*,*,#10366,.T.);
#14151=ORIENTED_EDGE('',*,*,#10364,.F.);
#14152=ORIENTED_EDGE('',*,*,#10366,.F.);
#14153=ORIENTED_EDGE('',*,*,#10340,.F.);
#14154=ORIENTED_EDGE('',*,*,#10343,.F.);
#14155=ORIENTED_EDGE('',*,*,#10345,.F.);
#14156=ORIENTED_EDGE('',*,*,#10347,.F.);
#14157=ORIENTED_EDGE('',*,*,#10349,.F.);
#14158=ORIENTED_EDGE('',*,*,#10351,.F.);
#14159=ORIENTED_EDGE('',*,*,#10353,.F.);
#14160=ORIENTED_EDGE('',*,*,#10355,.F.);
#14161=ORIENTED_EDGE('',*,*,#10357,.F.);
#14162=ORIENTED_EDGE('',*,*,#10359,.F.);
#14163=ORIENTED_EDGE('',*,*,#10361,.F.);
#14164=ORIENTED_EDGE('',*,*,#10363,.F.);
#14165=ORIENTED_EDGE('',*,*,#10365,.F.);
#14166=ORIENTED_EDGE('',*,*,#10247,.F.);
#14167=ORIENTED_EDGE('',*,*,#10367,.T.);
#14168=ORIENTED_EDGE('',*,*,#10368,.T.);
#14169=ORIENTED_EDGE('',*,*,#10369,.F.);
#14170=ORIENTED_EDGE('',*,*,#10260,.F.);
#14171=ORIENTED_EDGE('',*,*,#10370,.T.);
#14172=ORIENTED_EDGE('',*,*,#10371,.T.);
#14173=ORIENTED_EDGE('',*,*,#10367,.F.);
#14174=ORIENTED_EDGE('',*,*,#10259,.F.);
#14175=ORIENTED_EDGE('',*,*,#10372,.T.);
#14176=ORIENTED_EDGE('',*,*,#10373,.T.);
#14177=ORIENTED_EDGE('',*,*,#10370,.F.);
#14178=ORIENTED_EDGE('',*,*,#10258,.F.);
#14179=ORIENTED_EDGE('',*,*,#10374,.T.);
#14180=ORIENTED_EDGE('',*,*,#10375,.T.);
#14181=ORIENTED_EDGE('',*,*,#10372,.F.);
#14182=ORIENTED_EDGE('',*,*,#10257,.F.);
#14183=ORIENTED_EDGE('',*,*,#10376,.T.);
#14184=ORIENTED_EDGE('',*,*,#10377,.T.);
#14185=ORIENTED_EDGE('',*,*,#10374,.F.);
#14186=ORIENTED_EDGE('',*,*,#10256,.F.);
#14187=ORIENTED_EDGE('',*,*,#10378,.T.);
#14188=ORIENTED_EDGE('',*,*,#10379,.T.);
#14189=ORIENTED_EDGE('',*,*,#10376,.F.);
#14190=ORIENTED_EDGE('',*,*,#10255,.F.);
#14191=ORIENTED_EDGE('',*,*,#10380,.T.);
#14192=ORIENTED_EDGE('',*,*,#10381,.T.);
#14193=ORIENTED_EDGE('',*,*,#10378,.F.);
#14194=ORIENTED_EDGE('',*,*,#10254,.F.);
#14195=ORIENTED_EDGE('',*,*,#10382,.T.);
#14196=ORIENTED_EDGE('',*,*,#10383,.T.);
#14197=ORIENTED_EDGE('',*,*,#10380,.F.);
#14198=ORIENTED_EDGE('',*,*,#10253,.F.);
#14199=ORIENTED_EDGE('',*,*,#10384,.T.);
#14200=ORIENTED_EDGE('',*,*,#10385,.T.);
#14201=ORIENTED_EDGE('',*,*,#10382,.F.);
#14202=ORIENTED_EDGE('',*,*,#10252,.F.);
#14203=ORIENTED_EDGE('',*,*,#10386,.T.);
#14204=ORIENTED_EDGE('',*,*,#10387,.T.);
#14205=ORIENTED_EDGE('',*,*,#10384,.F.);
#14206=ORIENTED_EDGE('',*,*,#10251,.F.);
#14207=ORIENTED_EDGE('',*,*,#10388,.T.);
#14208=ORIENTED_EDGE('',*,*,#10389,.T.);
#14209=ORIENTED_EDGE('',*,*,#10386,.F.);
#14210=ORIENTED_EDGE('',*,*,#10250,.F.);
#14211=ORIENTED_EDGE('',*,*,#10390,.T.);
#14212=ORIENTED_EDGE('',*,*,#10391,.T.);
#14213=ORIENTED_EDGE('',*,*,#10388,.F.);
#14214=ORIENTED_EDGE('',*,*,#10249,.F.);
#14215=ORIENTED_EDGE('',*,*,#10392,.T.);
#14216=ORIENTED_EDGE('',*,*,#10393,.T.);
#14217=ORIENTED_EDGE('',*,*,#10390,.F.);
#14218=ORIENTED_EDGE('',*,*,#10248,.F.);
#14219=ORIENTED_EDGE('',*,*,#10369,.T.);
#14220=ORIENTED_EDGE('',*,*,#10394,.T.);
#14221=ORIENTED_EDGE('',*,*,#10392,.F.);
#14222=ORIENTED_EDGE('',*,*,#10394,.F.);
#14223=ORIENTED_EDGE('',*,*,#10368,.F.);
#14224=ORIENTED_EDGE('',*,*,#10371,.F.);
#14225=ORIENTED_EDGE('',*,*,#10373,.F.);
#14226=ORIENTED_EDGE('',*,*,#10375,.F.);
#14227=ORIENTED_EDGE('',*,*,#10377,.F.);
#14228=ORIENTED_EDGE('',*,*,#10379,.F.);
#14229=ORIENTED_EDGE('',*,*,#10381,.F.);
#14230=ORIENTED_EDGE('',*,*,#10383,.F.);
#14231=ORIENTED_EDGE('',*,*,#10385,.F.);
#14232=ORIENTED_EDGE('',*,*,#10387,.F.);
#14233=ORIENTED_EDGE('',*,*,#10389,.F.);
#14234=ORIENTED_EDGE('',*,*,#10391,.F.);
#14235=ORIENTED_EDGE('',*,*,#10393,.F.);
#14236=ORIENTED_EDGE('',*,*,#10233,.F.);
#14237=ORIENTED_EDGE('',*,*,#10395,.T.);
#14238=ORIENTED_EDGE('',*,*,#10396,.T.);
#14239=ORIENTED_EDGE('',*,*,#10397,.F.);
#14240=ORIENTED_EDGE('',*,*,#10246,.F.);
#14241=ORIENTED_EDGE('',*,*,#10398,.T.);
#14242=ORIENTED_EDGE('',*,*,#10399,.T.);
#14243=ORIENTED_EDGE('',*,*,#10395,.F.);
#14244=ORIENTED_EDGE('',*,*,#10245,.F.);
#14245=ORIENTED_EDGE('',*,*,#10400,.T.);
#14246=ORIENTED_EDGE('',*,*,#10401,.T.);
#14247=ORIENTED_EDGE('',*,*,#10398,.F.);
#14248=ORIENTED_EDGE('',*,*,#10244,.F.);
#14249=ORIENTED_EDGE('',*,*,#10402,.T.);
#14250=ORIENTED_EDGE('',*,*,#10403,.T.);
#14251=ORIENTED_EDGE('',*,*,#10400,.F.);
#14252=ORIENTED_EDGE('',*,*,#10243,.F.);
#14253=ORIENTED_EDGE('',*,*,#10404,.T.);
#14254=ORIENTED_EDGE('',*,*,#10405,.T.);
#14255=ORIENTED_EDGE('',*,*,#10402,.F.);
#14256=ORIENTED_EDGE('',*,*,#10242,.F.);
#14257=ORIENTED_EDGE('',*,*,#10406,.T.);
#14258=ORIENTED_EDGE('',*,*,#10407,.T.);
#14259=ORIENTED_EDGE('',*,*,#10404,.F.);
#14260=ORIENTED_EDGE('',*,*,#10241,.F.);
#14261=ORIENTED_EDGE('',*,*,#10408,.T.);
#14262=ORIENTED_EDGE('',*,*,#10409,.T.);
#14263=ORIENTED_EDGE('',*,*,#10406,.F.);
#14264=ORIENTED_EDGE('',*,*,#10240,.F.);
#14265=ORIENTED_EDGE('',*,*,#10410,.T.);
#14266=ORIENTED_EDGE('',*,*,#10411,.T.);
#14267=ORIENTED_EDGE('',*,*,#10408,.F.);
#14268=ORIENTED_EDGE('',*,*,#10239,.F.);
#14269=ORIENTED_EDGE('',*,*,#10412,.T.);
#14270=ORIENTED_EDGE('',*,*,#10413,.T.);
#14271=ORIENTED_EDGE('',*,*,#10410,.F.);
#14272=ORIENTED_EDGE('',*,*,#10238,.F.);
#14273=ORIENTED_EDGE('',*,*,#10414,.T.);
#14274=ORIENTED_EDGE('',*,*,#10415,.T.);
#14275=ORIENTED_EDGE('',*,*,#10412,.F.);
#14276=ORIENTED_EDGE('',*,*,#10237,.F.);
#14277=ORIENTED_EDGE('',*,*,#10416,.T.);
#14278=ORIENTED_EDGE('',*,*,#10417,.T.);
#14279=ORIENTED_EDGE('',*,*,#10414,.F.);
#14280=ORIENTED_EDGE('',*,*,#10236,.F.);
#14281=ORIENTED_EDGE('',*,*,#10418,.T.);
#14282=ORIENTED_EDGE('',*,*,#10419,.T.);
#14283=ORIENTED_EDGE('',*,*,#10416,.F.);
#14284=ORIENTED_EDGE('',*,*,#10235,.F.);
#14285=ORIENTED_EDGE('',*,*,#10420,.T.);
#14286=ORIENTED_EDGE('',*,*,#10421,.T.);
#14287=ORIENTED_EDGE('',*,*,#10418,.F.);
#14288=ORIENTED_EDGE('',*,*,#10234,.F.);
#14289=ORIENTED_EDGE('',*,*,#10397,.T.);
#14290=ORIENTED_EDGE('',*,*,#10422,.T.);
#14291=ORIENTED_EDGE('',*,*,#10420,.F.);
#14292=ORIENTED_EDGE('',*,*,#10422,.F.);
#14293=ORIENTED_EDGE('',*,*,#10396,.F.);
#14294=ORIENTED_EDGE('',*,*,#10399,.F.);
#14295=ORIENTED_EDGE('',*,*,#10401,.F.);
#14296=ORIENTED_EDGE('',*,*,#10403,.F.);
#14297=ORIENTED_EDGE('',*,*,#10405,.F.);
#14298=ORIENTED_EDGE('',*,*,#10407,.F.);
#14299=ORIENTED_EDGE('',*,*,#10409,.F.);
#14300=ORIENTED_EDGE('',*,*,#10411,.F.);
#14301=ORIENTED_EDGE('',*,*,#10413,.F.);
#14302=ORIENTED_EDGE('',*,*,#10415,.F.);
#14303=ORIENTED_EDGE('',*,*,#10417,.F.);
#14304=ORIENTED_EDGE('',*,*,#10419,.F.);
#14305=ORIENTED_EDGE('',*,*,#10421,.F.);
#14306=ORIENTED_EDGE('',*,*,#10219,.F.);
#14307=ORIENTED_EDGE('',*,*,#10423,.T.);
#14308=ORIENTED_EDGE('',*,*,#10424,.T.);
#14309=ORIENTED_EDGE('',*,*,#10425,.F.);
#14310=ORIENTED_EDGE('',*,*,#10232,.F.);
#14311=ORIENTED_EDGE('',*,*,#10426,.T.);
#14312=ORIENTED_EDGE('',*,*,#10427,.T.);
#14313=ORIENTED_EDGE('',*,*,#10423,.F.);
#14314=ORIENTED_EDGE('',*,*,#10231,.F.);
#14315=ORIENTED_EDGE('',*,*,#10428,.T.);
#14316=ORIENTED_EDGE('',*,*,#10429,.T.);
#14317=ORIENTED_EDGE('',*,*,#10426,.F.);
#14318=ORIENTED_EDGE('',*,*,#10230,.F.);
#14319=ORIENTED_EDGE('',*,*,#10430,.T.);
#14320=ORIENTED_EDGE('',*,*,#10431,.T.);
#14321=ORIENTED_EDGE('',*,*,#10428,.F.);
#14322=ORIENTED_EDGE('',*,*,#10229,.F.);
#14323=ORIENTED_EDGE('',*,*,#10432,.T.);
#14324=ORIENTED_EDGE('',*,*,#10433,.T.);
#14325=ORIENTED_EDGE('',*,*,#10430,.F.);
#14326=ORIENTED_EDGE('',*,*,#10228,.F.);
#14327=ORIENTED_EDGE('',*,*,#10434,.T.);
#14328=ORIENTED_EDGE('',*,*,#10435,.T.);
#14329=ORIENTED_EDGE('',*,*,#10432,.F.);
#14330=ORIENTED_EDGE('',*,*,#10227,.F.);
#14331=ORIENTED_EDGE('',*,*,#10436,.T.);
#14332=ORIENTED_EDGE('',*,*,#10437,.T.);
#14333=ORIENTED_EDGE('',*,*,#10434,.F.);
#14334=ORIENTED_EDGE('',*,*,#10226,.F.);
#14335=ORIENTED_EDGE('',*,*,#10438,.T.);
#14336=ORIENTED_EDGE('',*,*,#10439,.T.);
#14337=ORIENTED_EDGE('',*,*,#10436,.F.);
#14338=ORIENTED_EDGE('',*,*,#10225,.F.);
#14339=ORIENTED_EDGE('',*,*,#10440,.T.);
#14340=ORIENTED_EDGE('',*,*,#10441,.T.);
#14341=ORIENTED_EDGE('',*,*,#10438,.F.);
#14342=ORIENTED_EDGE('',*,*,#10224,.F.);
#14343=ORIENTED_EDGE('',*,*,#10442,.T.);
#14344=ORIENTED_EDGE('',*,*,#10443,.T.);
#14345=ORIENTED_EDGE('',*,*,#10440,.F.);
#14346=ORIENTED_EDGE('',*,*,#10223,.F.);
#14347=ORIENTED_EDGE('',*,*,#10444,.T.);
#14348=ORIENTED_EDGE('',*,*,#10445,.T.);
#14349=ORIENTED_EDGE('',*,*,#10442,.F.);
#14350=ORIENTED_EDGE('',*,*,#10222,.F.);
#14351=ORIENTED_EDGE('',*,*,#10446,.T.);
#14352=ORIENTED_EDGE('',*,*,#10447,.T.);
#14353=ORIENTED_EDGE('',*,*,#10444,.F.);
#14354=ORIENTED_EDGE('',*,*,#10221,.F.);
#14355=ORIENTED_EDGE('',*,*,#10448,.T.);
#14356=ORIENTED_EDGE('',*,*,#10449,.T.);
#14357=ORIENTED_EDGE('',*,*,#10446,.F.);
#14358=ORIENTED_EDGE('',*,*,#10220,.F.);
#14359=ORIENTED_EDGE('',*,*,#10425,.T.);
#14360=ORIENTED_EDGE('',*,*,#10450,.T.);
#14361=ORIENTED_EDGE('',*,*,#10448,.F.);
#14362=ORIENTED_EDGE('',*,*,#10450,.F.);
#14363=ORIENTED_EDGE('',*,*,#10424,.F.);
#14364=ORIENTED_EDGE('',*,*,#10427,.F.);
#14365=ORIENTED_EDGE('',*,*,#10429,.F.);
#14366=ORIENTED_EDGE('',*,*,#10431,.F.);
#14367=ORIENTED_EDGE('',*,*,#10433,.F.);
#14368=ORIENTED_EDGE('',*,*,#10435,.F.);
#14369=ORIENTED_EDGE('',*,*,#10437,.F.);
#14370=ORIENTED_EDGE('',*,*,#10439,.F.);
#14371=ORIENTED_EDGE('',*,*,#10441,.F.);
#14372=ORIENTED_EDGE('',*,*,#10443,.F.);
#14373=ORIENTED_EDGE('',*,*,#10445,.F.);
#14374=ORIENTED_EDGE('',*,*,#10447,.F.);
#14375=ORIENTED_EDGE('',*,*,#10449,.F.);
#14376=ORIENTED_EDGE('',*,*,#10205,.F.);
#14377=ORIENTED_EDGE('',*,*,#10451,.T.);
#14378=ORIENTED_EDGE('',*,*,#10452,.T.);
#14379=ORIENTED_EDGE('',*,*,#10453,.F.);
#14380=ORIENTED_EDGE('',*,*,#10218,.F.);
#14381=ORIENTED_EDGE('',*,*,#10454,.T.);
#14382=ORIENTED_EDGE('',*,*,#10455,.T.);
#14383=ORIENTED_EDGE('',*,*,#10451,.F.);
#14384=ORIENTED_EDGE('',*,*,#10217,.F.);
#14385=ORIENTED_EDGE('',*,*,#10456,.T.);
#14386=ORIENTED_EDGE('',*,*,#10457,.T.);
#14387=ORIENTED_EDGE('',*,*,#10454,.F.);
#14388=ORIENTED_EDGE('',*,*,#10216,.F.);
#14389=ORIENTED_EDGE('',*,*,#10458,.T.);
#14390=ORIENTED_EDGE('',*,*,#10459,.T.);
#14391=ORIENTED_EDGE('',*,*,#10456,.F.);
#14392=ORIENTED_EDGE('',*,*,#10215,.F.);
#14393=ORIENTED_EDGE('',*,*,#10460,.T.);
#14394=ORIENTED_EDGE('',*,*,#10461,.T.);
#14395=ORIENTED_EDGE('',*,*,#10458,.F.);
#14396=ORIENTED_EDGE('',*,*,#10214,.F.);
#14397=ORIENTED_EDGE('',*,*,#10462,.T.);
#14398=ORIENTED_EDGE('',*,*,#10463,.T.);
#14399=ORIENTED_EDGE('',*,*,#10460,.F.);
#14400=ORIENTED_EDGE('',*,*,#10213,.F.);
#14401=ORIENTED_EDGE('',*,*,#10464,.T.);
#14402=ORIENTED_EDGE('',*,*,#10465,.T.);
#14403=ORIENTED_EDGE('',*,*,#10462,.F.);
#14404=ORIENTED_EDGE('',*,*,#10212,.F.);
#14405=ORIENTED_EDGE('',*,*,#10466,.T.);
#14406=ORIENTED_EDGE('',*,*,#10467,.T.);
#14407=ORIENTED_EDGE('',*,*,#10464,.F.);
#14408=ORIENTED_EDGE('',*,*,#10211,.F.);
#14409=ORIENTED_EDGE('',*,*,#10468,.T.);
#14410=ORIENTED_EDGE('',*,*,#10469,.T.);
#14411=ORIENTED_EDGE('',*,*,#10466,.F.);
#14412=ORIENTED_EDGE('',*,*,#10210,.F.);
#14413=ORIENTED_EDGE('',*,*,#10470,.T.);
#14414=ORIENTED_EDGE('',*,*,#10471,.T.);
#14415=ORIENTED_EDGE('',*,*,#10468,.F.);
#14416=ORIENTED_EDGE('',*,*,#10209,.F.);
#14417=ORIENTED_EDGE('',*,*,#10472,.T.);
#14418=ORIENTED_EDGE('',*,*,#10473,.T.);
#14419=ORIENTED_EDGE('',*,*,#10470,.F.);
#14420=ORIENTED_EDGE('',*,*,#10208,.F.);
#14421=ORIENTED_EDGE('',*,*,#10474,.T.);
#14422=ORIENTED_EDGE('',*,*,#10475,.T.);
#14423=ORIENTED_EDGE('',*,*,#10472,.F.);
#14424=ORIENTED_EDGE('',*,*,#10207,.F.);
#14425=ORIENTED_EDGE('',*,*,#10476,.T.);
#14426=ORIENTED_EDGE('',*,*,#10477,.T.);
#14427=ORIENTED_EDGE('',*,*,#10474,.F.);
#14428=ORIENTED_EDGE('',*,*,#10206,.F.);
#14429=ORIENTED_EDGE('',*,*,#10453,.T.);
#14430=ORIENTED_EDGE('',*,*,#10478,.T.);
#14431=ORIENTED_EDGE('',*,*,#10476,.F.);
#14432=ORIENTED_EDGE('',*,*,#10478,.F.);
#14433=ORIENTED_EDGE('',*,*,#10452,.F.);
#14434=ORIENTED_EDGE('',*,*,#10455,.F.);
#14435=ORIENTED_EDGE('',*,*,#10457,.F.);
#14436=ORIENTED_EDGE('',*,*,#10459,.F.);
#14437=ORIENTED_EDGE('',*,*,#10461,.F.);
#14438=ORIENTED_EDGE('',*,*,#10463,.F.);
#14439=ORIENTED_EDGE('',*,*,#10465,.F.);
#14440=ORIENTED_EDGE('',*,*,#10467,.F.);
#14441=ORIENTED_EDGE('',*,*,#10469,.F.);
#14442=ORIENTED_EDGE('',*,*,#10471,.F.);
#14443=ORIENTED_EDGE('',*,*,#10473,.F.);
#14444=ORIENTED_EDGE('',*,*,#10475,.F.);
#14445=ORIENTED_EDGE('',*,*,#10477,.F.);
#14446=ORIENTED_EDGE('',*,*,#10170,.F.);
#14447=ORIENTED_EDGE('',*,*,#10479,.T.);
#14448=ORIENTED_EDGE('',*,*,#10480,.T.);
#14449=ORIENTED_EDGE('',*,*,#10481,.F.);
#14450=ORIENTED_EDGE('',*,*,#10183,.F.);
#14451=ORIENTED_EDGE('',*,*,#10482,.T.);
#14452=ORIENTED_EDGE('',*,*,#10483,.T.);
#14453=ORIENTED_EDGE('',*,*,#10479,.F.);
#14454=ORIENTED_EDGE('',*,*,#10182,.F.);
#14455=ORIENTED_EDGE('',*,*,#10484,.T.);
#14456=ORIENTED_EDGE('',*,*,#10485,.T.);
#14457=ORIENTED_EDGE('',*,*,#10482,.F.);
#14458=ORIENTED_EDGE('',*,*,#10181,.F.);
#14459=ORIENTED_EDGE('',*,*,#10486,.T.);
#14460=ORIENTED_EDGE('',*,*,#10487,.T.);
#14461=ORIENTED_EDGE('',*,*,#10484,.F.);
#14462=ORIENTED_EDGE('',*,*,#10180,.F.);
#14463=ORIENTED_EDGE('',*,*,#10488,.T.);
#14464=ORIENTED_EDGE('',*,*,#10489,.T.);
#14465=ORIENTED_EDGE('',*,*,#10486,.F.);
#14466=ORIENTED_EDGE('',*,*,#10179,.F.);
#14467=ORIENTED_EDGE('',*,*,#10490,.T.);
#14468=ORIENTED_EDGE('',*,*,#10491,.T.);
#14469=ORIENTED_EDGE('',*,*,#10488,.F.);
#14470=ORIENTED_EDGE('',*,*,#10178,.F.);
#14471=ORIENTED_EDGE('',*,*,#10492,.T.);
#14472=ORIENTED_EDGE('',*,*,#10493,.T.);
#14473=ORIENTED_EDGE('',*,*,#10490,.F.);
#14474=ORIENTED_EDGE('',*,*,#10177,.F.);
#14475=ORIENTED_EDGE('',*,*,#10494,.T.);
#14476=ORIENTED_EDGE('',*,*,#10495,.T.);
#14477=ORIENTED_EDGE('',*,*,#10492,.F.);
#14478=ORIENTED_EDGE('',*,*,#10176,.F.);
#14479=ORIENTED_EDGE('',*,*,#10496,.T.);
#14480=ORIENTED_EDGE('',*,*,#10497,.T.);
#14481=ORIENTED_EDGE('',*,*,#10494,.F.);
#14482=ORIENTED_EDGE('',*,*,#10175,.F.);
#14483=ORIENTED_EDGE('',*,*,#10498,.T.);
#14484=ORIENTED_EDGE('',*,*,#10499,.T.);
#14485=ORIENTED_EDGE('',*,*,#10496,.F.);
#14486=ORIENTED_EDGE('',*,*,#10174,.F.);
#14487=ORIENTED_EDGE('',*,*,#10500,.T.);
#14488=ORIENTED_EDGE('',*,*,#10501,.T.);
#14489=ORIENTED_EDGE('',*,*,#10498,.F.);
#14490=ORIENTED_EDGE('',*,*,#10173,.F.);
#14491=ORIENTED_EDGE('',*,*,#10502,.T.);
#14492=ORIENTED_EDGE('',*,*,#10503,.T.);
#14493=ORIENTED_EDGE('',*,*,#10500,.F.);
#14494=ORIENTED_EDGE('',*,*,#10172,.F.);
#14495=ORIENTED_EDGE('',*,*,#10504,.T.);
#14496=ORIENTED_EDGE('',*,*,#10505,.T.);
#14497=ORIENTED_EDGE('',*,*,#10502,.F.);
#14498=ORIENTED_EDGE('',*,*,#10171,.F.);
#14499=ORIENTED_EDGE('',*,*,#10481,.T.);
#14500=ORIENTED_EDGE('',*,*,#10506,.T.);
#14501=ORIENTED_EDGE('',*,*,#10504,.F.);
#14502=ORIENTED_EDGE('',*,*,#10506,.F.);
#14503=ORIENTED_EDGE('',*,*,#10480,.F.);
#14504=ORIENTED_EDGE('',*,*,#10483,.F.);
#14505=ORIENTED_EDGE('',*,*,#10485,.F.);
#14506=ORIENTED_EDGE('',*,*,#10487,.F.);
#14507=ORIENTED_EDGE('',*,*,#10489,.F.);
#14508=ORIENTED_EDGE('',*,*,#10491,.F.);
#14509=ORIENTED_EDGE('',*,*,#10493,.F.);
#14510=ORIENTED_EDGE('',*,*,#10495,.F.);
#14511=ORIENTED_EDGE('',*,*,#10497,.F.);
#14512=ORIENTED_EDGE('',*,*,#10499,.F.);
#14513=ORIENTED_EDGE('',*,*,#10501,.F.);
#14514=ORIENTED_EDGE('',*,*,#10503,.F.);
#14515=ORIENTED_EDGE('',*,*,#10505,.F.);
#14516=ORIENTED_EDGE('',*,*,#10156,.F.);
#14517=ORIENTED_EDGE('',*,*,#10507,.T.);
#14518=ORIENTED_EDGE('',*,*,#10508,.T.);
#14519=ORIENTED_EDGE('',*,*,#10509,.F.);
#14520=ORIENTED_EDGE('',*,*,#10169,.F.);
#14521=ORIENTED_EDGE('',*,*,#10510,.T.);
#14522=ORIENTED_EDGE('',*,*,#10511,.T.);
#14523=ORIENTED_EDGE('',*,*,#10507,.F.);
#14524=ORIENTED_EDGE('',*,*,#10168,.F.);
#14525=ORIENTED_EDGE('',*,*,#10512,.T.);
#14526=ORIENTED_EDGE('',*,*,#10513,.T.);
#14527=ORIENTED_EDGE('',*,*,#10510,.F.);
#14528=ORIENTED_EDGE('',*,*,#10167,.F.);
#14529=ORIENTED_EDGE('',*,*,#10514,.T.);
#14530=ORIENTED_EDGE('',*,*,#10515,.T.);
#14531=ORIENTED_EDGE('',*,*,#10512,.F.);
#14532=ORIENTED_EDGE('',*,*,#10166,.F.);
#14533=ORIENTED_EDGE('',*,*,#10516,.T.);
#14534=ORIENTED_EDGE('',*,*,#10517,.T.);
#14535=ORIENTED_EDGE('',*,*,#10514,.F.);
#14536=ORIENTED_EDGE('',*,*,#10165,.F.);
#14537=ORIENTED_EDGE('',*,*,#10518,.T.);
#14538=ORIENTED_EDGE('',*,*,#10519,.T.);
#14539=ORIENTED_EDGE('',*,*,#10516,.F.);
#14540=ORIENTED_EDGE('',*,*,#10164,.F.);
#14541=ORIENTED_EDGE('',*,*,#10520,.T.);
#14542=ORIENTED_EDGE('',*,*,#10521,.T.);
#14543=ORIENTED_EDGE('',*,*,#10518,.F.);
#14544=ORIENTED_EDGE('',*,*,#10163,.F.);
#14545=ORIENTED_EDGE('',*,*,#10522,.T.);
#14546=ORIENTED_EDGE('',*,*,#10523,.T.);
#14547=ORIENTED_EDGE('',*,*,#10520,.F.);
#14548=ORIENTED_EDGE('',*,*,#10162,.F.);
#14549=ORIENTED_EDGE('',*,*,#10524,.T.);
#14550=ORIENTED_EDGE('',*,*,#10525,.T.);
#14551=ORIENTED_EDGE('',*,*,#10522,.F.);
#14552=ORIENTED_EDGE('',*,*,#10161,.F.);
#14553=ORIENTED_EDGE('',*,*,#10526,.T.);
#14554=ORIENTED_EDGE('',*,*,#10527,.T.);
#14555=ORIENTED_EDGE('',*,*,#10524,.F.);
#14556=ORIENTED_EDGE('',*,*,#10160,.F.);
#14557=ORIENTED_EDGE('',*,*,#10528,.T.);
#14558=ORIENTED_EDGE('',*,*,#10529,.T.);
#14559=ORIENTED_EDGE('',*,*,#10526,.F.);
#14560=ORIENTED_EDGE('',*,*,#10159,.F.);
#14561=ORIENTED_EDGE('',*,*,#10530,.T.);
#14562=ORIENTED_EDGE('',*,*,#10531,.T.);
#14563=ORIENTED_EDGE('',*,*,#10528,.F.);
#14564=ORIENTED_EDGE('',*,*,#10158,.F.);
#14565=ORIENTED_EDGE('',*,*,#10532,.T.);
#14566=ORIENTED_EDGE('',*,*,#10533,.T.);
#14567=ORIENTED_EDGE('',*,*,#10530,.F.);
#14568=ORIENTED_EDGE('',*,*,#10157,.F.);
#14569=ORIENTED_EDGE('',*,*,#10509,.T.);
#14570=ORIENTED_EDGE('',*,*,#10534,.T.);
#14571=ORIENTED_EDGE('',*,*,#10532,.F.);
#14572=ORIENTED_EDGE('',*,*,#10534,.F.);
#14573=ORIENTED_EDGE('',*,*,#10508,.F.);
#14574=ORIENTED_EDGE('',*,*,#10511,.F.);
#14575=ORIENTED_EDGE('',*,*,#10513,.F.);
#14576=ORIENTED_EDGE('',*,*,#10515,.F.);
#14577=ORIENTED_EDGE('',*,*,#10517,.F.);
#14578=ORIENTED_EDGE('',*,*,#10519,.F.);
#14579=ORIENTED_EDGE('',*,*,#10521,.F.);
#14580=ORIENTED_EDGE('',*,*,#10523,.F.);
#14581=ORIENTED_EDGE('',*,*,#10525,.F.);
#14582=ORIENTED_EDGE('',*,*,#10527,.F.);
#14583=ORIENTED_EDGE('',*,*,#10529,.F.);
#14584=ORIENTED_EDGE('',*,*,#10531,.F.);
#14585=ORIENTED_EDGE('',*,*,#10533,.F.);
#14586=ORIENTED_EDGE('',*,*,#10142,.F.);
#14587=ORIENTED_EDGE('',*,*,#10535,.T.);
#14588=ORIENTED_EDGE('',*,*,#10536,.T.);
#14589=ORIENTED_EDGE('',*,*,#10537,.F.);
#14590=ORIENTED_EDGE('',*,*,#10155,.F.);
#14591=ORIENTED_EDGE('',*,*,#10538,.T.);
#14592=ORIENTED_EDGE('',*,*,#10539,.T.);
#14593=ORIENTED_EDGE('',*,*,#10535,.F.);
#14594=ORIENTED_EDGE('',*,*,#10154,.F.);
#14595=ORIENTED_EDGE('',*,*,#10540,.T.);
#14596=ORIENTED_EDGE('',*,*,#10541,.T.);
#14597=ORIENTED_EDGE('',*,*,#10538,.F.);
#14598=ORIENTED_EDGE('',*,*,#10153,.F.);
#14599=ORIENTED_EDGE('',*,*,#10542,.T.);
#14600=ORIENTED_EDGE('',*,*,#10543,.T.);
#14601=ORIENTED_EDGE('',*,*,#10540,.F.);
#14602=ORIENTED_EDGE('',*,*,#10152,.F.);
#14603=ORIENTED_EDGE('',*,*,#10544,.T.);
#14604=ORIENTED_EDGE('',*,*,#10545,.T.);
#14605=ORIENTED_EDGE('',*,*,#10542,.F.);
#14606=ORIENTED_EDGE('',*,*,#10151,.F.);
#14607=ORIENTED_EDGE('',*,*,#10546,.T.);
#14608=ORIENTED_EDGE('',*,*,#10547,.T.);
#14609=ORIENTED_EDGE('',*,*,#10544,.F.);
#14610=ORIENTED_EDGE('',*,*,#10150,.F.);
#14611=ORIENTED_EDGE('',*,*,#10548,.T.);
#14612=ORIENTED_EDGE('',*,*,#10549,.T.);
#14613=ORIENTED_EDGE('',*,*,#10546,.F.);
#14614=ORIENTED_EDGE('',*,*,#10149,.F.);
#14615=ORIENTED_EDGE('',*,*,#10550,.T.);
#14616=ORIENTED_EDGE('',*,*,#10551,.T.);
#14617=ORIENTED_EDGE('',*,*,#10548,.F.);
#14618=ORIENTED_EDGE('',*,*,#10148,.F.);
#14619=ORIENTED_EDGE('',*,*,#10552,.T.);
#14620=ORIENTED_EDGE('',*,*,#10553,.T.);
#14621=ORIENTED_EDGE('',*,*,#10550,.F.);
#14622=ORIENTED_EDGE('',*,*,#10147,.F.);
#14623=ORIENTED_EDGE('',*,*,#10554,.T.);
#14624=ORIENTED_EDGE('',*,*,#10555,.T.);
#14625=ORIENTED_EDGE('',*,*,#10552,.F.);
#14626=ORIENTED_EDGE('',*,*,#10146,.F.);
#14627=ORIENTED_EDGE('',*,*,#10556,.T.);
#14628=ORIENTED_EDGE('',*,*,#10557,.T.);
#14629=ORIENTED_EDGE('',*,*,#10554,.F.);
#14630=ORIENTED_EDGE('',*,*,#10145,.F.);
#14631=ORIENTED_EDGE('',*,*,#10558,.T.);
#14632=ORIENTED_EDGE('',*,*,#10559,.T.);
#14633=ORIENTED_EDGE('',*,*,#10556,.F.);
#14634=ORIENTED_EDGE('',*,*,#10144,.F.);
#14635=ORIENTED_EDGE('',*,*,#10560,.T.);
#14636=ORIENTED_EDGE('',*,*,#10561,.T.);
#14637=ORIENTED_EDGE('',*,*,#10558,.F.);
#14638=ORIENTED_EDGE('',*,*,#10143,.F.);
#14639=ORIENTED_EDGE('',*,*,#10537,.T.);
#14640=ORIENTED_EDGE('',*,*,#10562,.T.);
#14641=ORIENTED_EDGE('',*,*,#10560,.F.);
#14642=ORIENTED_EDGE('',*,*,#10562,.F.);
#14643=ORIENTED_EDGE('',*,*,#10536,.F.);
#14644=ORIENTED_EDGE('',*,*,#10539,.F.);
#14645=ORIENTED_EDGE('',*,*,#10541,.F.);
#14646=ORIENTED_EDGE('',*,*,#10543,.F.);
#14647=ORIENTED_EDGE('',*,*,#10545,.F.);
#14648=ORIENTED_EDGE('',*,*,#10547,.F.);
#14649=ORIENTED_EDGE('',*,*,#10549,.F.);
#14650=ORIENTED_EDGE('',*,*,#10551,.F.);
#14651=ORIENTED_EDGE('',*,*,#10553,.F.);
#14652=ORIENTED_EDGE('',*,*,#10555,.F.);
#14653=ORIENTED_EDGE('',*,*,#10557,.F.);
#14654=ORIENTED_EDGE('',*,*,#10559,.F.);
#14655=ORIENTED_EDGE('',*,*,#10561,.F.);
#14656=ORIENTED_EDGE('',*,*,#10128,.F.);
#14657=ORIENTED_EDGE('',*,*,#10563,.T.);
#14658=ORIENTED_EDGE('',*,*,#10564,.T.);
#14659=ORIENTED_EDGE('',*,*,#10565,.F.);
#14660=ORIENTED_EDGE('',*,*,#10141,.F.);
#14661=ORIENTED_EDGE('',*,*,#10566,.T.);
#14662=ORIENTED_EDGE('',*,*,#10567,.T.);
#14663=ORIENTED_EDGE('',*,*,#10563,.F.);
#14664=ORIENTED_EDGE('',*,*,#10140,.F.);
#14665=ORIENTED_EDGE('',*,*,#10568,.T.);
#14666=ORIENTED_EDGE('',*,*,#10569,.T.);
#14667=ORIENTED_EDGE('',*,*,#10566,.F.);
#14668=ORIENTED_EDGE('',*,*,#10139,.F.);
#14669=ORIENTED_EDGE('',*,*,#10570,.T.);
#14670=ORIENTED_EDGE('',*,*,#10571,.T.);
#14671=ORIENTED_EDGE('',*,*,#10568,.F.);
#14672=ORIENTED_EDGE('',*,*,#10138,.F.);
#14673=ORIENTED_EDGE('',*,*,#10572,.T.);
#14674=ORIENTED_EDGE('',*,*,#10573,.T.);
#14675=ORIENTED_EDGE('',*,*,#10570,.F.);
#14676=ORIENTED_EDGE('',*,*,#10137,.F.);
#14677=ORIENTED_EDGE('',*,*,#10574,.T.);
#14678=ORIENTED_EDGE('',*,*,#10575,.T.);
#14679=ORIENTED_EDGE('',*,*,#10572,.F.);
#14680=ORIENTED_EDGE('',*,*,#10136,.F.);
#14681=ORIENTED_EDGE('',*,*,#10576,.T.);
#14682=ORIENTED_EDGE('',*,*,#10577,.T.);
#14683=ORIENTED_EDGE('',*,*,#10574,.F.);
#14684=ORIENTED_EDGE('',*,*,#10135,.F.);
#14685=ORIENTED_EDGE('',*,*,#10578,.T.);
#14686=ORIENTED_EDGE('',*,*,#10579,.T.);
#14687=ORIENTED_EDGE('',*,*,#10576,.F.);
#14688=ORIENTED_EDGE('',*,*,#10134,.F.);
#14689=ORIENTED_EDGE('',*,*,#10580,.T.);
#14690=ORIENTED_EDGE('',*,*,#10581,.T.);
#14691=ORIENTED_EDGE('',*,*,#10578,.F.);
#14692=ORIENTED_EDGE('',*,*,#10133,.F.);
#14693=ORIENTED_EDGE('',*,*,#10582,.T.);
#14694=ORIENTED_EDGE('',*,*,#10583,.T.);
#14695=ORIENTED_EDGE('',*,*,#10580,.F.);
#14696=ORIENTED_EDGE('',*,*,#10132,.F.);
#14697=ORIENTED_EDGE('',*,*,#10584,.T.);
#14698=ORIENTED_EDGE('',*,*,#10585,.T.);
#14699=ORIENTED_EDGE('',*,*,#10582,.F.);
#14700=ORIENTED_EDGE('',*,*,#10131,.F.);
#14701=ORIENTED_EDGE('',*,*,#10586,.T.);
#14702=ORIENTED_EDGE('',*,*,#10587,.T.);
#14703=ORIENTED_EDGE('',*,*,#10584,.F.);
#14704=ORIENTED_EDGE('',*,*,#10130,.F.);
#14705=ORIENTED_EDGE('',*,*,#10588,.T.);
#14706=ORIENTED_EDGE('',*,*,#10589,.T.);
#14707=ORIENTED_EDGE('',*,*,#10586,.F.);
#14708=ORIENTED_EDGE('',*,*,#10129,.F.);
#14709=ORIENTED_EDGE('',*,*,#10565,.T.);
#14710=ORIENTED_EDGE('',*,*,#10590,.T.);
#14711=ORIENTED_EDGE('',*,*,#10588,.F.);
#14712=ORIENTED_EDGE('',*,*,#10590,.F.);
#14713=ORIENTED_EDGE('',*,*,#10564,.F.);
#14714=ORIENTED_EDGE('',*,*,#10567,.F.);
#14715=ORIENTED_EDGE('',*,*,#10569,.F.);
#14716=ORIENTED_EDGE('',*,*,#10571,.F.);
#14717=ORIENTED_EDGE('',*,*,#10573,.F.);
#14718=ORIENTED_EDGE('',*,*,#10575,.F.);
#14719=ORIENTED_EDGE('',*,*,#10577,.F.);
#14720=ORIENTED_EDGE('',*,*,#10579,.F.);
#14721=ORIENTED_EDGE('',*,*,#10581,.F.);
#14722=ORIENTED_EDGE('',*,*,#10583,.F.);
#14723=ORIENTED_EDGE('',*,*,#10585,.F.);
#14724=ORIENTED_EDGE('',*,*,#10587,.F.);
#14725=ORIENTED_EDGE('',*,*,#10589,.F.);
#14726=ORIENTED_EDGE('',*,*,#10114,.F.);
#14727=ORIENTED_EDGE('',*,*,#10591,.T.);
#14728=ORIENTED_EDGE('',*,*,#10592,.T.);
#14729=ORIENTED_EDGE('',*,*,#10593,.F.);
#14730=ORIENTED_EDGE('',*,*,#10127,.F.);
#14731=ORIENTED_EDGE('',*,*,#10594,.T.);
#14732=ORIENTED_EDGE('',*,*,#10595,.T.);
#14733=ORIENTED_EDGE('',*,*,#10591,.F.);
#14734=ORIENTED_EDGE('',*,*,#10126,.F.);
#14735=ORIENTED_EDGE('',*,*,#10596,.T.);
#14736=ORIENTED_EDGE('',*,*,#10597,.T.);
#14737=ORIENTED_EDGE('',*,*,#10594,.F.);
#14738=ORIENTED_EDGE('',*,*,#10125,.F.);
#14739=ORIENTED_EDGE('',*,*,#10598,.T.);
#14740=ORIENTED_EDGE('',*,*,#10599,.T.);
#14741=ORIENTED_EDGE('',*,*,#10596,.F.);
#14742=ORIENTED_EDGE('',*,*,#10124,.F.);
#14743=ORIENTED_EDGE('',*,*,#10600,.T.);
#14744=ORIENTED_EDGE('',*,*,#10601,.T.);
#14745=ORIENTED_EDGE('',*,*,#10598,.F.);
#14746=ORIENTED_EDGE('',*,*,#10123,.F.);
#14747=ORIENTED_EDGE('',*,*,#10602,.T.);
#14748=ORIENTED_EDGE('',*,*,#10603,.T.);
#14749=ORIENTED_EDGE('',*,*,#10600,.F.);
#14750=ORIENTED_EDGE('',*,*,#10122,.F.);
#14751=ORIENTED_EDGE('',*,*,#10604,.T.);
#14752=ORIENTED_EDGE('',*,*,#10605,.T.);
#14753=ORIENTED_EDGE('',*,*,#10602,.F.);
#14754=ORIENTED_EDGE('',*,*,#10121,.F.);
#14755=ORIENTED_EDGE('',*,*,#10606,.T.);
#14756=ORIENTED_EDGE('',*,*,#10607,.T.);
#14757=ORIENTED_EDGE('',*,*,#10604,.F.);
#14758=ORIENTED_EDGE('',*,*,#10120,.F.);
#14759=ORIENTED_EDGE('',*,*,#10608,.T.);
#14760=ORIENTED_EDGE('',*,*,#10609,.T.);
#14761=ORIENTED_EDGE('',*,*,#10606,.F.);
#14762=ORIENTED_EDGE('',*,*,#10119,.F.);
#14763=ORIENTED_EDGE('',*,*,#10610,.T.);
#14764=ORIENTED_EDGE('',*,*,#10611,.T.);
#14765=ORIENTED_EDGE('',*,*,#10608,.F.);
#14766=ORIENTED_EDGE('',*,*,#10118,.F.);
#14767=ORIENTED_EDGE('',*,*,#10612,.T.);
#14768=ORIENTED_EDGE('',*,*,#10613,.T.);
#14769=ORIENTED_EDGE('',*,*,#10610,.F.);
#14770=ORIENTED_EDGE('',*,*,#10117,.F.);
#14771=ORIENTED_EDGE('',*,*,#10614,.T.);
#14772=ORIENTED_EDGE('',*,*,#10615,.T.);
#14773=ORIENTED_EDGE('',*,*,#10612,.F.);
#14774=ORIENTED_EDGE('',*,*,#10116,.F.);
#14775=ORIENTED_EDGE('',*,*,#10616,.T.);
#14776=ORIENTED_EDGE('',*,*,#10617,.T.);
#14777=ORIENTED_EDGE('',*,*,#10614,.F.);
#14778=ORIENTED_EDGE('',*,*,#10115,.F.);
#14779=ORIENTED_EDGE('',*,*,#10593,.T.);
#14780=ORIENTED_EDGE('',*,*,#10618,.T.);
#14781=ORIENTED_EDGE('',*,*,#10616,.F.);
#14782=ORIENTED_EDGE('',*,*,#10618,.F.);
#14783=ORIENTED_EDGE('',*,*,#10592,.F.);
#14784=ORIENTED_EDGE('',*,*,#10595,.F.);
#14785=ORIENTED_EDGE('',*,*,#10597,.F.);
#14786=ORIENTED_EDGE('',*,*,#10599,.F.);
#14787=ORIENTED_EDGE('',*,*,#10601,.F.);
#14788=ORIENTED_EDGE('',*,*,#10603,.F.);
#14789=ORIENTED_EDGE('',*,*,#10605,.F.);
#14790=ORIENTED_EDGE('',*,*,#10607,.F.);
#14791=ORIENTED_EDGE('',*,*,#10609,.F.);
#14792=ORIENTED_EDGE('',*,*,#10611,.F.);
#14793=ORIENTED_EDGE('',*,*,#10613,.F.);
#14794=ORIENTED_EDGE('',*,*,#10615,.F.);
#14795=ORIENTED_EDGE('',*,*,#10617,.F.);
#14796=ORIENTED_EDGE('',*,*,#10100,.F.);
#14797=ORIENTED_EDGE('',*,*,#10619,.T.);
#14798=ORIENTED_EDGE('',*,*,#10620,.T.);
#14799=ORIENTED_EDGE('',*,*,#10621,.F.);
#14800=ORIENTED_EDGE('',*,*,#10113,.F.);
#14801=ORIENTED_EDGE('',*,*,#10622,.T.);
#14802=ORIENTED_EDGE('',*,*,#10623,.T.);
#14803=ORIENTED_EDGE('',*,*,#10619,.F.);
#14804=ORIENTED_EDGE('',*,*,#10112,.F.);
#14805=ORIENTED_EDGE('',*,*,#10624,.T.);
#14806=ORIENTED_EDGE('',*,*,#10625,.T.);
#14807=ORIENTED_EDGE('',*,*,#10622,.F.);
#14808=ORIENTED_EDGE('',*,*,#10111,.F.);
#14809=ORIENTED_EDGE('',*,*,#10626,.T.);
#14810=ORIENTED_EDGE('',*,*,#10627,.T.);
#14811=ORIENTED_EDGE('',*,*,#10624,.F.);
#14812=ORIENTED_EDGE('',*,*,#10110,.F.);
#14813=ORIENTED_EDGE('',*,*,#10628,.T.);
#14814=ORIENTED_EDGE('',*,*,#10629,.T.);
#14815=ORIENTED_EDGE('',*,*,#10626,.F.);
#14816=ORIENTED_EDGE('',*,*,#10109,.F.);
#14817=ORIENTED_EDGE('',*,*,#10630,.T.);
#14818=ORIENTED_EDGE('',*,*,#10631,.T.);
#14819=ORIENTED_EDGE('',*,*,#10628,.F.);
#14820=ORIENTED_EDGE('',*,*,#10108,.F.);
#14821=ORIENTED_EDGE('',*,*,#10632,.T.);
#14822=ORIENTED_EDGE('',*,*,#10633,.T.);
#14823=ORIENTED_EDGE('',*,*,#10630,.F.);
#14824=ORIENTED_EDGE('',*,*,#10107,.F.);
#14825=ORIENTED_EDGE('',*,*,#10634,.T.);
#14826=ORIENTED_EDGE('',*,*,#10635,.T.);
#14827=ORIENTED_EDGE('',*,*,#10632,.F.);
#14828=ORIENTED_EDGE('',*,*,#10106,.F.);
#14829=ORIENTED_EDGE('',*,*,#10636,.T.);
#14830=ORIENTED_EDGE('',*,*,#10637,.T.);
#14831=ORIENTED_EDGE('',*,*,#10634,.F.);
#14832=ORIENTED_EDGE('',*,*,#10105,.F.);
#14833=ORIENTED_EDGE('',*,*,#10638,.T.);
#14834=ORIENTED_EDGE('',*,*,#10639,.T.);
#14835=ORIENTED_EDGE('',*,*,#10636,.F.);
#14836=ORIENTED_EDGE('',*,*,#10104,.F.);
#14837=ORIENTED_EDGE('',*,*,#10640,.T.);
#14838=ORIENTED_EDGE('',*,*,#10641,.T.);
#14839=ORIENTED_EDGE('',*,*,#10638,.F.);
#14840=ORIENTED_EDGE('',*,*,#10103,.F.);
#14841=ORIENTED_EDGE('',*,*,#10642,.T.);
#14842=ORIENTED_EDGE('',*,*,#10643,.T.);
#14843=ORIENTED_EDGE('',*,*,#10640,.F.);
#14844=ORIENTED_EDGE('',*,*,#10102,.F.);
#14845=ORIENTED_EDGE('',*,*,#10644,.T.);
#14846=ORIENTED_EDGE('',*,*,#10645,.T.);
#14847=ORIENTED_EDGE('',*,*,#10642,.F.);
#14848=ORIENTED_EDGE('',*,*,#10101,.F.);
#14849=ORIENTED_EDGE('',*,*,#10621,.T.);
#14850=ORIENTED_EDGE('',*,*,#10646,.T.);
#14851=ORIENTED_EDGE('',*,*,#10644,.F.);
#14852=ORIENTED_EDGE('',*,*,#10646,.F.);
#14853=ORIENTED_EDGE('',*,*,#10620,.F.);
#14854=ORIENTED_EDGE('',*,*,#10623,.F.);
#14855=ORIENTED_EDGE('',*,*,#10625,.F.);
#14856=ORIENTED_EDGE('',*,*,#10627,.F.);
#14857=ORIENTED_EDGE('',*,*,#10629,.F.);
#14858=ORIENTED_EDGE('',*,*,#10631,.F.);
#14859=ORIENTED_EDGE('',*,*,#10633,.F.);
#14860=ORIENTED_EDGE('',*,*,#10635,.F.);
#14861=ORIENTED_EDGE('',*,*,#10637,.F.);
#14862=ORIENTED_EDGE('',*,*,#10639,.F.);
#14863=ORIENTED_EDGE('',*,*,#10641,.F.);
#14864=ORIENTED_EDGE('',*,*,#10643,.F.);
#14865=ORIENTED_EDGE('',*,*,#10645,.F.);
#14866=ORIENTED_EDGE('',*,*,#10204,.F.);
#14867=ORIENTED_EDGE('',*,*,#10647,.T.);
#14868=ORIENTED_EDGE('',*,*,#10309,.T.);
#14869=ORIENTED_EDGE('',*,*,#10308,.T.);
#14870=ORIENTED_EDGE('',*,*,#10648,.T.);
#14871=ORIENTED_EDGE('',*,*,#10099,.T.);
#14872=ORIENTED_EDGE('',*,*,#10648,.F.);
#14873=ORIENTED_EDGE('',*,*,#10310,.T.);
#14874=ORIENTED_EDGE('',*,*,#10647,.F.);
#14875=ORIENTED_EDGE('',*,*,#10185,.F.);
#14876=ORIENTED_EDGE('',*,*,#10095,.T.);
#14877=ORIENTED_EDGE('',*,*,#10091,.F.);
#14878=ORIENTED_EDGE('',*,*,#10087,.T.);
#14879=ORIENTED_EDGE('',*,*,#10083,.F.);
#14880=ORIENTED_EDGE('',*,*,#10201,.F.);
#14881=ORIENTED_EDGE('',*,*,#10194,.F.);
#14882=ORIENTED_EDGE('',*,*,#10191,.F.);
#14883=ORIENTED_EDGE('',*,*,#10649,.F.);
#14884=ORIENTED_EDGE('',*,*,#10650,.T.);
#14885=ORIENTED_EDGE('',*,*,#10651,.T.);
#14886=ORIENTED_EDGE('',*,*,#10650,.F.);
#14887=ORIENTED_EDGE('',*,*,#10651,.F.);
#14888=ORIENTED_EDGE('',*,*,#10652,.F.);
#14889=ORIENTED_EDGE('',*,*,#10653,.T.);
#14890=ORIENTED_EDGE('',*,*,#10654,.T.);
#14891=ORIENTED_EDGE('',*,*,#10653,.F.);
#14892=ORIENTED_EDGE('',*,*,#10654,.F.);
#14893=ORIENTED_EDGE('',*,*,#10655,.F.);
#14894=ORIENTED_EDGE('',*,*,#10656,.T.);
#14895=ORIENTED_EDGE('',*,*,#10657,.T.);
#14896=ORIENTED_EDGE('',*,*,#10656,.F.);
#14897=ORIENTED_EDGE('',*,*,#10657,.F.);
#14898=ORIENTED_EDGE('',*,*,#10658,.F.);
#14899=ORIENTED_EDGE('',*,*,#10659,.T.);
#14900=ORIENTED_EDGE('',*,*,#10660,.T.);
#14901=ORIENTED_EDGE('',*,*,#10659,.F.);
#14902=ORIENTED_EDGE('',*,*,#10660,.F.);
#14903=ORIENTED_EDGE('',*,*,#10661,.F.);
#14904=ORIENTED_EDGE('',*,*,#10662,.T.);
#14905=ORIENTED_EDGE('',*,*,#10663,.T.);
#14906=ORIENTED_EDGE('',*,*,#10662,.F.);
#14907=ORIENTED_EDGE('',*,*,#10663,.F.);
#14908=ORIENTED_EDGE('',*,*,#10664,.F.);
#14909=ORIENTED_EDGE('',*,*,#10665,.T.);
#14910=ORIENTED_EDGE('',*,*,#10666,.T.);
#14911=ORIENTED_EDGE('',*,*,#10665,.F.);
#14912=ORIENTED_EDGE('',*,*,#10666,.F.);
#14913=ORIENTED_EDGE('',*,*,#10667,.T.);
#14914=ORIENTED_EDGE('',*,*,#10668,.T.);
#14915=ORIENTED_EDGE('',*,*,#10669,.F.);
#14916=ORIENTED_EDGE('',*,*,#10668,.F.);
#14917=ORIENTED_EDGE('',*,*,#10670,.F.);
#14918=ORIENTED_EDGE('',*,*,#10667,.F.);
#14919=ORIENTED_EDGE('',*,*,#10671,.F.);
#14920=ORIENTED_EDGE('',*,*,#10669,.T.);
#14921=ORIENTED_EDGE('',*,*,#10672,.F.);
#14922=ORIENTED_EDGE('',*,*,#10673,.T.);
#14923=ORIENTED_EDGE('',*,*,#10671,.T.);
#14924=ORIENTED_EDGE('',*,*,#10673,.F.);
#14925=ORIENTED_EDGE('',*,*,#10674,.F.);
#14926=ORIENTED_EDGE('',*,*,#10675,.T.);
#14927=ORIENTED_EDGE('',*,*,#10676,.T.);
#14928=ORIENTED_EDGE('',*,*,#10675,.F.);
#14929=ORIENTED_EDGE('',*,*,#10677,.F.);
#14930=ORIENTED_EDGE('',*,*,#10678,.T.);
#14931=ORIENTED_EDGE('',*,*,#10674,.T.);
#14932=ORIENTED_EDGE('',*,*,#10678,.F.);
#14933=ORIENTED_EDGE('',*,*,#10679,.F.);
#14934=ORIENTED_EDGE('',*,*,#10677,.T.);
#14935=ORIENTED_EDGE('',*,*,#10664,.T.);
#14936=ORIENTED_EDGE('',*,*,#10661,.T.);
#14937=ORIENTED_EDGE('',*,*,#10658,.T.);
#14938=ORIENTED_EDGE('',*,*,#10655,.T.);
#14939=ORIENTED_EDGE('',*,*,#10652,.T.);
#14940=ORIENTED_EDGE('',*,*,#10649,.T.);
#14941=ORIENTED_EDGE('',*,*,#10680,.F.);
#14942=ORIENTED_EDGE('',*,*,#10681,.T.);
#14943=ORIENTED_EDGE('',*,*,#10679,.T.);
#14944=ORIENTED_EDGE('',*,*,#10681,.F.);
#14945=ORIENTED_EDGE('',*,*,#10682,.F.);
#14946=ORIENTED_EDGE('',*,*,#10683,.T.);
#14947=ORIENTED_EDGE('',*,*,#10680,.T.);
#14948=ORIENTED_EDGE('',*,*,#10683,.F.);
#14949=ORIENTED_EDGE('',*,*,#10684,.F.);
#14950=ORIENTED_EDGE('',*,*,#10685,.T.);
#14951=ORIENTED_EDGE('',*,*,#10682,.T.);
#14952=ORIENTED_EDGE('',*,*,#10685,.F.);
#14953=ORIENTED_EDGE('',*,*,#10684,.T.);
#14954=ORIENTED_EDGE('',*,*,#10686,.F.);
#14955=ORIENTED_EDGE('',*,*,#10687,.F.);
#14956=ORIENTED_EDGE('',*,*,#10688,.T.);
#14957=ORIENTED_EDGE('',*,*,#10686,.T.);
#14958=ORIENTED_EDGE('',*,*,#10688,.F.);
#14959=ORIENTED_EDGE('',*,*,#10670,.T.);
#14960=ORIENTED_EDGE('',*,*,#10689,.T.);
#14961=ORIENTED_EDGE('',*,*,#10687,.T.);
#14962=ORIENTED_EDGE('',*,*,#10689,.F.);
#14963=ORIENTED_EDGE('',*,*,#10690,.F.);
#14964=ORIENTED_EDGE('',*,*,#10691,.T.);
#14965=ORIENTED_EDGE('',*,*,#10672,.T.);
#14966=ORIENTED_EDGE('',*,*,#10691,.F.);
#14967=ORIENTED_EDGE('',*,*,#10690,.T.);
#14968=ORIENTED_EDGE('',*,*,#10692,.F.);
#14969=ORIENTED_EDGE('',*,*,#10692,.T.);
#14970=ORIENTED_EDGE('',*,*,#10693,.T.);
#14971=ORIENTED_EDGE('',*,*,#10694,.F.);
#14972=ORIENTED_EDGE('',*,*,#10693,.F.);
#14973=ORIENTED_EDGE('',*,*,#10694,.T.);
#14974=ORIENTED_EDGE('',*,*,#10695,.T.);
#14975=ORIENTED_EDGE('',*,*,#10696,.F.);
#14976=ORIENTED_EDGE('',*,*,#10695,.F.);
#14977=ORIENTED_EDGE('',*,*,#10696,.T.);
#14978=ORIENTED_EDGE('',*,*,#10697,.T.);
#14979=ORIENTED_EDGE('',*,*,#10698,.F.);
#14980=ORIENTED_EDGE('',*,*,#10697,.F.);
#14981=ORIENTED_EDGE('',*,*,#10676,.F.);
#14982=ORIENTED_EDGE('',*,*,#10698,.T.);
#14983=ORIENTED_EDGE('',*,*,#10699,.T.);
#14984=ORIENTED_EDGE('',*,*,#10700,.T.);
#14985=ORIENTED_EDGE('',*,*,#10701,.T.);
#14986=ORIENTED_EDGE('',*,*,#10702,.T.);
#14987=ORIENTED_EDGE('',*,*,#10699,.F.);
#14988=ORIENTED_EDGE('',*,*,#10703,.F.);
#14989=ORIENTED_EDGE('',*,*,#10704,.F.);
#14990=ORIENTED_EDGE('',*,*,#10705,.T.);
#14991=ORIENTED_EDGE('',*,*,#10706,.F.);
#14992=ORIENTED_EDGE('',*,*,#10707,.T.);
#14993=ORIENTED_EDGE('',*,*,#10708,.F.);
#14994=ORIENTED_EDGE('',*,*,#10709,.F.);
#14995=ORIENTED_EDGE('',*,*,#10702,.F.);
#14996=ORIENTED_EDGE('',*,*,#10710,.F.);
#14997=ORIENTED_EDGE('',*,*,#10711,.F.);
#14998=ORIENTED_EDGE('',*,*,#10703,.T.);
#14999=ORIENTED_EDGE('',*,*,#10704,.T.);
#15000=ORIENTED_EDGE('',*,*,#10711,.T.);
#15001=ORIENTED_EDGE('',*,*,#10712,.T.);
#15002=ORIENTED_EDGE('',*,*,#10713,.T.);
#15003=ORIENTED_EDGE('',*,*,#10714,.T.);
#15004=ORIENTED_EDGE('',*,*,#10715,.T.);
#15005=ORIENTED_EDGE('',*,*,#10708,.T.);
#15006=ORIENTED_EDGE('',*,*,#10716,.T.);
#15007=ORIENTED_EDGE('',*,*,#10716,.F.);
#15008=ORIENTED_EDGE('',*,*,#10707,.F.);
#15009=ORIENTED_EDGE('',*,*,#10717,.F.);
#15010=ORIENTED_EDGE('',*,*,#10718,.T.);
#15011=ORIENTED_EDGE('',*,*,#10719,.T.);
#15012=ORIENTED_EDGE('',*,*,#10717,.T.);
#15013=ORIENTED_EDGE('',*,*,#10706,.T.);
#15014=ORIENTED_EDGE('',*,*,#10720,.T.);
#15015=ORIENTED_EDGE('',*,*,#10701,.F.);
#15016=ORIENTED_EDGE('',*,*,#10721,.F.);
#15017=ORIENTED_EDGE('',*,*,#10714,.F.);
#15018=ORIENTED_EDGE('',*,*,#10718,.F.);
#15019=ORIENTED_EDGE('',*,*,#10719,.F.);
#15020=ORIENTED_EDGE('',*,*,#10722,.T.);
#15021=ORIENTED_EDGE('',*,*,#10712,.F.);
#15022=ORIENTED_EDGE('',*,*,#10710,.T.);
#15023=ORIENTED_EDGE('',*,*,#10700,.F.);
#15024=ORIENTED_EDGE('',*,*,#10709,.T.);
#15025=ORIENTED_EDGE('',*,*,#10715,.F.);
#15026=ORIENTED_EDGE('',*,*,#10721,.T.);
#15027=ORIENTED_EDGE('',*,*,#10713,.F.);
#15028=ORIENTED_EDGE('',*,*,#10722,.F.);
#15029=ORIENTED_EDGE('',*,*,#10720,.F.);
#15030=ORIENTED_EDGE('',*,*,#10705,.F.);
#15031=ORIENTED_EDGE('',*,*,#10723,.F.);
#15032=ORIENTED_EDGE('',*,*,#10724,.T.);
#15033=ORIENTED_EDGE('',*,*,#10725,.T.);
#15034=ORIENTED_EDGE('',*,*,#10726,.T.);
#15035=ORIENTED_EDGE('',*,*,#10727,.T.);
#15036=ORIENTED_EDGE('',*,*,#10728,.T.);
#15037=ORIENTED_EDGE('',*,*,#10729,.T.);
#15038=ORIENTED_EDGE('',*,*,#10730,.T.);
#15039=ORIENTED_EDGE('',*,*,#10731,.T.);
#15040=ORIENTED_EDGE('',*,*,#10732,.T.);
#15041=ORIENTED_EDGE('',*,*,#10733,.T.);
#15042=ORIENTED_EDGE('',*,*,#10734,.T.);
#15043=ORIENTED_EDGE('',*,*,#10735,.F.);
#15044=ORIENTED_EDGE('',*,*,#10732,.F.);
#15045=ORIENTED_EDGE('',*,*,#10736,.F.);
#15046=ORIENTED_EDGE('',*,*,#10737,.T.);
#15047=ORIENTED_EDGE('',*,*,#10738,.F.);
#15048=ORIENTED_EDGE('',*,*,#10739,.T.);
#15049=ORIENTED_EDGE('',*,*,#10740,.F.);
#15050=ORIENTED_EDGE('',*,*,#10741,.F.);
#15051=ORIENTED_EDGE('',*,*,#10742,.F.);
#15052=ORIENTED_EDGE('',*,*,#10743,.T.);
#15053=ORIENTED_EDGE('',*,*,#10744,.F.);
#15054=ORIENTED_EDGE('',*,*,#10745,.T.);
#15055=ORIENTED_EDGE('',*,*,#10746,.F.);
#15056=ORIENTED_EDGE('',*,*,#10747,.F.);
#15057=ORIENTED_EDGE('',*,*,#10748,.F.);
#15058=ORIENTED_EDGE('',*,*,#10749,.T.);
#15059=ORIENTED_EDGE('',*,*,#10750,.F.);
#15060=ORIENTED_EDGE('',*,*,#10751,.T.);
#15061=ORIENTED_EDGE('',*,*,#10752,.F.);
#15062=ORIENTED_EDGE('',*,*,#10753,.F.);
#15063=ORIENTED_EDGE('',*,*,#10754,.F.);
#15064=ORIENTED_EDGE('',*,*,#10755,.T.);
#15065=ORIENTED_EDGE('',*,*,#10756,.F.);
#15066=ORIENTED_EDGE('',*,*,#10757,.T.);
#15067=ORIENTED_EDGE('',*,*,#10758,.F.);
#15068=ORIENTED_EDGE('',*,*,#10759,.F.);
#15069=ORIENTED_EDGE('',*,*,#10760,.F.);
#15070=ORIENTED_EDGE('',*,*,#10761,.T.);
#15071=ORIENTED_EDGE('',*,*,#10762,.F.);
#15072=ORIENTED_EDGE('',*,*,#10763,.T.);
#15073=ORIENTED_EDGE('',*,*,#10764,.F.);
#15074=ORIENTED_EDGE('',*,*,#10765,.F.);
#15075=ORIENTED_EDGE('',*,*,#10766,.F.);
#15076=ORIENTED_EDGE('',*,*,#10767,.T.);
#15077=ORIENTED_EDGE('',*,*,#10768,.F.);
#15078=ORIENTED_EDGE('',*,*,#10769,.T.);
#15079=ORIENTED_EDGE('',*,*,#10770,.F.);
#15080=ORIENTED_EDGE('',*,*,#10771,.F.);
#15081=ORIENTED_EDGE('',*,*,#10772,.F.);
#15082=ORIENTED_EDGE('',*,*,#10773,.T.);
#15083=ORIENTED_EDGE('',*,*,#10774,.F.);
#15084=ORIENTED_EDGE('',*,*,#10775,.T.);
#15085=ORIENTED_EDGE('',*,*,#10776,.T.);
#15086=ORIENTED_EDGE('',*,*,#10775,.F.);
#15087=ORIENTED_EDGE('',*,*,#10777,.F.);
#15088=ORIENTED_EDGE('',*,*,#10778,.T.);
#15089=ORIENTED_EDGE('',*,*,#10779,.F.);
#15090=ORIENTED_EDGE('',*,*,#10780,.F.);
#15091=ORIENTED_EDGE('',*,*,#10781,.F.);
#15092=ORIENTED_EDGE('',*,*,#10782,.T.);
#15093=ORIENTED_EDGE('',*,*,#10783,.F.);
#15094=ORIENTED_EDGE('',*,*,#10784,.T.);
#15095=ORIENTED_EDGE('',*,*,#10785,.F.);
#15096=ORIENTED_EDGE('',*,*,#10786,.F.);
#15097=ORIENTED_EDGE('',*,*,#10787,.F.);
#15098=ORIENTED_EDGE('',*,*,#10788,.T.);
#15099=ORIENTED_EDGE('',*,*,#10789,.F.);
#15100=ORIENTED_EDGE('',*,*,#10790,.T.);
#15101=ORIENTED_EDGE('',*,*,#10791,.F.);
#15102=ORIENTED_EDGE('',*,*,#10792,.F.);
#15103=ORIENTED_EDGE('',*,*,#10793,.F.);
#15104=ORIENTED_EDGE('',*,*,#10794,.T.);
#15105=ORIENTED_EDGE('',*,*,#10795,.F.);
#15106=ORIENTED_EDGE('',*,*,#10796,.T.);
#15107=ORIENTED_EDGE('',*,*,#10797,.F.);
#15108=ORIENTED_EDGE('',*,*,#10798,.F.);
#15109=ORIENTED_EDGE('',*,*,#10799,.F.);
#15110=ORIENTED_EDGE('',*,*,#10800,.T.);
#15111=ORIENTED_EDGE('',*,*,#10801,.F.);
#15112=ORIENTED_EDGE('',*,*,#10802,.T.);
#15113=ORIENTED_EDGE('',*,*,#10803,.F.);
#15114=ORIENTED_EDGE('',*,*,#10804,.F.);
#15115=ORIENTED_EDGE('',*,*,#10805,.F.);
#15116=ORIENTED_EDGE('',*,*,#10806,.T.);
#15117=ORIENTED_EDGE('',*,*,#10807,.F.);
#15118=ORIENTED_EDGE('',*,*,#10808,.T.);
#15119=ORIENTED_EDGE('',*,*,#10809,.F.);
#15120=ORIENTED_EDGE('',*,*,#10810,.F.);
#15121=ORIENTED_EDGE('',*,*,#10811,.F.);
#15122=ORIENTED_EDGE('',*,*,#10812,.T.);
#15123=ORIENTED_EDGE('',*,*,#10813,.F.);
#15124=ORIENTED_EDGE('',*,*,#10814,.T.);
#15125=ORIENTED_EDGE('',*,*,#10815,.F.);
#15126=ORIENTED_EDGE('',*,*,#10816,.F.);
#15127=ORIENTED_EDGE('',*,*,#10817,.F.);
#15128=ORIENTED_EDGE('',*,*,#10818,.T.);
#15129=ORIENTED_EDGE('',*,*,#10819,.F.);
#15130=ORIENTED_EDGE('',*,*,#10820,.T.);
#15131=ORIENTED_EDGE('',*,*,#10821,.T.);
#15132=ORIENTED_EDGE('',*,*,#10810,.T.);
#15133=ORIENTED_EDGE('',*,*,#10822,.T.);
#15134=ORIENTED_EDGE('',*,*,#10823,.T.);
#15135=ORIENTED_EDGE('',*,*,#10824,.T.);
#15136=ORIENTED_EDGE('',*,*,#10798,.T.);
#15137=ORIENTED_EDGE('',*,*,#10825,.T.);
#15138=ORIENTED_EDGE('',*,*,#10826,.T.);
#15139=ORIENTED_EDGE('',*,*,#10827,.T.);
#15140=ORIENTED_EDGE('',*,*,#10786,.T.);
#15141=ORIENTED_EDGE('',*,*,#10828,.T.);
#15142=ORIENTED_EDGE('',*,*,#10829,.T.);
#15143=ORIENTED_EDGE('',*,*,#10830,.T.);
#15144=ORIENTED_EDGE('',*,*,#10771,.T.);
#15145=ORIENTED_EDGE('',*,*,#10831,.T.);
#15146=ORIENTED_EDGE('',*,*,#10832,.T.);
#15147=ORIENTED_EDGE('',*,*,#10833,.T.);
#15148=ORIENTED_EDGE('',*,*,#10759,.T.);
#15149=ORIENTED_EDGE('',*,*,#10834,.T.);
#15150=ORIENTED_EDGE('',*,*,#10835,.T.);
#15151=ORIENTED_EDGE('',*,*,#10836,.T.);
#15152=ORIENTED_EDGE('',*,*,#10747,.T.);
#15153=ORIENTED_EDGE('',*,*,#10837,.T.);
#15154=ORIENTED_EDGE('',*,*,#10838,.T.);
#15155=ORIENTED_EDGE('',*,*,#10839,.T.);
#15156=ORIENTED_EDGE('',*,*,#10816,.T.);
#15157=ORIENTED_EDGE('',*,*,#10840,.T.);
#15158=ORIENTED_EDGE('',*,*,#10841,.T.);
#15159=ORIENTED_EDGE('',*,*,#10842,.T.);
#15160=ORIENTED_EDGE('',*,*,#10804,.T.);
#15161=ORIENTED_EDGE('',*,*,#10843,.T.);
#15162=ORIENTED_EDGE('',*,*,#10844,.T.);
#15163=ORIENTED_EDGE('',*,*,#10845,.T.);
#15164=ORIENTED_EDGE('',*,*,#10792,.T.);
#15165=ORIENTED_EDGE('',*,*,#10846,.T.);
#15166=ORIENTED_EDGE('',*,*,#10847,.T.);
#15167=ORIENTED_EDGE('',*,*,#10848,.T.);
#15168=ORIENTED_EDGE('',*,*,#10780,.T.);
#15169=ORIENTED_EDGE('',*,*,#10849,.T.);
#15170=ORIENTED_EDGE('',*,*,#10850,.T.);
#15171=ORIENTED_EDGE('',*,*,#10851,.T.);
#15172=ORIENTED_EDGE('',*,*,#10765,.T.);
#15173=ORIENTED_EDGE('',*,*,#10852,.T.);
#15174=ORIENTED_EDGE('',*,*,#10853,.T.);
#15175=ORIENTED_EDGE('',*,*,#10854,.T.);
#15176=ORIENTED_EDGE('',*,*,#10753,.T.);
#15177=ORIENTED_EDGE('',*,*,#10855,.T.);
#15178=ORIENTED_EDGE('',*,*,#10856,.T.);
#15179=ORIENTED_EDGE('',*,*,#10857,.T.);
#15180=ORIENTED_EDGE('',*,*,#10741,.T.);
#15181=ORIENTED_EDGE('',*,*,#10858,.T.);
#15182=ORIENTED_EDGE('',*,*,#10859,.T.);
#15183=ORIENTED_EDGE('',*,*,#10860,.T.);
#15184=ORIENTED_EDGE('',*,*,#10861,.T.);
#15185=ORIENTED_EDGE('',*,*,#10862,.T.);
#15186=ORIENTED_EDGE('',*,*,#10863,.T.);
#15187=ORIENTED_EDGE('',*,*,#10861,.F.);
#15188=ORIENTED_EDGE('',*,*,#10864,.F.);
#15189=ORIENTED_EDGE('',*,*,#10865,.F.);
#15190=ORIENTED_EDGE('',*,*,#10866,.T.);
#15191=ORIENTED_EDGE('',*,*,#10862,.F.);
#15192=ORIENTED_EDGE('',*,*,#10863,.F.);
#15193=ORIENTED_EDGE('',*,*,#10866,.F.);
#15194=ORIENTED_EDGE('',*,*,#10867,.F.);
#15195=ORIENTED_EDGE('',*,*,#10860,.F.);
#15196=ORIENTED_EDGE('',*,*,#10864,.T.);
#15197=ORIENTED_EDGE('',*,*,#10865,.T.);
#15198=ORIENTED_EDGE('',*,*,#10868,.T.);
#15199=ORIENTED_EDGE('',*,*,#10869,.T.);
#15200=ORIENTED_EDGE('',*,*,#10868,.F.);
#15201=ORIENTED_EDGE('',*,*,#10870,.T.);
#15202=ORIENTED_EDGE('',*,*,#10869,.F.);
#15203=ORIENTED_EDGE('',*,*,#10871,.F.);
#15204=ORIENTED_EDGE('',*,*,#10872,.F.);
#15205=ORIENTED_EDGE('',*,*,#10873,.F.);
#15206=ORIENTED_EDGE('',*,*,#10874,.F.);
#15207=ORIENTED_EDGE('',*,*,#10737,.F.);
#15208=ORIENTED_EDGE('',*,*,#10736,.T.);
#15209=ORIENTED_EDGE('',*,*,#10731,.F.);
#15210=ORIENTED_EDGE('',*,*,#10875,.F.);
#15211=ORIENTED_EDGE('',*,*,#10876,.T.);
#15212=ORIENTED_EDGE('',*,*,#10877,.T.);
#15213=ORIENTED_EDGE('',*,*,#10873,.T.);
#15214=ORIENTED_EDGE('',*,*,#10878,.T.);
#15215=ORIENTED_EDGE('',*,*,#10738,.T.);
#15216=ORIENTED_EDGE('',*,*,#10874,.T.);
#15217=ORIENTED_EDGE('',*,*,#10877,.F.);
#15218=ORIENTED_EDGE('',*,*,#10739,.F.);
#15219=ORIENTED_EDGE('',*,*,#10878,.F.);
#15220=ORIENTED_EDGE('',*,*,#10876,.F.);
#15221=ORIENTED_EDGE('',*,*,#10879,.F.);
#15222=ORIENTED_EDGE('',*,*,#10880,.F.);
#15223=ORIENTED_EDGE('',*,*,#10858,.F.);
#15224=ORIENTED_EDGE('',*,*,#10740,.T.);
#15225=ORIENTED_EDGE('',*,*,#10859,.F.);
#15226=ORIENTED_EDGE('',*,*,#10880,.T.);
#15227=ORIENTED_EDGE('',*,*,#10881,.F.);
#15228=ORIENTED_EDGE('',*,*,#10882,.T.);
#15229=ORIENTED_EDGE('',*,*,#10883,.F.);
#15230=ORIENTED_EDGE('',*,*,#10884,.F.);
#15231=ORIENTED_EDGE('',*,*,#10885,.F.);
#15232=ORIENTED_EDGE('',*,*,#10886,.F.);
#15233=ORIENTED_EDGE('',*,*,#10749,.F.);
#15234=ORIENTED_EDGE('',*,*,#10748,.T.);
#15235=ORIENTED_EDGE('',*,*,#10836,.F.);
#15236=ORIENTED_EDGE('',*,*,#10887,.F.);
#15237=ORIENTED_EDGE('',*,*,#10888,.T.);
#15238=ORIENTED_EDGE('',*,*,#10889,.T.);
#15239=ORIENTED_EDGE('',*,*,#10885,.T.);
#15240=ORIENTED_EDGE('',*,*,#10890,.T.);
#15241=ORIENTED_EDGE('',*,*,#10750,.T.);
#15242=ORIENTED_EDGE('',*,*,#10886,.T.);
#15243=ORIENTED_EDGE('',*,*,#10889,.F.);
#15244=ORIENTED_EDGE('',*,*,#10751,.F.);
#15245=ORIENTED_EDGE('',*,*,#10890,.F.);
#15246=ORIENTED_EDGE('',*,*,#10888,.F.);
#15247=ORIENTED_EDGE('',*,*,#10891,.F.);
#15248=ORIENTED_EDGE('',*,*,#10892,.F.);
#15249=ORIENTED_EDGE('',*,*,#10855,.F.);
#15250=ORIENTED_EDGE('',*,*,#10752,.T.);
#15251=ORIENTED_EDGE('',*,*,#10856,.F.);
#15252=ORIENTED_EDGE('',*,*,#10892,.T.);
#15253=ORIENTED_EDGE('',*,*,#10893,.F.);
#15254=ORIENTED_EDGE('',*,*,#10894,.T.);
#15255=ORIENTED_EDGE('',*,*,#10895,.F.);
#15256=ORIENTED_EDGE('',*,*,#10896,.F.);
#15257=ORIENTED_EDGE('',*,*,#10897,.F.);
#15258=ORIENTED_EDGE('',*,*,#10898,.F.);
#15259=ORIENTED_EDGE('',*,*,#10761,.F.);
#15260=ORIENTED_EDGE('',*,*,#10760,.T.);
#15261=ORIENTED_EDGE('',*,*,#10833,.F.);
#15262=ORIENTED_EDGE('',*,*,#10899,.F.);
#15263=ORIENTED_EDGE('',*,*,#10900,.T.);
#15264=ORIENTED_EDGE('',*,*,#10901,.T.);
#15265=ORIENTED_EDGE('',*,*,#10897,.T.);
#15266=ORIENTED_EDGE('',*,*,#10902,.T.);
#15267=ORIENTED_EDGE('',*,*,#10762,.T.);
#15268=ORIENTED_EDGE('',*,*,#10898,.T.);
#15269=ORIENTED_EDGE('',*,*,#10901,.F.);
#15270=ORIENTED_EDGE('',*,*,#10763,.F.);
#15271=ORIENTED_EDGE('',*,*,#10902,.F.);
#15272=ORIENTED_EDGE('',*,*,#10900,.F.);
#15273=ORIENTED_EDGE('',*,*,#10903,.F.);
#15274=ORIENTED_EDGE('',*,*,#10904,.F.);
#15275=ORIENTED_EDGE('',*,*,#10852,.F.);
#15276=ORIENTED_EDGE('',*,*,#10764,.T.);
#15277=ORIENTED_EDGE('',*,*,#10853,.F.);
#15278=ORIENTED_EDGE('',*,*,#10904,.T.);
#15279=ORIENTED_EDGE('',*,*,#10905,.F.);
#15280=ORIENTED_EDGE('',*,*,#10906,.T.);
#15281=ORIENTED_EDGE('',*,*,#10907,.F.);
#15282=ORIENTED_EDGE('',*,*,#10908,.F.);
#15283=ORIENTED_EDGE('',*,*,#10909,.F.);
#15284=ORIENTED_EDGE('',*,*,#10910,.F.);
#15285=ORIENTED_EDGE('',*,*,#10773,.F.);
#15286=ORIENTED_EDGE('',*,*,#10772,.T.);
#15287=ORIENTED_EDGE('',*,*,#10830,.F.);
#15288=ORIENTED_EDGE('',*,*,#10911,.F.);
#15289=ORIENTED_EDGE('',*,*,#10912,.T.);
#15290=ORIENTED_EDGE('',*,*,#10913,.T.);
#15291=ORIENTED_EDGE('',*,*,#10909,.T.);
#15292=ORIENTED_EDGE('',*,*,#10914,.T.);
#15293=ORIENTED_EDGE('',*,*,#10777,.T.);
#15294=ORIENTED_EDGE('',*,*,#10774,.T.);
#15295=ORIENTED_EDGE('',*,*,#10910,.T.);
#15296=ORIENTED_EDGE('',*,*,#10913,.F.);
#15297=ORIENTED_EDGE('',*,*,#10778,.F.);
#15298=ORIENTED_EDGE('',*,*,#10914,.F.);
#15299=ORIENTED_EDGE('',*,*,#10912,.F.);
#15300=ORIENTED_EDGE('',*,*,#10915,.F.);
#15301=ORIENTED_EDGE('',*,*,#10916,.F.);
#15302=ORIENTED_EDGE('',*,*,#10849,.F.);
#15303=ORIENTED_EDGE('',*,*,#10779,.T.);
#15304=ORIENTED_EDGE('',*,*,#10850,.F.);
#15305=ORIENTED_EDGE('',*,*,#10916,.T.);
#15306=ORIENTED_EDGE('',*,*,#10917,.F.);
#15307=ORIENTED_EDGE('',*,*,#10918,.T.);
#15308=ORIENTED_EDGE('',*,*,#10919,.F.);
#15309=ORIENTED_EDGE('',*,*,#10920,.F.);
#15310=ORIENTED_EDGE('',*,*,#10921,.F.);
#15311=ORIENTED_EDGE('',*,*,#10922,.F.);
#15312=ORIENTED_EDGE('',*,*,#10788,.F.);
#15313=ORIENTED_EDGE('',*,*,#10787,.T.);
#15314=ORIENTED_EDGE('',*,*,#10827,.F.);
#15315=ORIENTED_EDGE('',*,*,#10923,.F.);
#15316=ORIENTED_EDGE('',*,*,#10924,.T.);
#15317=ORIENTED_EDGE('',*,*,#10925,.T.);
#15318=ORIENTED_EDGE('',*,*,#10921,.T.);
#15319=ORIENTED_EDGE('',*,*,#10926,.T.);
#15320=ORIENTED_EDGE('',*,*,#10789,.T.);
#15321=ORIENTED_EDGE('',*,*,#10922,.T.);
#15322=ORIENTED_EDGE('',*,*,#10925,.F.);
#15323=ORIENTED_EDGE('',*,*,#10790,.F.);
#15324=ORIENTED_EDGE('',*,*,#10926,.F.);
#15325=ORIENTED_EDGE('',*,*,#10924,.F.);
#15326=ORIENTED_EDGE('',*,*,#10927,.F.);
#15327=ORIENTED_EDGE('',*,*,#10928,.F.);
#15328=ORIENTED_EDGE('',*,*,#10846,.F.);
#15329=ORIENTED_EDGE('',*,*,#10791,.T.);
#15330=ORIENTED_EDGE('',*,*,#10847,.F.);
#15331=ORIENTED_EDGE('',*,*,#10928,.T.);
#15332=ORIENTED_EDGE('',*,*,#10929,.F.);
#15333=ORIENTED_EDGE('',*,*,#10930,.T.);
#15334=ORIENTED_EDGE('',*,*,#10931,.F.);
#15335=ORIENTED_EDGE('',*,*,#10932,.F.);
#15336=ORIENTED_EDGE('',*,*,#10933,.F.);
#15337=ORIENTED_EDGE('',*,*,#10934,.F.);
#15338=ORIENTED_EDGE('',*,*,#10800,.F.);
#15339=ORIENTED_EDGE('',*,*,#10799,.T.);
#15340=ORIENTED_EDGE('',*,*,#10824,.F.);
#15341=ORIENTED_EDGE('',*,*,#10935,.F.);
#15342=ORIENTED_EDGE('',*,*,#10936,.T.);
#15343=ORIENTED_EDGE('',*,*,#10937,.T.);
#15344=ORIENTED_EDGE('',*,*,#10933,.T.);
#15345=ORIENTED_EDGE('',*,*,#10938,.T.);
#15346=ORIENTED_EDGE('',*,*,#10801,.T.);
#15347=ORIENTED_EDGE('',*,*,#10934,.T.);
#15348=ORIENTED_EDGE('',*,*,#10937,.F.);
#15349=ORIENTED_EDGE('',*,*,#10802,.F.);
#15350=ORIENTED_EDGE('',*,*,#10938,.F.);
#15351=ORIENTED_EDGE('',*,*,#10936,.F.);
#15352=ORIENTED_EDGE('',*,*,#10939,.F.);
#15353=ORIENTED_EDGE('',*,*,#10940,.F.);
#15354=ORIENTED_EDGE('',*,*,#10843,.F.);
#15355=ORIENTED_EDGE('',*,*,#10803,.T.);
#15356=ORIENTED_EDGE('',*,*,#10844,.F.);
#15357=ORIENTED_EDGE('',*,*,#10940,.T.);
#15358=ORIENTED_EDGE('',*,*,#10941,.F.);
#15359=ORIENTED_EDGE('',*,*,#10942,.T.);
#15360=ORIENTED_EDGE('',*,*,#10943,.F.);
#15361=ORIENTED_EDGE('',*,*,#10728,.F.);
#15362=ORIENTED_EDGE('',*,*,#10944,.F.);
#15363=ORIENTED_EDGE('',*,*,#10945,.F.);
#15364=ORIENTED_EDGE('',*,*,#10812,.F.);
#15365=ORIENTED_EDGE('',*,*,#10811,.T.);
#15366=ORIENTED_EDGE('',*,*,#10821,.F.);
#15367=ORIENTED_EDGE('',*,*,#10727,.F.);
#15368=ORIENTED_EDGE('',*,*,#10946,.T.);
#15369=ORIENTED_EDGE('',*,*,#10947,.T.);
#15370=ORIENTED_EDGE('',*,*,#10944,.T.);
#15371=ORIENTED_EDGE('',*,*,#10948,.T.);
#15372=ORIENTED_EDGE('',*,*,#10813,.T.);
#15373=ORIENTED_EDGE('',*,*,#10945,.T.);
#15374=ORIENTED_EDGE('',*,*,#10947,.F.);
#15375=ORIENTED_EDGE('',*,*,#10814,.F.);
#15376=ORIENTED_EDGE('',*,*,#10948,.F.);
#15377=ORIENTED_EDGE('',*,*,#10946,.F.);
#15378=ORIENTED_EDGE('',*,*,#10726,.F.);
#15379=ORIENTED_EDGE('',*,*,#10949,.F.);
#15380=ORIENTED_EDGE('',*,*,#10840,.F.);
#15381=ORIENTED_EDGE('',*,*,#10815,.T.);
#15382=ORIENTED_EDGE('',*,*,#10841,.F.);
#15383=ORIENTED_EDGE('',*,*,#10949,.T.);
#15384=ORIENTED_EDGE('',*,*,#10725,.F.);
#15385=ORIENTED_EDGE('',*,*,#10950,.T.);
#15386=ORIENTED_EDGE('',*,*,#10882,.F.);
#15387=ORIENTED_EDGE('',*,*,#10951,.F.);
#15388=ORIENTED_EDGE('',*,*,#10952,.F.);
#15389=ORIENTED_EDGE('',*,*,#10953,.F.);
#15390=ORIENTED_EDGE('',*,*,#10954,.F.);
#15391=ORIENTED_EDGE('',*,*,#10743,.F.);
#15392=ORIENTED_EDGE('',*,*,#10742,.T.);
#15393=ORIENTED_EDGE('',*,*,#10857,.F.);
#15394=ORIENTED_EDGE('',*,*,#10955,.F.);
#15395=ORIENTED_EDGE('',*,*,#10956,.T.);
#15396=ORIENTED_EDGE('',*,*,#10957,.T.);
#15397=ORIENTED_EDGE('',*,*,#10952,.T.);
#15398=ORIENTED_EDGE('',*,*,#10954,.T.);
#15399=ORIENTED_EDGE('',*,*,#10953,.T.);
#15400=ORIENTED_EDGE('',*,*,#10957,.F.);
#15401=ORIENTED_EDGE('',*,*,#10958,.T.);
#15402=ORIENTED_EDGE('',*,*,#10744,.T.);
#15403=ORIENTED_EDGE('',*,*,#10745,.F.);
#15404=ORIENTED_EDGE('',*,*,#10958,.F.);
#15405=ORIENTED_EDGE('',*,*,#10956,.F.);
#15406=ORIENTED_EDGE('',*,*,#10959,.F.);
#15407=ORIENTED_EDGE('',*,*,#10960,.F.);
#15408=ORIENTED_EDGE('',*,*,#10837,.F.);
#15409=ORIENTED_EDGE('',*,*,#10746,.T.);
#15410=ORIENTED_EDGE('',*,*,#10838,.F.);
#15411=ORIENTED_EDGE('',*,*,#10960,.T.);
#15412=ORIENTED_EDGE('',*,*,#10961,.F.);
#15413=ORIENTED_EDGE('',*,*,#10883,.T.);
#15414=ORIENTED_EDGE('',*,*,#10894,.F.);
#15415=ORIENTED_EDGE('',*,*,#10962,.F.);
#15416=ORIENTED_EDGE('',*,*,#10963,.F.);
#15417=ORIENTED_EDGE('',*,*,#10964,.F.);
#15418=ORIENTED_EDGE('',*,*,#10965,.F.);
#15419=ORIENTED_EDGE('',*,*,#10755,.F.);
#15420=ORIENTED_EDGE('',*,*,#10754,.T.);
#15421=ORIENTED_EDGE('',*,*,#10854,.F.);
#15422=ORIENTED_EDGE('',*,*,#10966,.F.);
#15423=ORIENTED_EDGE('',*,*,#10967,.T.);
#15424=ORIENTED_EDGE('',*,*,#10968,.T.);
#15425=ORIENTED_EDGE('',*,*,#10963,.T.);
#15426=ORIENTED_EDGE('',*,*,#10965,.T.);
#15427=ORIENTED_EDGE('',*,*,#10964,.T.);
#15428=ORIENTED_EDGE('',*,*,#10968,.F.);
#15429=ORIENTED_EDGE('',*,*,#10969,.T.);
#15430=ORIENTED_EDGE('',*,*,#10756,.T.);
#15431=ORIENTED_EDGE('',*,*,#10757,.F.);
#15432=ORIENTED_EDGE('',*,*,#10969,.F.);
#15433=ORIENTED_EDGE('',*,*,#10967,.F.);
#15434=ORIENTED_EDGE('',*,*,#10970,.F.);
#15435=ORIENTED_EDGE('',*,*,#10971,.F.);
#15436=ORIENTED_EDGE('',*,*,#10834,.F.);
#15437=ORIENTED_EDGE('',*,*,#10758,.T.);
#15438=ORIENTED_EDGE('',*,*,#10835,.F.);
#15439=ORIENTED_EDGE('',*,*,#10971,.T.);
#15440=ORIENTED_EDGE('',*,*,#10972,.F.);
#15441=ORIENTED_EDGE('',*,*,#10895,.T.);
#15442=ORIENTED_EDGE('',*,*,#10906,.F.);
#15443=ORIENTED_EDGE('',*,*,#10973,.F.);
#15444=ORIENTED_EDGE('',*,*,#10974,.F.);
#15445=ORIENTED_EDGE('',*,*,#10975,.F.);
#15446=ORIENTED_EDGE('',*,*,#10976,.F.);
#15447=ORIENTED_EDGE('',*,*,#10767,.F.);
#15448=ORIENTED_EDGE('',*,*,#10766,.T.);
#15449=ORIENTED_EDGE('',*,*,#10851,.F.);
#15450=ORIENTED_EDGE('',*,*,#10977,.F.);
#15451=ORIENTED_EDGE('',*,*,#10978,.T.);
#15452=ORIENTED_EDGE('',*,*,#10979,.T.);
#15453=ORIENTED_EDGE('',*,*,#10974,.T.);
#15454=ORIENTED_EDGE('',*,*,#10976,.T.);
#15455=ORIENTED_EDGE('',*,*,#10975,.T.);
#15456=ORIENTED_EDGE('',*,*,#10979,.F.);
#15457=ORIENTED_EDGE('',*,*,#10980,.T.);
#15458=ORIENTED_EDGE('',*,*,#10768,.T.);
#15459=ORIENTED_EDGE('',*,*,#10769,.F.);
#15460=ORIENTED_EDGE('',*,*,#10980,.F.);
#15461=ORIENTED_EDGE('',*,*,#10978,.F.);
#15462=ORIENTED_EDGE('',*,*,#10981,.F.);
#15463=ORIENTED_EDGE('',*,*,#10982,.F.);
#15464=ORIENTED_EDGE('',*,*,#10831,.F.);
#15465=ORIENTED_EDGE('',*,*,#10770,.T.);
#15466=ORIENTED_EDGE('',*,*,#10832,.F.);
#15467=ORIENTED_EDGE('',*,*,#10982,.T.);
#15468=ORIENTED_EDGE('',*,*,#10983,.F.);
#15469=ORIENTED_EDGE('',*,*,#10907,.T.);
#15470=ORIENTED_EDGE('',*,*,#10918,.F.);
#15471=ORIENTED_EDGE('',*,*,#10984,.F.);
#15472=ORIENTED_EDGE('',*,*,#10985,.F.);
#15473=ORIENTED_EDGE('',*,*,#10986,.F.);
#15474=ORIENTED_EDGE('',*,*,#10987,.F.);
#15475=ORIENTED_EDGE('',*,*,#10782,.F.);
#15476=ORIENTED_EDGE('',*,*,#10781,.T.);
#15477=ORIENTED_EDGE('',*,*,#10848,.F.);
#15478=ORIENTED_EDGE('',*,*,#10988,.F.);
#15479=ORIENTED_EDGE('',*,*,#10989,.T.);
#15480=ORIENTED_EDGE('',*,*,#10990,.T.);
#15481=ORIENTED_EDGE('',*,*,#10985,.T.);
#15482=ORIENTED_EDGE('',*,*,#10987,.T.);
#15483=ORIENTED_EDGE('',*,*,#10986,.T.);
#15484=ORIENTED_EDGE('',*,*,#10990,.F.);
#15485=ORIENTED_EDGE('',*,*,#10991,.T.);
#15486=ORIENTED_EDGE('',*,*,#10783,.T.);
#15487=ORIENTED_EDGE('',*,*,#10784,.F.);
#15488=ORIENTED_EDGE('',*,*,#10991,.F.);
#15489=ORIENTED_EDGE('',*,*,#10989,.F.);
#15490=ORIENTED_EDGE('',*,*,#10992,.F.);
#15491=ORIENTED_EDGE('',*,*,#10993,.F.);
#15492=ORIENTED_EDGE('',*,*,#10828,.F.);
#15493=ORIENTED_EDGE('',*,*,#10785,.T.);
#15494=ORIENTED_EDGE('',*,*,#10829,.F.);
#15495=ORIENTED_EDGE('',*,*,#10993,.T.);
#15496=ORIENTED_EDGE('',*,*,#10994,.F.);
#15497=ORIENTED_EDGE('',*,*,#10919,.T.);
#15498=ORIENTED_EDGE('',*,*,#10930,.F.);
#15499=ORIENTED_EDGE('',*,*,#10995,.F.);
#15500=ORIENTED_EDGE('',*,*,#10996,.F.);
#15501=ORIENTED_EDGE('',*,*,#10997,.F.);
#15502=ORIENTED_EDGE('',*,*,#10998,.F.);
#15503=ORIENTED_EDGE('',*,*,#10794,.F.);
#15504=ORIENTED_EDGE('',*,*,#10793,.T.);
#15505=ORIENTED_EDGE('',*,*,#10845,.F.);
#15506=ORIENTED_EDGE('',*,*,#10999,.F.);
#15507=ORIENTED_EDGE('',*,*,#11000,.T.);
#15508=ORIENTED_EDGE('',*,*,#11001,.T.);
#15509=ORIENTED_EDGE('',*,*,#10996,.T.);
#15510=ORIENTED_EDGE('',*,*,#10998,.T.);
#15511=ORIENTED_EDGE('',*,*,#10997,.T.);
#15512=ORIENTED_EDGE('',*,*,#11001,.F.);
#15513=ORIENTED_EDGE('',*,*,#11002,.T.);
#15514=ORIENTED_EDGE('',*,*,#10795,.T.);
#15515=ORIENTED_EDGE('',*,*,#10796,.F.);
#15516=ORIENTED_EDGE('',*,*,#11002,.F.);
#15517=ORIENTED_EDGE('',*,*,#11000,.F.);
#15518=ORIENTED_EDGE('',*,*,#11003,.F.);
#15519=ORIENTED_EDGE('',*,*,#11004,.F.);
#15520=ORIENTED_EDGE('',*,*,#10825,.F.);
#15521=ORIENTED_EDGE('',*,*,#10797,.T.);
#15522=ORIENTED_EDGE('',*,*,#10826,.F.);
#15523=ORIENTED_EDGE('',*,*,#11004,.T.);
#15524=ORIENTED_EDGE('',*,*,#11005,.F.);
#15525=ORIENTED_EDGE('',*,*,#10931,.T.);
#15526=ORIENTED_EDGE('',*,*,#10942,.F.);
#15527=ORIENTED_EDGE('',*,*,#11006,.F.);
#15528=ORIENTED_EDGE('',*,*,#11007,.F.);
#15529=ORIENTED_EDGE('',*,*,#11008,.F.);
#15530=ORIENTED_EDGE('',*,*,#11009,.F.);
#15531=ORIENTED_EDGE('',*,*,#10806,.F.);
#15532=ORIENTED_EDGE('',*,*,#10805,.T.);
#15533=ORIENTED_EDGE('',*,*,#10842,.F.);
#15534=ORIENTED_EDGE('',*,*,#11010,.F.);
#15535=ORIENTED_EDGE('',*,*,#11011,.F.);
#15536=ORIENTED_EDGE('',*,*,#11012,.T.);
#15537=ORIENTED_EDGE('',*,*,#11013,.T.);
#15538=ORIENTED_EDGE('',*,*,#11007,.T.);
#15539=ORIENTED_EDGE('',*,*,#11009,.T.);
#15540=ORIENTED_EDGE('',*,*,#11008,.T.);
#15541=ORIENTED_EDGE('',*,*,#11013,.F.);
#15542=ORIENTED_EDGE('',*,*,#11014,.T.);
#15543=ORIENTED_EDGE('',*,*,#10807,.T.);
#15544=ORIENTED_EDGE('',*,*,#10808,.F.);
#15545=ORIENTED_EDGE('',*,*,#11014,.F.);
#15546=ORIENTED_EDGE('',*,*,#11012,.F.);
#15547=ORIENTED_EDGE('',*,*,#11015,.F.);
#15548=ORIENTED_EDGE('',*,*,#10730,.F.);
#15549=ORIENTED_EDGE('',*,*,#11016,.F.);
#15550=ORIENTED_EDGE('',*,*,#10822,.F.);
#15551=ORIENTED_EDGE('',*,*,#10809,.T.);
#15552=ORIENTED_EDGE('',*,*,#10823,.F.);
#15553=ORIENTED_EDGE('',*,*,#11016,.T.);
#15554=ORIENTED_EDGE('',*,*,#10729,.F.);
#15555=ORIENTED_EDGE('',*,*,#10943,.T.);
#15556=ORIENTED_EDGE('',*,*,#10723,.T.);
#15557=ORIENTED_EDGE('',*,*,#11015,.T.);
#15558=ORIENTED_EDGE('',*,*,#11011,.T.);
#15559=ORIENTED_EDGE('',*,*,#11017,.T.);
#15560=ORIENTED_EDGE('',*,*,#11018,.F.);
#15561=ORIENTED_EDGE('',*,*,#11019,.F.);
#15562=ORIENTED_EDGE('',*,*,#11017,.F.);
#15563=ORIENTED_EDGE('',*,*,#11010,.T.);
#15564=ORIENTED_EDGE('',*,*,#11006,.T.);
#15565=ORIENTED_EDGE('',*,*,#10941,.T.);
#15566=ORIENTED_EDGE('',*,*,#10939,.T.);
#15567=ORIENTED_EDGE('',*,*,#10935,.T.);
#15568=ORIENTED_EDGE('',*,*,#10932,.T.);
#15569=ORIENTED_EDGE('',*,*,#11005,.T.);
#15570=ORIENTED_EDGE('',*,*,#11003,.T.);
#15571=ORIENTED_EDGE('',*,*,#10999,.T.);
#15572=ORIENTED_EDGE('',*,*,#10995,.T.);
#15573=ORIENTED_EDGE('',*,*,#10929,.T.);
#15574=ORIENTED_EDGE('',*,*,#10927,.T.);
#15575=ORIENTED_EDGE('',*,*,#10923,.T.);
#15576=ORIENTED_EDGE('',*,*,#10920,.T.);
#15577=ORIENTED_EDGE('',*,*,#10994,.T.);
#15578=ORIENTED_EDGE('',*,*,#10992,.T.);
#15579=ORIENTED_EDGE('',*,*,#10988,.T.);
#15580=ORIENTED_EDGE('',*,*,#10984,.T.);
#15581=ORIENTED_EDGE('',*,*,#10917,.T.);
#15582=ORIENTED_EDGE('',*,*,#10915,.T.);
#15583=ORIENTED_EDGE('',*,*,#10911,.T.);
#15584=ORIENTED_EDGE('',*,*,#10908,.T.);
#15585=ORIENTED_EDGE('',*,*,#10983,.T.);
#15586=ORIENTED_EDGE('',*,*,#10981,.T.);
#15587=ORIENTED_EDGE('',*,*,#10977,.T.);
#15588=ORIENTED_EDGE('',*,*,#10973,.T.);
#15589=ORIENTED_EDGE('',*,*,#10905,.T.);
#15590=ORIENTED_EDGE('',*,*,#10903,.T.);
#15591=ORIENTED_EDGE('',*,*,#10899,.T.);
#15592=ORIENTED_EDGE('',*,*,#10896,.T.);
#15593=ORIENTED_EDGE('',*,*,#10972,.T.);
#15594=ORIENTED_EDGE('',*,*,#10970,.T.);
#15595=ORIENTED_EDGE('',*,*,#10966,.T.);
#15596=ORIENTED_EDGE('',*,*,#10962,.T.);
#15597=ORIENTED_EDGE('',*,*,#10893,.T.);
#15598=ORIENTED_EDGE('',*,*,#10891,.T.);
#15599=ORIENTED_EDGE('',*,*,#10887,.T.);
#15600=ORIENTED_EDGE('',*,*,#10884,.T.);
#15601=ORIENTED_EDGE('',*,*,#10961,.T.);
#15602=ORIENTED_EDGE('',*,*,#10959,.T.);
#15603=ORIENTED_EDGE('',*,*,#10955,.T.);
#15604=ORIENTED_EDGE('',*,*,#10951,.T.);
#15605=ORIENTED_EDGE('',*,*,#10881,.T.);
#15606=ORIENTED_EDGE('',*,*,#10879,.T.);
#15607=ORIENTED_EDGE('',*,*,#10875,.T.);
#15608=ORIENTED_EDGE('',*,*,#10872,.T.);
#15609=ORIENTED_EDGE('',*,*,#11020,.T.);
#15610=ORIENTED_EDGE('',*,*,#11021,.T.);
#15611=ORIENTED_EDGE('',*,*,#11022,.T.);
#15612=ORIENTED_EDGE('',*,*,#11023,.T.);
#15613=ORIENTED_EDGE('',*,*,#10950,.F.);
#15614=ORIENTED_EDGE('',*,*,#10724,.F.);
#15615=ORIENTED_EDGE('',*,*,#11023,.F.);
#15616=ORIENTED_EDGE('',*,*,#11024,.F.);
#15617=ORIENTED_EDGE('',*,*,#11025,.F.);
#15618=ORIENTED_EDGE('',*,*,#11026,.F.);
#15619=ORIENTED_EDGE('',*,*,#10818,.F.);
#15620=ORIENTED_EDGE('',*,*,#10817,.T.);
#15621=ORIENTED_EDGE('',*,*,#10839,.F.);
#15622=ORIENTED_EDGE('',*,*,#11022,.F.);
#15623=ORIENTED_EDGE('',*,*,#11027,.T.);
#15624=ORIENTED_EDGE('',*,*,#11028,.T.);
#15625=ORIENTED_EDGE('',*,*,#11024,.T.);
#15626=ORIENTED_EDGE('',*,*,#11026,.T.);
#15627=ORIENTED_EDGE('',*,*,#11025,.T.);
#15628=ORIENTED_EDGE('',*,*,#11028,.F.);
#15629=ORIENTED_EDGE('',*,*,#11029,.T.);
#15630=ORIENTED_EDGE('',*,*,#10819,.T.);
#15631=ORIENTED_EDGE('',*,*,#10820,.F.);
#15632=ORIENTED_EDGE('',*,*,#11029,.F.);
#15633=ORIENTED_EDGE('',*,*,#11027,.F.);
#15634=ORIENTED_EDGE('',*,*,#11021,.F.);
#15635=ORIENTED_EDGE('',*,*,#11030,.F.);
#15636=ORIENTED_EDGE('',*,*,#10733,.F.);
#15637=ORIENTED_EDGE('',*,*,#10735,.T.);
#15638=ORIENTED_EDGE('',*,*,#10776,.F.);
#15639=ORIENTED_EDGE('',*,*,#11031,.T.);
#15640=ORIENTED_EDGE('',*,*,#10867,.T.);
#15641=ORIENTED_EDGE('',*,*,#11031,.F.);
#15642=ORIENTED_EDGE('',*,*,#10734,.F.);
#15643=ORIENTED_EDGE('',*,*,#11030,.T.);
#15644=ORIENTED_EDGE('',*,*,#11020,.F.);
#15645=ORIENTED_EDGE('',*,*,#10871,.T.);
#15646=ORIENTED_EDGE('',*,*,#11032,.F.);
#15647=ORIENTED_EDGE('',*,*,#11033,.T.);
#15648=ORIENTED_EDGE('',*,*,#11018,.T.);
#15649=ORIENTED_EDGE('',*,*,#11019,.T.);
#15650=ORIENTED_EDGE('',*,*,#11033,.F.);
#15651=ORIENTED_EDGE('',*,*,#11034,.F.);
#15652=ORIENTED_EDGE('',*,*,#11035,.T.);
#15653=ORIENTED_EDGE('',*,*,#11032,.T.);
#15654=ORIENTED_EDGE('',*,*,#11035,.F.);
#15655=ORIENTED_EDGE('',*,*,#10870,.F.);
#15656=ORIENTED_EDGE('',*,*,#11036,.T.);
#15657=ORIENTED_EDGE('',*,*,#11034,.T.);
#15658=ORIENTED_EDGE('',*,*,#11036,.F.);
#15659=ORIENTED_EDGE('',*,*,#11037,.T.);
#15660=ORIENTED_EDGE('',*,*,#11038,.T.);
#15661=ORIENTED_EDGE('',*,*,#11039,.T.);
#15662=ORIENTED_EDGE('',*,*,#11040,.T.);
#15663=ORIENTED_EDGE('',*,*,#11041,.T.);
#15664=ORIENTED_EDGE('',*,*,#11038,.F.);
#15665=ORIENTED_EDGE('',*,*,#11042,.F.);
#15666=ORIENTED_EDGE('',*,*,#11043,.F.);
#15667=ORIENTED_EDGE('',*,*,#11044,.F.);
#15668=ORIENTED_EDGE('',*,*,#11037,.F.);
#15669=ORIENTED_EDGE('',*,*,#11045,.F.);
#15670=ORIENTED_EDGE('',*,*,#11046,.T.);
#15671=ORIENTED_EDGE('',*,*,#11047,.T.);
#15672=ORIENTED_EDGE('',*,*,#11048,.T.);
#15673=ORIENTED_EDGE('',*,*,#11042,.T.);
#15674=ORIENTED_EDGE('',*,*,#11049,.T.);
#15675=ORIENTED_EDGE('',*,*,#11050,.T.);
#15676=ORIENTED_EDGE('',*,*,#11051,.T.);
#15677=ORIENTED_EDGE('',*,*,#11052,.T.);
#15678=ORIENTED_EDGE('',*,*,#11053,.T.);
#15679=ORIENTED_EDGE('',*,*,#11050,.F.);
#15680=ORIENTED_EDGE('',*,*,#11054,.F.);
#15681=ORIENTED_EDGE('',*,*,#11055,.F.);
#15682=ORIENTED_EDGE('',*,*,#11056,.F.);
#15683=ORIENTED_EDGE('',*,*,#11049,.F.);
#15684=ORIENTED_EDGE('',*,*,#11057,.F.);
#15685=ORIENTED_EDGE('',*,*,#11058,.T.);
#15686=ORIENTED_EDGE('',*,*,#11059,.T.);
#15687=ORIENTED_EDGE('',*,*,#11060,.T.);
#15688=ORIENTED_EDGE('',*,*,#11054,.T.);
#15689=ORIENTED_EDGE('',*,*,#11061,.T.);
#15690=ORIENTED_EDGE('',*,*,#11062,.T.);
#15691=ORIENTED_EDGE('',*,*,#11063,.T.);
#15692=ORIENTED_EDGE('',*,*,#11064,.T.);
#15693=ORIENTED_EDGE('',*,*,#11065,.T.);
#15694=ORIENTED_EDGE('',*,*,#11062,.F.);
#15695=ORIENTED_EDGE('',*,*,#11066,.F.);
#15696=ORIENTED_EDGE('',*,*,#11067,.F.);
#15697=ORIENTED_EDGE('',*,*,#11068,.F.);
#15698=ORIENTED_EDGE('',*,*,#11061,.F.);
#15699=ORIENTED_EDGE('',*,*,#11069,.F.);
#15700=ORIENTED_EDGE('',*,*,#11070,.T.);
#15701=ORIENTED_EDGE('',*,*,#11071,.T.);
#15702=ORIENTED_EDGE('',*,*,#11072,.T.);
#15703=ORIENTED_EDGE('',*,*,#11066,.T.);
#15704=ORIENTED_EDGE('',*,*,#11073,.T.);
#15705=ORIENTED_EDGE('',*,*,#11074,.T.);
#15706=ORIENTED_EDGE('',*,*,#11075,.T.);
#15707=ORIENTED_EDGE('',*,*,#11076,.T.);
#15708=ORIENTED_EDGE('',*,*,#11074,.F.);
#15709=ORIENTED_EDGE('',*,*,#11077,.T.);
#15710=ORIENTED_EDGE('',*,*,#11078,.T.);
#15711=ORIENTED_EDGE('',*,*,#11079,.F.);
#15712=ORIENTED_EDGE('',*,*,#11080,.F.);
#15713=ORIENTED_EDGE('',*,*,#11081,.F.);
#15714=ORIENTED_EDGE('',*,*,#11073,.F.);
#15715=ORIENTED_EDGE('',*,*,#11082,.F.);
#15716=ORIENTED_EDGE('',*,*,#11083,.F.);
#15717=ORIENTED_EDGE('',*,*,#11084,.F.);
#15718=ORIENTED_EDGE('',*,*,#11085,.F.);
#15719=ORIENTED_EDGE('',*,*,#11086,.F.);
#15720=ORIENTED_EDGE('',*,*,#11087,.F.);
#15721=ORIENTED_EDGE('',*,*,#11088,.F.);
#15722=ORIENTED_EDGE('',*,*,#11089,.F.);
#15723=ORIENTED_EDGE('',*,*,#11090,.F.);
#15724=ORIENTED_EDGE('',*,*,#11091,.F.);
#15725=ORIENTED_EDGE('',*,*,#11070,.F.);
#15726=ORIENTED_EDGE('',*,*,#11092,.F.);
#15727=ORIENTED_EDGE('',*,*,#11078,.F.);
#15728=ORIENTED_EDGE('',*,*,#11077,.F.);
#15729=ORIENTED_EDGE('',*,*,#11084,.T.);
#15730=ORIENTED_EDGE('',*,*,#11093,.T.);
#15731=ORIENTED_EDGE('',*,*,#11094,.T.);
#15732=ORIENTED_EDGE('',*,*,#11095,.T.);
#15733=ORIENTED_EDGE('',*,*,#11093,.F.);
#15734=ORIENTED_EDGE('',*,*,#11083,.T.);
#15735=ORIENTED_EDGE('',*,*,#11096,.F.);
#15736=ORIENTED_EDGE('',*,*,#11097,.F.);
#15737=ORIENTED_EDGE('',*,*,#11098,.T.);
#15738=ORIENTED_EDGE('',*,*,#11099,.T.);
#15739=ORIENTED_EDGE('',*,*,#11100,.T.);
#15740=ORIENTED_EDGE('',*,*,#11101,.T.);
#15741=ORIENTED_EDGE('',*,*,#11102,.T.);
#15742=ORIENTED_EDGE('',*,*,#11099,.F.);
#15743=ORIENTED_EDGE('',*,*,#11103,.F.);
#15744=ORIENTED_EDGE('',*,*,#11104,.F.);
#15745=ORIENTED_EDGE('',*,*,#11105,.F.);
#15746=ORIENTED_EDGE('',*,*,#11098,.F.);
#15747=ORIENTED_EDGE('',*,*,#11106,.T.);
#15748=ORIENTED_EDGE('',*,*,#11107,.T.);
#15749=ORIENTED_EDGE('',*,*,#11108,.T.);
#15750=ORIENTED_EDGE('',*,*,#11109,.F.);
#15751=ORIENTED_EDGE('',*,*,#11103,.T.);
#15752=ORIENTED_EDGE('',*,*,#11102,.F.);
#15753=ORIENTED_EDGE('',*,*,#11110,.T.);
#15754=ORIENTED_EDGE('',*,*,#11111,.T.);
#15755=ORIENTED_EDGE('',*,*,#11112,.F.);
#15756=ORIENTED_EDGE('',*,*,#11113,.T.);
#15757=ORIENTED_EDGE('',*,*,#11106,.F.);
#15758=ORIENTED_EDGE('',*,*,#11114,.T.);
#15759=ORIENTED_EDGE('',*,*,#11115,.T.);
#15760=ORIENTED_EDGE('',*,*,#11116,.T.);
#15761=ORIENTED_EDGE('',*,*,#11117,.T.);
#15762=ORIENTED_EDGE('',*,*,#11118,.T.);
#15763=ORIENTED_EDGE('',*,*,#11115,.F.);
#15764=ORIENTED_EDGE('',*,*,#11119,.F.);
#15765=ORIENTED_EDGE('',*,*,#11120,.F.);
#15766=ORIENTED_EDGE('',*,*,#11121,.F.);
#15767=ORIENTED_EDGE('',*,*,#11114,.F.);
#15768=ORIENTED_EDGE('',*,*,#11122,.T.);
#15769=ORIENTED_EDGE('',*,*,#11123,.T.);
#15770=ORIENTED_EDGE('',*,*,#11124,.T.);
#15771=ORIENTED_EDGE('',*,*,#11111,.F.);
#15772=ORIENTED_EDGE('',*,*,#11119,.T.);
#15773=ORIENTED_EDGE('',*,*,#11118,.F.);
#15774=ORIENTED_EDGE('',*,*,#11125,.T.);
#15775=ORIENTED_EDGE('',*,*,#11126,.T.);
#15776=ORIENTED_EDGE('',*,*,#11127,.F.);
#15777=ORIENTED_EDGE('',*,*,#11128,.T.);
#15778=ORIENTED_EDGE('',*,*,#11122,.F.);
#15779=ORIENTED_EDGE('',*,*,#11129,.T.);
#15780=ORIENTED_EDGE('',*,*,#11130,.T.);
#15781=ORIENTED_EDGE('',*,*,#11131,.T.);
#15782=ORIENTED_EDGE('',*,*,#11132,.T.);
#15783=ORIENTED_EDGE('',*,*,#11133,.T.);
#15784=ORIENTED_EDGE('',*,*,#11130,.F.);
#15785=ORIENTED_EDGE('',*,*,#11134,.F.);
#15786=ORIENTED_EDGE('',*,*,#11135,.F.);
#15787=ORIENTED_EDGE('',*,*,#11136,.F.);
#15788=ORIENTED_EDGE('',*,*,#11129,.F.);
#15789=ORIENTED_EDGE('',*,*,#11137,.F.);
#15790=ORIENTED_EDGE('',*,*,#11138,.T.);
#15791=ORIENTED_EDGE('',*,*,#11139,.T.);
#15792=ORIENTED_EDGE('',*,*,#11126,.F.);
#15793=ORIENTED_EDGE('',*,*,#11134,.T.);
#15794=ORIENTED_EDGE('',*,*,#11140,.T.);
#15795=ORIENTED_EDGE('',*,*,#11141,.T.);
#15796=ORIENTED_EDGE('',*,*,#11142,.T.);
#15797=ORIENTED_EDGE('',*,*,#11143,.T.);
#15798=ORIENTED_EDGE('',*,*,#11144,.T.);
#15799=ORIENTED_EDGE('',*,*,#11141,.F.);
#15800=ORIENTED_EDGE('',*,*,#11145,.F.);
#15801=ORIENTED_EDGE('',*,*,#11146,.F.);
#15802=ORIENTED_EDGE('',*,*,#11147,.F.);
#15803=ORIENTED_EDGE('',*,*,#11140,.F.);
#15804=ORIENTED_EDGE('',*,*,#11148,.T.);
#15805=ORIENTED_EDGE('',*,*,#11087,.T.);
#15806=ORIENTED_EDGE('',*,*,#11149,.T.);
#15807=ORIENTED_EDGE('',*,*,#11145,.T.);
#15808=ORIENTED_EDGE('',*,*,#11144,.F.);
#15809=ORIENTED_EDGE('',*,*,#11150,.T.);
#15810=ORIENTED_EDGE('',*,*,#11151,.T.);
#15811=ORIENTED_EDGE('',*,*,#11152,.F.);
#15812=ORIENTED_EDGE('',*,*,#11088,.T.);
#15813=ORIENTED_EDGE('',*,*,#11148,.F.);
#15814=ORIENTED_EDGE('',*,*,#11153,.T.);
#15815=ORIENTED_EDGE('',*,*,#11154,.T.);
#15816=ORIENTED_EDGE('',*,*,#11155,.T.);
#15817=ORIENTED_EDGE('',*,*,#11156,.T.);
#15818=ORIENTED_EDGE('',*,*,#11157,.T.);
#15819=ORIENTED_EDGE('',*,*,#11154,.F.);
#15820=ORIENTED_EDGE('',*,*,#11158,.F.);
#15821=ORIENTED_EDGE('',*,*,#11159,.F.);
#15822=ORIENTED_EDGE('',*,*,#11160,.F.);
#15823=ORIENTED_EDGE('',*,*,#11153,.F.);
#15824=ORIENTED_EDGE('',*,*,#11161,.T.);
#15825=ORIENTED_EDGE('',*,*,#11162,.T.);
#15826=ORIENTED_EDGE('',*,*,#11163,.T.);
#15827=ORIENTED_EDGE('',*,*,#11151,.F.);
#15828=ORIENTED_EDGE('',*,*,#11158,.T.);
#15829=ORIENTED_EDGE('',*,*,#11157,.F.);
#15830=ORIENTED_EDGE('',*,*,#11164,.T.);
#15831=ORIENTED_EDGE('',*,*,#11165,.T.);
#15832=ORIENTED_EDGE('',*,*,#11166,.F.);
#15833=ORIENTED_EDGE('',*,*,#11167,.T.);
#15834=ORIENTED_EDGE('',*,*,#11161,.F.);
#15835=ORIENTED_EDGE('',*,*,#11168,.T.);
#15836=ORIENTED_EDGE('',*,*,#11169,.T.);
#15837=ORIENTED_EDGE('',*,*,#11170,.T.);
#15838=ORIENTED_EDGE('',*,*,#11171,.T.);
#15839=ORIENTED_EDGE('',*,*,#11172,.T.);
#15840=ORIENTED_EDGE('',*,*,#11169,.F.);
#15841=ORIENTED_EDGE('',*,*,#11173,.F.);
#15842=ORIENTED_EDGE('',*,*,#11174,.F.);
#15843=ORIENTED_EDGE('',*,*,#11175,.F.);
#15844=ORIENTED_EDGE('',*,*,#11168,.F.);
#15845=ORIENTED_EDGE('',*,*,#11176,.T.);
#15846=ORIENTED_EDGE('',*,*,#11177,.T.);
#15847=ORIENTED_EDGE('',*,*,#11178,.T.);
#15848=ORIENTED_EDGE('',*,*,#11165,.F.);
#15849=ORIENTED_EDGE('',*,*,#11173,.T.);
#15850=ORIENTED_EDGE('',*,*,#11172,.F.);
#15851=ORIENTED_EDGE('',*,*,#11179,.T.);
#15852=ORIENTED_EDGE('',*,*,#11180,.T.);
#15853=ORIENTED_EDGE('',*,*,#11181,.F.);
#15854=ORIENTED_EDGE('',*,*,#11182,.T.);
#15855=ORIENTED_EDGE('',*,*,#11176,.F.);
#15856=ORIENTED_EDGE('',*,*,#11183,.T.);
#15857=ORIENTED_EDGE('',*,*,#11184,.T.);
#15858=ORIENTED_EDGE('',*,*,#11185,.T.);
#15859=ORIENTED_EDGE('',*,*,#11186,.T.);
#15860=ORIENTED_EDGE('',*,*,#11187,.T.);
#15861=ORIENTED_EDGE('',*,*,#11184,.F.);
#15862=ORIENTED_EDGE('',*,*,#11188,.F.);
#15863=ORIENTED_EDGE('',*,*,#11189,.F.);
#15864=ORIENTED_EDGE('',*,*,#11190,.F.);
#15865=ORIENTED_EDGE('',*,*,#11183,.F.);
#15866=ORIENTED_EDGE('',*,*,#11191,.T.);
#15867=ORIENTED_EDGE('',*,*,#11192,.T.);
#15868=ORIENTED_EDGE('',*,*,#11193,.T.);
#15869=ORIENTED_EDGE('',*,*,#11180,.F.);
#15870=ORIENTED_EDGE('',*,*,#11188,.T.);
#15871=ORIENTED_EDGE('',*,*,#11187,.F.);
#15872=ORIENTED_EDGE('',*,*,#11194,.T.);
#15873=ORIENTED_EDGE('',*,*,#11109,.T.);
#15874=ORIENTED_EDGE('',*,*,#11195,.F.);
#15875=ORIENTED_EDGE('',*,*,#11196,.T.);
#15876=ORIENTED_EDGE('',*,*,#11191,.F.);
#15877=ORIENTED_EDGE('',*,*,#11139,.F.);
#15878=ORIENTED_EDGE('',*,*,#11197,.T.);
#15879=ORIENTED_EDGE('',*,*,#11198,.T.);
#15880=ORIENTED_EDGE('',*,*,#11199,.F.);
#15881=ORIENTED_EDGE('',*,*,#11124,.F.);
#15882=ORIENTED_EDGE('',*,*,#11200,.T.);
#15883=ORIENTED_EDGE('',*,*,#11201,.T.);
#15884=ORIENTED_EDGE('',*,*,#11202,.F.);
#15885=ORIENTED_EDGE('',*,*,#11108,.F.);
#15886=ORIENTED_EDGE('',*,*,#11203,.T.);
#15887=ORIENTED_EDGE('',*,*,#11204,.T.);
#15888=ORIENTED_EDGE('',*,*,#11205,.F.);
#15889=ORIENTED_EDGE('',*,*,#11193,.F.);
#15890=ORIENTED_EDGE('',*,*,#11206,.T.);
#15891=ORIENTED_EDGE('',*,*,#11207,.T.);
#15892=ORIENTED_EDGE('',*,*,#11208,.F.);
#15893=ORIENTED_EDGE('',*,*,#11178,.F.);
#15894=ORIENTED_EDGE('',*,*,#11209,.T.);
#15895=ORIENTED_EDGE('',*,*,#11210,.T.);
#15896=ORIENTED_EDGE('',*,*,#11211,.F.);
#15897=ORIENTED_EDGE('',*,*,#11163,.F.);
#15898=ORIENTED_EDGE('',*,*,#11212,.T.);
#15899=ORIENTED_EDGE('',*,*,#11213,.T.);
#15900=ORIENTED_EDGE('',*,*,#11214,.F.);
#15901=ORIENTED_EDGE('',*,*,#11133,.F.);
#15902=ORIENTED_EDGE('',*,*,#11215,.T.);
#15903=ORIENTED_EDGE('',*,*,#11048,.F.);
#15904=ORIENTED_EDGE('',*,*,#11216,.F.);
#15905=ORIENTED_EDGE('',*,*,#11217,.T.);
#15906=ORIENTED_EDGE('',*,*,#11137,.T.);
#15907=ORIENTED_EDGE('',*,*,#11047,.F.);
#15908=ORIENTED_EDGE('',*,*,#11218,.T.);
#15909=ORIENTED_EDGE('',*,*,#11219,.T.);
#15910=ORIENTED_EDGE('',*,*,#11220,.T.);
#15911=ORIENTED_EDGE('',*,*,#11041,.F.);
#15912=ORIENTED_EDGE('',*,*,#11221,.T.);
#15913=ORIENTED_EDGE('',*,*,#11060,.F.);
#15914=ORIENTED_EDGE('',*,*,#11222,.F.);
#15915=ORIENTED_EDGE('',*,*,#11223,.T.);
#15916=ORIENTED_EDGE('',*,*,#11045,.T.);
#15917=ORIENTED_EDGE('',*,*,#11059,.F.);
#15918=ORIENTED_EDGE('',*,*,#11224,.T.);
#15919=ORIENTED_EDGE('',*,*,#11225,.T.);
#15920=ORIENTED_EDGE('',*,*,#11226,.T.);
#15921=ORIENTED_EDGE('',*,*,#11053,.F.);
#15922=ORIENTED_EDGE('',*,*,#11227,.T.);
#15923=ORIENTED_EDGE('',*,*,#11072,.F.);
#15924=ORIENTED_EDGE('',*,*,#11228,.F.);
#15925=ORIENTED_EDGE('',*,*,#11229,.T.);
#15926=ORIENTED_EDGE('',*,*,#11057,.T.);
#15927=ORIENTED_EDGE('',*,*,#11071,.F.);
#15928=ORIENTED_EDGE('',*,*,#11091,.T.);
#15929=ORIENTED_EDGE('',*,*,#11230,.T.);
#15930=ORIENTED_EDGE('',*,*,#11231,.T.);
#15931=ORIENTED_EDGE('',*,*,#11065,.F.);
#15932=ORIENTED_EDGE('',*,*,#11232,.T.);
#15933=ORIENTED_EDGE('',*,*,#11079,.T.);
#15934=ORIENTED_EDGE('',*,*,#11092,.T.);
#15935=ORIENTED_EDGE('',*,*,#11069,.T.);
#15936=ORIENTED_EDGE('',*,*,#11228,.T.);
#15937=ORIENTED_EDGE('',*,*,#11231,.F.);
#15938=ORIENTED_EDGE('',*,*,#11233,.T.);
#15939=ORIENTED_EDGE('',*,*,#11234,.T.);
#15940=ORIENTED_EDGE('',*,*,#11222,.T.);
#15941=ORIENTED_EDGE('',*,*,#11226,.F.);
#15942=ORIENTED_EDGE('',*,*,#11235,.T.);
#15943=ORIENTED_EDGE('',*,*,#11236,.T.);
#15944=ORIENTED_EDGE('',*,*,#11216,.T.);
#15945=ORIENTED_EDGE('',*,*,#11220,.F.);
#15946=ORIENTED_EDGE('',*,*,#11237,.T.);
#15947=ORIENTED_EDGE('',*,*,#11238,.T.);
#15948=ORIENTED_EDGE('',*,*,#11152,.T.);
#15949=ORIENTED_EDGE('',*,*,#11214,.T.);
#15950=ORIENTED_EDGE('',*,*,#11239,.T.);
#15951=ORIENTED_EDGE('',*,*,#11089,.T.);
#15952=ORIENTED_EDGE('',*,*,#11166,.T.);
#15953=ORIENTED_EDGE('',*,*,#11211,.T.);
#15954=ORIENTED_EDGE('',*,*,#11240,.T.);
#15955=ORIENTED_EDGE('',*,*,#11241,.T.);
#15956=ORIENTED_EDGE('',*,*,#11181,.T.);
#15957=ORIENTED_EDGE('',*,*,#11208,.T.);
#15958=ORIENTED_EDGE('',*,*,#11242,.T.);
#15959=ORIENTED_EDGE('',*,*,#11243,.T.);
#15960=ORIENTED_EDGE('',*,*,#11195,.T.);
#15961=ORIENTED_EDGE('',*,*,#11205,.T.);
#15962=ORIENTED_EDGE('',*,*,#11244,.T.);
#15963=ORIENTED_EDGE('',*,*,#11245,.T.);
#15964=ORIENTED_EDGE('',*,*,#11112,.T.);
#15965=ORIENTED_EDGE('',*,*,#11202,.T.);
#15966=ORIENTED_EDGE('',*,*,#11246,.T.);
#15967=ORIENTED_EDGE('',*,*,#11247,.T.);
#15968=ORIENTED_EDGE('',*,*,#11127,.T.);
#15969=ORIENTED_EDGE('',*,*,#11199,.T.);
#15970=ORIENTED_EDGE('',*,*,#11248,.T.);
#15971=ORIENTED_EDGE('',*,*,#11249,.T.);
#15972=ORIENTED_EDGE('',*,*,#11186,.F.);
#15973=ORIENTED_EDGE('',*,*,#11250,.F.);
#15974=ORIENTED_EDGE('',*,*,#11104,.T.);
#15975=ORIENTED_EDGE('',*,*,#11194,.F.);
#15976=ORIENTED_EDGE('',*,*,#11171,.F.);
#15977=ORIENTED_EDGE('',*,*,#11251,.F.);
#15978=ORIENTED_EDGE('',*,*,#11189,.T.);
#15979=ORIENTED_EDGE('',*,*,#11179,.F.);
#15980=ORIENTED_EDGE('',*,*,#11156,.F.);
#15981=ORIENTED_EDGE('',*,*,#11252,.F.);
#15982=ORIENTED_EDGE('',*,*,#11174,.T.);
#15983=ORIENTED_EDGE('',*,*,#11164,.F.);
#15984=ORIENTED_EDGE('',*,*,#11143,.F.);
#15985=ORIENTED_EDGE('',*,*,#11253,.F.);
#15986=ORIENTED_EDGE('',*,*,#11159,.T.);
#15987=ORIENTED_EDGE('',*,*,#11150,.F.);
#15988=ORIENTED_EDGE('',*,*,#11239,.F.);
#15989=ORIENTED_EDGE('',*,*,#11213,.F.);
#15990=ORIENTED_EDGE('',*,*,#11254,.T.);
#15991=ORIENTED_EDGE('',*,*,#11240,.F.);
#15992=ORIENTED_EDGE('',*,*,#11210,.F.);
#15993=ORIENTED_EDGE('',*,*,#11255,.T.);
#15994=ORIENTED_EDGE('',*,*,#11242,.F.);
#15995=ORIENTED_EDGE('',*,*,#11207,.F.);
#15996=ORIENTED_EDGE('',*,*,#11256,.T.);
#15997=ORIENTED_EDGE('',*,*,#11244,.F.);
#15998=ORIENTED_EDGE('',*,*,#11204,.F.);
#15999=ORIENTED_EDGE('',*,*,#11257,.T.);
#16000=ORIENTED_EDGE('',*,*,#11246,.F.);
#16001=ORIENTED_EDGE('',*,*,#11201,.F.);
#16002=ORIENTED_EDGE('',*,*,#11258,.T.);
#16003=ORIENTED_EDGE('',*,*,#11248,.F.);
#16004=ORIENTED_EDGE('',*,*,#11198,.F.);
#16005=ORIENTED_EDGE('',*,*,#11259,.T.);
#16006=ORIENTED_EDGE('',*,*,#11237,.F.);
#16007=ORIENTED_EDGE('',*,*,#11219,.F.);
#16008=ORIENTED_EDGE('',*,*,#11260,.T.);
#16009=ORIENTED_EDGE('',*,*,#11235,.F.);
#16010=ORIENTED_EDGE('',*,*,#11225,.F.);
#16011=ORIENTED_EDGE('',*,*,#11261,.T.);
#16012=ORIENTED_EDGE('',*,*,#11233,.F.);
#16013=ORIENTED_EDGE('',*,*,#11230,.F.);
#16014=ORIENTED_EDGE('',*,*,#11090,.T.);
#16015=ORIENTED_EDGE('',*,*,#11262,.T.);
#16016=ORIENTED_EDGE('',*,*,#11162,.F.);
#16017=ORIENTED_EDGE('',*,*,#11167,.F.);
#16018=ORIENTED_EDGE('',*,*,#11241,.F.);
#16019=ORIENTED_EDGE('',*,*,#11254,.F.);
#16020=ORIENTED_EDGE('',*,*,#11212,.F.);
#16021=ORIENTED_EDGE('',*,*,#11177,.F.);
#16022=ORIENTED_EDGE('',*,*,#11182,.F.);
#16023=ORIENTED_EDGE('',*,*,#11243,.F.);
#16024=ORIENTED_EDGE('',*,*,#11255,.F.);
#16025=ORIENTED_EDGE('',*,*,#11209,.F.);
#16026=ORIENTED_EDGE('',*,*,#11192,.F.);
#16027=ORIENTED_EDGE('',*,*,#11196,.F.);
#16028=ORIENTED_EDGE('',*,*,#11245,.F.);
#16029=ORIENTED_EDGE('',*,*,#11256,.F.);
#16030=ORIENTED_EDGE('',*,*,#11206,.F.);
#16031=ORIENTED_EDGE('',*,*,#11107,.F.);
#16032=ORIENTED_EDGE('',*,*,#11113,.F.);
#16033=ORIENTED_EDGE('',*,*,#11247,.F.);
#16034=ORIENTED_EDGE('',*,*,#11257,.F.);
#16035=ORIENTED_EDGE('',*,*,#11203,.F.);
#16036=ORIENTED_EDGE('',*,*,#11249,.F.);
#16037=ORIENTED_EDGE('',*,*,#11258,.F.);
#16038=ORIENTED_EDGE('',*,*,#11200,.F.);
#16039=ORIENTED_EDGE('',*,*,#11123,.F.);
#16040=ORIENTED_EDGE('',*,*,#11128,.F.);
#16041=ORIENTED_EDGE('',*,*,#11238,.F.);
#16042=ORIENTED_EDGE('',*,*,#11259,.F.);
#16043=ORIENTED_EDGE('',*,*,#11197,.F.);
#16044=ORIENTED_EDGE('',*,*,#11138,.F.);
#16045=ORIENTED_EDGE('',*,*,#11217,.F.);
#16046=ORIENTED_EDGE('',*,*,#11236,.F.);
#16047=ORIENTED_EDGE('',*,*,#11260,.F.);
#16048=ORIENTED_EDGE('',*,*,#11218,.F.);
#16049=ORIENTED_EDGE('',*,*,#11046,.F.);
#16050=ORIENTED_EDGE('',*,*,#11223,.F.);
#16051=ORIENTED_EDGE('',*,*,#11234,.F.);
#16052=ORIENTED_EDGE('',*,*,#11261,.F.);
#16053=ORIENTED_EDGE('',*,*,#11224,.F.);
#16054=ORIENTED_EDGE('',*,*,#11058,.F.);
#16055=ORIENTED_EDGE('',*,*,#11229,.F.);
#16056=ORIENTED_EDGE('',*,*,#11263,.F.);
#16057=ORIENTED_EDGE('',*,*,#11264,.T.);
#16058=ORIENTED_EDGE('',*,*,#11262,.F.);
#16059=ORIENTED_EDGE('',*,*,#11264,.F.);
#16060=ORIENTED_EDGE('',*,*,#11265,.F.);
#16061=ORIENTED_EDGE('',*,*,#11266,.T.);
#16062=ORIENTED_EDGE('',*,*,#11267,.F.);
#16063=ORIENTED_EDGE('',*,*,#11266,.F.);
#16064=ORIENTED_EDGE('',*,*,#11117,.F.);
#16065=ORIENTED_EDGE('',*,*,#11268,.F.);
#16066=ORIENTED_EDGE('',*,*,#11135,.T.);
#16067=ORIENTED_EDGE('',*,*,#11125,.F.);
#16068=ORIENTED_EDGE('',*,*,#11101,.F.);
#16069=ORIENTED_EDGE('',*,*,#11269,.F.);
#16070=ORIENTED_EDGE('',*,*,#11120,.T.);
#16071=ORIENTED_EDGE('',*,*,#11110,.F.);
#16072=ORIENTED_EDGE('',*,*,#11095,.F.);
#16073=ORIENTED_EDGE('',*,*,#11270,.F.);
#16074=ORIENTED_EDGE('',*,*,#11146,.T.);
#16075=ORIENTED_EDGE('',*,*,#11149,.F.);
#16076=ORIENTED_EDGE('',*,*,#11086,.T.);
#16077=ORIENTED_EDGE('',*,*,#11085,.T.);
#16078=ORIENTED_EDGE('',*,*,#11076,.F.);
#16079=ORIENTED_EDGE('',*,*,#11271,.F.);
#16080=ORIENTED_EDGE('',*,*,#11096,.T.);
#16081=ORIENTED_EDGE('',*,*,#11082,.T.);
#16082=ORIENTED_EDGE('',*,*,#11064,.F.);
#16083=ORIENTED_EDGE('',*,*,#11272,.F.);
#16084=ORIENTED_EDGE('',*,*,#11080,.T.);
#16085=ORIENTED_EDGE('',*,*,#11232,.F.);
#16086=ORIENTED_EDGE('',*,*,#11052,.F.);
#16087=ORIENTED_EDGE('',*,*,#11273,.F.);
#16088=ORIENTED_EDGE('',*,*,#11067,.T.);
#16089=ORIENTED_EDGE('',*,*,#11227,.F.);
#16090=ORIENTED_EDGE('',*,*,#11040,.F.);
#16091=ORIENTED_EDGE('',*,*,#11274,.F.);
#16092=ORIENTED_EDGE('',*,*,#11055,.T.);
#16093=ORIENTED_EDGE('',*,*,#11221,.F.);
#16094=ORIENTED_EDGE('',*,*,#11132,.F.);
#16095=ORIENTED_EDGE('',*,*,#11275,.F.);
#16096=ORIENTED_EDGE('',*,*,#11043,.T.);
#16097=ORIENTED_EDGE('',*,*,#11215,.F.);
#16098=ORIENTED_EDGE('',*,*,#11263,.T.);
#16099=ORIENTED_EDGE('',*,*,#11276,.T.);
#16100=ORIENTED_EDGE('',*,*,#11267,.T.);
#16101=ORIENTED_EDGE('',*,*,#11276,.F.);
#16102=ORIENTED_EDGE('',*,*,#11277,.F.);
#16103=ORIENTED_EDGE('',*,*,#11265,.T.);
#16104=ORIENTED_EDGE('',*,*,#11278,.F.);
#16105=ORIENTED_EDGE('',*,*,#11279,.T.);
#16106=ORIENTED_EDGE('',*,*,#11277,.T.);
#16107=ORIENTED_EDGE('',*,*,#11279,.F.);
#16108=ORIENTED_EDGE('',*,*,#11280,.F.);
#16109=ORIENTED_EDGE('',*,*,#11281,.T.);
#16110=ORIENTED_EDGE('',*,*,#11278,.T.);
#16111=ORIENTED_EDGE('',*,*,#11281,.F.);
#16112=ORIENTED_EDGE('',*,*,#11282,.F.);
#16113=ORIENTED_EDGE('',*,*,#11283,.T.);
#16114=ORIENTED_EDGE('',*,*,#11280,.T.);
#16115=ORIENTED_EDGE('',*,*,#11283,.F.);
#16116=ORIENTED_EDGE('',*,*,#11282,.T.);
#16117=ORIENTED_EDGE('',*,*,#11268,.T.);
#16118=ORIENTED_EDGE('',*,*,#11116,.F.);
#16119=ORIENTED_EDGE('',*,*,#11121,.T.);
#16120=ORIENTED_EDGE('',*,*,#11269,.T.);
#16121=ORIENTED_EDGE('',*,*,#11100,.F.);
#16122=ORIENTED_EDGE('',*,*,#11105,.T.);
#16123=ORIENTED_EDGE('',*,*,#11250,.T.);
#16124=ORIENTED_EDGE('',*,*,#11185,.F.);
#16125=ORIENTED_EDGE('',*,*,#11190,.T.);
#16126=ORIENTED_EDGE('',*,*,#11251,.T.);
#16127=ORIENTED_EDGE('',*,*,#11170,.F.);
#16128=ORIENTED_EDGE('',*,*,#11175,.T.);
#16129=ORIENTED_EDGE('',*,*,#11252,.T.);
#16130=ORIENTED_EDGE('',*,*,#11155,.F.);
#16131=ORIENTED_EDGE('',*,*,#11160,.T.);
#16132=ORIENTED_EDGE('',*,*,#11253,.T.);
#16133=ORIENTED_EDGE('',*,*,#11142,.F.);
#16134=ORIENTED_EDGE('',*,*,#11147,.T.);
#16135=ORIENTED_EDGE('',*,*,#11270,.T.);
#16136=ORIENTED_EDGE('',*,*,#11094,.F.);
#16137=ORIENTED_EDGE('',*,*,#11097,.T.);
#16138=ORIENTED_EDGE('',*,*,#11271,.T.);
#16139=ORIENTED_EDGE('',*,*,#11075,.F.);
#16140=ORIENTED_EDGE('',*,*,#11081,.T.);
#16141=ORIENTED_EDGE('',*,*,#11272,.T.);
#16142=ORIENTED_EDGE('',*,*,#11063,.F.);
#16143=ORIENTED_EDGE('',*,*,#11068,.T.);
#16144=ORIENTED_EDGE('',*,*,#11273,.T.);
#16145=ORIENTED_EDGE('',*,*,#11051,.F.);
#16146=ORIENTED_EDGE('',*,*,#11056,.T.);
#16147=ORIENTED_EDGE('',*,*,#11274,.T.);
#16148=ORIENTED_EDGE('',*,*,#11039,.F.);
#16149=ORIENTED_EDGE('',*,*,#11044,.T.);
#16150=ORIENTED_EDGE('',*,*,#11275,.T.);
#16151=ORIENTED_EDGE('',*,*,#11131,.F.);
#16152=ORIENTED_EDGE('',*,*,#11136,.T.);
#16153=ORIENTED_EDGE('',*,*,#11284,.F.);
#16154=ORIENTED_EDGE('',*,*,#11285,.T.);
#16155=ORIENTED_EDGE('',*,*,#11286,.F.);
#16156=ORIENTED_EDGE('',*,*,#11287,.T.);
#16157=ORIENTED_EDGE('',*,*,#11288,.F.);
#16158=ORIENTED_EDGE('',*,*,#11285,.F.);
#16159=ORIENTED_EDGE('',*,*,#11289,.F.);
#16160=ORIENTED_EDGE('',*,*,#11287,.F.);
#16161=ORIENTED_EDGE('',*,*,#11290,.F.);
#16162=ORIENTED_EDGE('',*,*,#11291,.T.);
#16163=ORIENTED_EDGE('',*,*,#11292,.F.);
#16164=ORIENTED_EDGE('',*,*,#11293,.T.);
#16165=ORIENTED_EDGE('',*,*,#11294,.F.);
#16166=ORIENTED_EDGE('',*,*,#11291,.F.);
#16167=ORIENTED_EDGE('',*,*,#11295,.F.);
#16168=ORIENTED_EDGE('',*,*,#11293,.F.);
#16169=ORIENTED_EDGE('',*,*,#11296,.F.);
#16170=ORIENTED_EDGE('',*,*,#11297,.T.);
#16171=ORIENTED_EDGE('',*,*,#11298,.F.);
#16172=ORIENTED_EDGE('',*,*,#11299,.T.);
#16173=ORIENTED_EDGE('',*,*,#11300,.F.);
#16174=ORIENTED_EDGE('',*,*,#11297,.F.);
#16175=ORIENTED_EDGE('',*,*,#11301,.F.);
#16176=ORIENTED_EDGE('',*,*,#11299,.F.);
#16177=ORIENTED_EDGE('',*,*,#11302,.F.);
#16178=ORIENTED_EDGE('',*,*,#11303,.T.);
#16179=ORIENTED_EDGE('',*,*,#11304,.F.);
#16180=ORIENTED_EDGE('',*,*,#11305,.T.);
#16181=ORIENTED_EDGE('',*,*,#11306,.F.);
#16182=ORIENTED_EDGE('',*,*,#11303,.F.);
#16183=ORIENTED_EDGE('',*,*,#11307,.F.);
#16184=ORIENTED_EDGE('',*,*,#11305,.F.);
#16185=ORIENTED_EDGE('',*,*,#11308,.F.);
#16186=ORIENTED_EDGE('',*,*,#11309,.F.);
#16187=ORIENTED_EDGE('',*,*,#11310,.T.);
#16188=ORIENTED_EDGE('',*,*,#11311,.F.);
#16189=ORIENTED_EDGE('',*,*,#11312,.F.);
#16190=ORIENTED_EDGE('',*,*,#11310,.F.);
#16191=ORIENTED_EDGE('',*,*,#11313,.F.);
#16192=ORIENTED_EDGE('',*,*,#11314,.F.);
#16193=ORIENTED_EDGE('',*,*,#11315,.T.);
#16194=ORIENTED_EDGE('',*,*,#11316,.F.);
#16195=ORIENTED_EDGE('',*,*,#11317,.F.);
#16196=ORIENTED_EDGE('',*,*,#11315,.F.);
#16197=ORIENTED_EDGE('',*,*,#11318,.F.);
#16198=ORIENTED_EDGE('',*,*,#11319,.F.);
#16199=ORIENTED_EDGE('',*,*,#11320,.T.);
#16200=ORIENTED_EDGE('',*,*,#11321,.F.);
#16201=ORIENTED_EDGE('',*,*,#11322,.F.);
#16202=ORIENTED_EDGE('',*,*,#11323,.F.);
#16203=ORIENTED_EDGE('',*,*,#11320,.F.);
#16204=ORIENTED_EDGE('',*,*,#11324,.F.);
#16205=ORIENTED_EDGE('',*,*,#11325,.F.);
#16206=ORIENTED_EDGE('',*,*,#11326,.T.);
#16207=ORIENTED_EDGE('',*,*,#11327,.F.);
#16208=ORIENTED_EDGE('',*,*,#11328,.F.);
#16209=ORIENTED_EDGE('',*,*,#11326,.F.);
#16210=ORIENTED_EDGE('',*,*,#11329,.T.);
#16211=ORIENTED_EDGE('',*,*,#11330,.T.);
#16212=ORIENTED_EDGE('',*,*,#11319,.T.);
#16213=ORIENTED_EDGE('',*,*,#11331,.T.);
#16214=ORIENTED_EDGE('',*,*,#11332,.F.);
#16215=ORIENTED_EDGE('',*,*,#11331,.F.);
#16216=ORIENTED_EDGE('',*,*,#11318,.T.);
#16217=ORIENTED_EDGE('',*,*,#11330,.F.);
#16218=ORIENTED_EDGE('',*,*,#11308,.T.);
#16219=ORIENTED_EDGE('',*,*,#11309,.T.);
#16220=ORIENTED_EDGE('',*,*,#11313,.T.);
#16221=ORIENTED_EDGE('',*,*,#11314,.T.);
#16222=ORIENTED_EDGE('',*,*,#11324,.T.);
#16223=ORIENTED_EDGE('',*,*,#11325,.T.);
#16224=ORIENTED_EDGE('',*,*,#11333,.F.);
#16225=ORIENTED_EDGE('',*,*,#11329,.F.);
#16226=ORIENTED_EDGE('',*,*,#11334,.F.);
#16227=ORIENTED_EDGE('',*,*,#11332,.T.);
#16228=ORIENTED_EDGE('',*,*,#11335,.F.);
#16229=ORIENTED_EDGE('',*,*,#11336,.T.);
#16230=ORIENTED_EDGE('',*,*,#11334,.T.);
#16231=ORIENTED_EDGE('',*,*,#11336,.F.);
#16232=ORIENTED_EDGE('',*,*,#11337,.F.);
#16233=ORIENTED_EDGE('',*,*,#11338,.T.);
#16234=ORIENTED_EDGE('',*,*,#11339,.T.);
#16235=ORIENTED_EDGE('',*,*,#11338,.F.);
#16236=ORIENTED_EDGE('',*,*,#11333,.T.);
#16237=ORIENTED_EDGE('',*,*,#11340,.T.);
#16238=ORIENTED_EDGE('',*,*,#11337,.T.);
#16239=ORIENTED_EDGE('',*,*,#11340,.F.);
#16240=ORIENTED_EDGE('',*,*,#11341,.F.);
#16241=ORIENTED_EDGE('',*,*,#11342,.T.);
#16242=ORIENTED_EDGE('',*,*,#11335,.T.);
#16243=ORIENTED_EDGE('',*,*,#11342,.F.);
#16244=ORIENTED_EDGE('',*,*,#11341,.T.);
#16245=ORIENTED_EDGE('',*,*,#11343,.F.);
#16246=ORIENTED_EDGE('',*,*,#11343,.T.);
#16247=ORIENTED_EDGE('',*,*,#11344,.T.);
#16248=ORIENTED_EDGE('',*,*,#11345,.F.);
#16249=ORIENTED_EDGE('',*,*,#11344,.F.);
#16250=ORIENTED_EDGE('',*,*,#11345,.T.);
#16251=ORIENTED_EDGE('',*,*,#11346,.T.);
#16252=ORIENTED_EDGE('',*,*,#11322,.T.);
#16253=ORIENTED_EDGE('',*,*,#11321,.T.);
#16254=ORIENTED_EDGE('',*,*,#11347,.T.);
#16255=ORIENTED_EDGE('',*,*,#11348,.F.);
#16256=ORIENTED_EDGE('',*,*,#11347,.F.);
#16257=ORIENTED_EDGE('',*,*,#11323,.T.);
#16258=ORIENTED_EDGE('',*,*,#11346,.F.);
#16259=ORIENTED_EDGE('',*,*,#11288,.T.);
#16260=ORIENTED_EDGE('',*,*,#11289,.T.);
#16261=ORIENTED_EDGE('',*,*,#11286,.T.);
#16262=ORIENTED_EDGE('',*,*,#11284,.T.);
#16263=ORIENTED_EDGE('',*,*,#11294,.T.);
#16264=ORIENTED_EDGE('',*,*,#11295,.T.);
#16265=ORIENTED_EDGE('',*,*,#11292,.T.);
#16266=ORIENTED_EDGE('',*,*,#11290,.T.);
#16267=ORIENTED_EDGE('',*,*,#11300,.T.);
#16268=ORIENTED_EDGE('',*,*,#11301,.T.);
#16269=ORIENTED_EDGE('',*,*,#11298,.T.);
#16270=ORIENTED_EDGE('',*,*,#11296,.T.);
#16271=ORIENTED_EDGE('',*,*,#11306,.T.);
#16272=ORIENTED_EDGE('',*,*,#11307,.T.);
#16273=ORIENTED_EDGE('',*,*,#11304,.T.);
#16274=ORIENTED_EDGE('',*,*,#11302,.T.);
#16275=ORIENTED_EDGE('',*,*,#11311,.T.);
#16276=ORIENTED_EDGE('',*,*,#11312,.T.);
#16277=ORIENTED_EDGE('',*,*,#11316,.T.);
#16278=ORIENTED_EDGE('',*,*,#11317,.T.);
#16279=ORIENTED_EDGE('',*,*,#11327,.T.);
#16280=ORIENTED_EDGE('',*,*,#11328,.T.);
#16281=ORIENTED_EDGE('',*,*,#11348,.T.);
#16282=ORIENTED_EDGE('',*,*,#11349,.T.);
#16283=ORIENTED_EDGE('',*,*,#11350,.F.);
#16284=ORIENTED_EDGE('',*,*,#11349,.F.);
#16285=ORIENTED_EDGE('',*,*,#11339,.F.);
#16286=ORIENTED_EDGE('',*,*,#11350,.T.);
#16287=ORIENTED_EDGE('',*,*,#11351,.T.);
#16288=ORIENTED_EDGE('',*,*,#11352,.T.);
#16289=ORIENTED_EDGE('',*,*,#11353,.T.);
#16290=ORIENTED_EDGE('',*,*,#11352,.F.);
#16291=ORIENTED_EDGE('',*,*,#11353,.F.);
#16292=ORIENTED_EDGE('',*,*,#11354,.T.);
#16293=ORIENTED_EDGE('',*,*,#11355,.F.);
#16294=ORIENTED_EDGE('',*,*,#11354,.F.);
#16295=ORIENTED_EDGE('',*,*,#11356,.F.);
#16296=ORIENTED_EDGE('',*,*,#11357,.F.);
#16297=ORIENTED_EDGE('',*,*,#11358,.F.);
#16298=ORIENTED_EDGE('',*,*,#11359,.F.);
#16299=ORIENTED_EDGE('',*,*,#11360,.F.);
#16300=ORIENTED_EDGE('',*,*,#11361,.F.);
#16301=ORIENTED_EDGE('',*,*,#11362,.F.);
#16302=ORIENTED_EDGE('',*,*,#11363,.F.);
#16303=ORIENTED_EDGE('',*,*,#11364,.F.);
#16304=ORIENTED_EDGE('',*,*,#11365,.F.);
#16305=ORIENTED_EDGE('',*,*,#11366,.F.);
#16306=ORIENTED_EDGE('',*,*,#11367,.F.);
#16307=ORIENTED_EDGE('',*,*,#11368,.F.);
#16308=ORIENTED_EDGE('',*,*,#11369,.F.);
#16309=ORIENTED_EDGE('',*,*,#11370,.F.);
#16310=ORIENTED_EDGE('',*,*,#11371,.F.);
#16311=ORIENTED_EDGE('',*,*,#11372,.F.);
#16312=ORIENTED_EDGE('',*,*,#11373,.F.);
#16313=ORIENTED_EDGE('',*,*,#11374,.F.);
#16314=ORIENTED_EDGE('',*,*,#11375,.F.);
#16315=ORIENTED_EDGE('',*,*,#11376,.F.);
#16316=ORIENTED_EDGE('',*,*,#11377,.F.);
#16317=ORIENTED_EDGE('',*,*,#11378,.F.);
#16318=ORIENTED_EDGE('',*,*,#11379,.F.);
#16319=ORIENTED_EDGE('',*,*,#11380,.F.);
#16320=ORIENTED_EDGE('',*,*,#11381,.F.);
#16321=ORIENTED_EDGE('',*,*,#11382,.F.);
#16322=ORIENTED_EDGE('',*,*,#11383,.F.);
#16323=ORIENTED_EDGE('',*,*,#11384,.F.);
#16324=ORIENTED_EDGE('',*,*,#11385,.F.);
#16325=ORIENTED_EDGE('',*,*,#11386,.F.);
#16326=ORIENTED_EDGE('',*,*,#11387,.F.);
#16327=ORIENTED_EDGE('',*,*,#11388,.F.);
#16328=ORIENTED_EDGE('',*,*,#11389,.F.);
#16329=ORIENTED_EDGE('',*,*,#11390,.F.);
#16330=ORIENTED_EDGE('',*,*,#11391,.F.);
#16331=ORIENTED_EDGE('',*,*,#11392,.F.);
#16332=ORIENTED_EDGE('',*,*,#11393,.F.);
#16333=ORIENTED_EDGE('',*,*,#11394,.F.);
#16334=ORIENTED_EDGE('',*,*,#11395,.F.);
#16335=ORIENTED_EDGE('',*,*,#11396,.F.);
#16336=ORIENTED_EDGE('',*,*,#11397,.F.);
#16337=ORIENTED_EDGE('',*,*,#11398,.F.);
#16338=ORIENTED_EDGE('',*,*,#11399,.F.);
#16339=ORIENTED_EDGE('',*,*,#11400,.F.);
#16340=ORIENTED_EDGE('',*,*,#11401,.F.);
#16341=ORIENTED_EDGE('',*,*,#11402,.F.);
#16342=ORIENTED_EDGE('',*,*,#11403,.F.);
#16343=ORIENTED_EDGE('',*,*,#11404,.F.);
#16344=ORIENTED_EDGE('',*,*,#11405,.F.);
#16345=ORIENTED_EDGE('',*,*,#11406,.F.);
#16346=ORIENTED_EDGE('',*,*,#11407,.F.);
#16347=ORIENTED_EDGE('',*,*,#11408,.F.);
#16348=ORIENTED_EDGE('',*,*,#11409,.F.);
#16349=ORIENTED_EDGE('',*,*,#11410,.F.);
#16350=ORIENTED_EDGE('',*,*,#11411,.F.);
#16351=ORIENTED_EDGE('',*,*,#11412,.F.);
#16352=ORIENTED_EDGE('',*,*,#11413,.F.);
#16353=ORIENTED_EDGE('',*,*,#11414,.F.);
#16354=ORIENTED_EDGE('',*,*,#11415,.F.);
#16355=ORIENTED_EDGE('',*,*,#11416,.F.);
#16356=ORIENTED_EDGE('',*,*,#11417,.F.);
#16357=ORIENTED_EDGE('',*,*,#11418,.F.);
#16358=ORIENTED_EDGE('',*,*,#11419,.F.);
#16359=ORIENTED_EDGE('',*,*,#11420,.F.);
#16360=ORIENTED_EDGE('',*,*,#11421,.F.);
#16361=ORIENTED_EDGE('',*,*,#11422,.F.);
#16362=ORIENTED_EDGE('',*,*,#11423,.F.);
#16363=ORIENTED_EDGE('',*,*,#11424,.F.);
#16364=ORIENTED_EDGE('',*,*,#11425,.F.);
#16365=ORIENTED_EDGE('',*,*,#11426,.F.);
#16366=ORIENTED_EDGE('',*,*,#11427,.F.);
#16367=ORIENTED_EDGE('',*,*,#11428,.F.);
#16368=ORIENTED_EDGE('',*,*,#11429,.F.);
#16369=ORIENTED_EDGE('',*,*,#11430,.F.);
#16370=ORIENTED_EDGE('',*,*,#11431,.F.);
#16371=ORIENTED_EDGE('',*,*,#11432,.F.);
#16372=ORIENTED_EDGE('',*,*,#11433,.F.);
#16373=ORIENTED_EDGE('',*,*,#11434,.F.);
#16374=ORIENTED_EDGE('',*,*,#11435,.F.);
#16375=ORIENTED_EDGE('',*,*,#11436,.F.);
#16376=ORIENTED_EDGE('',*,*,#11437,.F.);
#16377=ORIENTED_EDGE('',*,*,#11438,.F.);
#16378=ORIENTED_EDGE('',*,*,#11439,.F.);
#16379=ORIENTED_EDGE('',*,*,#11440,.F.);
#16380=ORIENTED_EDGE('',*,*,#11441,.F.);
#16381=ORIENTED_EDGE('',*,*,#11442,.F.);
#16382=ORIENTED_EDGE('',*,*,#11443,.F.);
#16383=ORIENTED_EDGE('',*,*,#11444,.F.);
#16384=ORIENTED_EDGE('',*,*,#11445,.F.);
#16385=ORIENTED_EDGE('',*,*,#11446,.F.);
#16386=ORIENTED_EDGE('',*,*,#11447,.F.);
#16387=ORIENTED_EDGE('',*,*,#11448,.F.);
#16388=ORIENTED_EDGE('',*,*,#11449,.F.);
#16389=ORIENTED_EDGE('',*,*,#11450,.F.);
#16390=ORIENTED_EDGE('',*,*,#11451,.F.);
#16391=ORIENTED_EDGE('',*,*,#11452,.F.);
#16392=ORIENTED_EDGE('',*,*,#11453,.F.);
#16393=ORIENTED_EDGE('',*,*,#11454,.F.);
#16394=ORIENTED_EDGE('',*,*,#11455,.F.);
#16395=ORIENTED_EDGE('',*,*,#11456,.F.);
#16396=ORIENTED_EDGE('',*,*,#11457,.F.);
#16397=ORIENTED_EDGE('',*,*,#11458,.F.);
#16398=ORIENTED_EDGE('',*,*,#11459,.F.);
#16399=ORIENTED_EDGE('',*,*,#11460,.F.);
#16400=ORIENTED_EDGE('',*,*,#11461,.F.);
#16401=ORIENTED_EDGE('',*,*,#11462,.F.);
#16402=ORIENTED_EDGE('',*,*,#11463,.F.);
#16403=ORIENTED_EDGE('',*,*,#11464,.F.);
#16404=ORIENTED_EDGE('',*,*,#11465,.F.);
#16405=ORIENTED_EDGE('',*,*,#11466,.F.);
#16406=ORIENTED_EDGE('',*,*,#11467,.F.);
#16407=ORIENTED_EDGE('',*,*,#11468,.F.);
#16408=ORIENTED_EDGE('',*,*,#11469,.F.);
#16409=ORIENTED_EDGE('',*,*,#11470,.F.);
#16410=ORIENTED_EDGE('',*,*,#11471,.F.);
#16411=ORIENTED_EDGE('',*,*,#11472,.F.);
#16412=ORIENTED_EDGE('',*,*,#11473,.F.);
#16413=ORIENTED_EDGE('',*,*,#11474,.F.);
#16414=ORIENTED_EDGE('',*,*,#11475,.F.);
#16415=ORIENTED_EDGE('',*,*,#11476,.F.);
#16416=ORIENTED_EDGE('',*,*,#11477,.F.);
#16417=ORIENTED_EDGE('',*,*,#11478,.F.);
#16418=ORIENTED_EDGE('',*,*,#11479,.F.);
#16419=ORIENTED_EDGE('',*,*,#11480,.F.);
#16420=ORIENTED_EDGE('',*,*,#11481,.F.);
#16421=ORIENTED_EDGE('',*,*,#11482,.F.);
#16422=ORIENTED_EDGE('',*,*,#11483,.F.);
#16423=ORIENTED_EDGE('',*,*,#11484,.F.);
#16424=ORIENTED_EDGE('',*,*,#11485,.F.);
#16425=ORIENTED_EDGE('',*,*,#11486,.F.);
#16426=ORIENTED_EDGE('',*,*,#11487,.F.);
#16427=ORIENTED_EDGE('',*,*,#11488,.F.);
#16428=ORIENTED_EDGE('',*,*,#11489,.F.);
#16429=ORIENTED_EDGE('',*,*,#11490,.F.);
#16430=ORIENTED_EDGE('',*,*,#11491,.F.);
#16431=ORIENTED_EDGE('',*,*,#11492,.F.);
#16432=ORIENTED_EDGE('',*,*,#11493,.F.);
#16433=ORIENTED_EDGE('',*,*,#11494,.F.);
#16434=ORIENTED_EDGE('',*,*,#11495,.F.);
#16435=ORIENTED_EDGE('',*,*,#11496,.F.);
#16436=ORIENTED_EDGE('',*,*,#11497,.F.);
#16437=ORIENTED_EDGE('',*,*,#11498,.F.);
#16438=ORIENTED_EDGE('',*,*,#11499,.F.);
#16439=ORIENTED_EDGE('',*,*,#11500,.F.);
#16440=ORIENTED_EDGE('',*,*,#11501,.F.);
#16441=ORIENTED_EDGE('',*,*,#11502,.F.);
#16442=ORIENTED_EDGE('',*,*,#11503,.F.);
#16443=ORIENTED_EDGE('',*,*,#11504,.F.);
#16444=ORIENTED_EDGE('',*,*,#11505,.F.);
#16445=ORIENTED_EDGE('',*,*,#11506,.F.);
#16446=ORIENTED_EDGE('',*,*,#11351,.F.);
#16447=ORIENTED_EDGE('',*,*,#11507,.T.);
#16448=ORIENTED_EDGE('',*,*,#11508,.T.);
#16449=ORIENTED_EDGE('',*,*,#11355,.T.);
#16450=ORIENTED_EDGE('',*,*,#11508,.F.);
#16451=ORIENTED_EDGE('',*,*,#11509,.T.);
#16452=ORIENTED_EDGE('',*,*,#11510,.T.);
#16453=ORIENTED_EDGE('',*,*,#11511,.T.);
#16454=ORIENTED_EDGE('',*,*,#11512,.T.);
#16455=ORIENTED_EDGE('',*,*,#11513,.T.);
#16456=ORIENTED_EDGE('',*,*,#11514,.T.);
#16457=ORIENTED_EDGE('',*,*,#11515,.T.);
#16458=ORIENTED_EDGE('',*,*,#11516,.T.);
#16459=ORIENTED_EDGE('',*,*,#11517,.T.);
#16460=ORIENTED_EDGE('',*,*,#11518,.T.);
#16461=ORIENTED_EDGE('',*,*,#11519,.T.);
#16462=ORIENTED_EDGE('',*,*,#11520,.T.);
#16463=ORIENTED_EDGE('',*,*,#11521,.T.);
#16464=ORIENTED_EDGE('',*,*,#11522,.T.);
#16465=ORIENTED_EDGE('',*,*,#11523,.T.);
#16466=ORIENTED_EDGE('',*,*,#11524,.T.);
#16467=ORIENTED_EDGE('',*,*,#11525,.T.);
#16468=ORIENTED_EDGE('',*,*,#11526,.T.);
#16469=ORIENTED_EDGE('',*,*,#11527,.T.);
#16470=ORIENTED_EDGE('',*,*,#11528,.T.);
#16471=ORIENTED_EDGE('',*,*,#11529,.T.);
#16472=ORIENTED_EDGE('',*,*,#11530,.T.);
#16473=ORIENTED_EDGE('',*,*,#11531,.T.);
#16474=ORIENTED_EDGE('',*,*,#11532,.T.);
#16475=ORIENTED_EDGE('',*,*,#11533,.T.);
#16476=ORIENTED_EDGE('',*,*,#11534,.T.);
#16477=ORIENTED_EDGE('',*,*,#11535,.T.);
#16478=ORIENTED_EDGE('',*,*,#11536,.T.);
#16479=ORIENTED_EDGE('',*,*,#11537,.T.);
#16480=ORIENTED_EDGE('',*,*,#11538,.T.);
#16481=ORIENTED_EDGE('',*,*,#11539,.T.);
#16482=ORIENTED_EDGE('',*,*,#11540,.T.);
#16483=ORIENTED_EDGE('',*,*,#11541,.T.);
#16484=ORIENTED_EDGE('',*,*,#11542,.T.);
#16485=ORIENTED_EDGE('',*,*,#11543,.T.);
#16486=ORIENTED_EDGE('',*,*,#11544,.T.);
#16487=ORIENTED_EDGE('',*,*,#11545,.T.);
#16488=ORIENTED_EDGE('',*,*,#11546,.T.);
#16489=ORIENTED_EDGE('',*,*,#11547,.T.);
#16490=ORIENTED_EDGE('',*,*,#11548,.T.);
#16491=ORIENTED_EDGE('',*,*,#11549,.T.);
#16492=ORIENTED_EDGE('',*,*,#11550,.T.);
#16493=ORIENTED_EDGE('',*,*,#11551,.T.);
#16494=ORIENTED_EDGE('',*,*,#11552,.T.);
#16495=ORIENTED_EDGE('',*,*,#11553,.T.);
#16496=ORIENTED_EDGE('',*,*,#11554,.T.);
#16497=ORIENTED_EDGE('',*,*,#11555,.T.);
#16498=ORIENTED_EDGE('',*,*,#11556,.T.);
#16499=ORIENTED_EDGE('',*,*,#11557,.T.);
#16500=ORIENTED_EDGE('',*,*,#11558,.T.);
#16501=ORIENTED_EDGE('',*,*,#11559,.T.);
#16502=ORIENTED_EDGE('',*,*,#11560,.T.);
#16503=ORIENTED_EDGE('',*,*,#11561,.T.);
#16504=ORIENTED_EDGE('',*,*,#11562,.T.);
#16505=ORIENTED_EDGE('',*,*,#11563,.T.);
#16506=ORIENTED_EDGE('',*,*,#11564,.T.);
#16507=ORIENTED_EDGE('',*,*,#11565,.T.);
#16508=ORIENTED_EDGE('',*,*,#11566,.T.);
#16509=ORIENTED_EDGE('',*,*,#11567,.T.);
#16510=ORIENTED_EDGE('',*,*,#11568,.T.);
#16511=ORIENTED_EDGE('',*,*,#11569,.T.);
#16512=ORIENTED_EDGE('',*,*,#11570,.T.);
#16513=ORIENTED_EDGE('',*,*,#11571,.T.);
#16514=ORIENTED_EDGE('',*,*,#11572,.T.);
#16515=ORIENTED_EDGE('',*,*,#11573,.T.);
#16516=ORIENTED_EDGE('',*,*,#11574,.T.);
#16517=ORIENTED_EDGE('',*,*,#11575,.T.);
#16518=ORIENTED_EDGE('',*,*,#11576,.T.);
#16519=ORIENTED_EDGE('',*,*,#11577,.T.);
#16520=ORIENTED_EDGE('',*,*,#11578,.T.);
#16521=ORIENTED_EDGE('',*,*,#11579,.T.);
#16522=ORIENTED_EDGE('',*,*,#11580,.T.);
#16523=ORIENTED_EDGE('',*,*,#11581,.T.);
#16524=ORIENTED_EDGE('',*,*,#11582,.T.);
#16525=ORIENTED_EDGE('',*,*,#11583,.T.);
#16526=ORIENTED_EDGE('',*,*,#11584,.T.);
#16527=ORIENTED_EDGE('',*,*,#11585,.T.);
#16528=ORIENTED_EDGE('',*,*,#11586,.T.);
#16529=ORIENTED_EDGE('',*,*,#11587,.T.);
#16530=ORIENTED_EDGE('',*,*,#11588,.T.);
#16531=ORIENTED_EDGE('',*,*,#11589,.T.);
#16532=ORIENTED_EDGE('',*,*,#11590,.T.);
#16533=ORIENTED_EDGE('',*,*,#11591,.T.);
#16534=ORIENTED_EDGE('',*,*,#11592,.T.);
#16535=ORIENTED_EDGE('',*,*,#11593,.T.);
#16536=ORIENTED_EDGE('',*,*,#11594,.T.);
#16537=ORIENTED_EDGE('',*,*,#11595,.T.);
#16538=ORIENTED_EDGE('',*,*,#11596,.T.);
#16539=ORIENTED_EDGE('',*,*,#11597,.T.);
#16540=ORIENTED_EDGE('',*,*,#11598,.T.);
#16541=ORIENTED_EDGE('',*,*,#11599,.T.);
#16542=ORIENTED_EDGE('',*,*,#11600,.T.);
#16543=ORIENTED_EDGE('',*,*,#11601,.T.);
#16544=ORIENTED_EDGE('',*,*,#11602,.T.);
#16545=ORIENTED_EDGE('',*,*,#11603,.T.);
#16546=ORIENTED_EDGE('',*,*,#11604,.T.);
#16547=ORIENTED_EDGE('',*,*,#11605,.T.);
#16548=ORIENTED_EDGE('',*,*,#11606,.T.);
#16549=ORIENTED_EDGE('',*,*,#11607,.T.);
#16550=ORIENTED_EDGE('',*,*,#11608,.T.);
#16551=ORIENTED_EDGE('',*,*,#11609,.T.);
#16552=ORIENTED_EDGE('',*,*,#11610,.T.);
#16553=ORIENTED_EDGE('',*,*,#11611,.T.);
#16554=ORIENTED_EDGE('',*,*,#11612,.T.);
#16555=ORIENTED_EDGE('',*,*,#11613,.T.);
#16556=ORIENTED_EDGE('',*,*,#11614,.T.);
#16557=ORIENTED_EDGE('',*,*,#11615,.T.);
#16558=ORIENTED_EDGE('',*,*,#11616,.T.);
#16559=ORIENTED_EDGE('',*,*,#11617,.T.);
#16560=ORIENTED_EDGE('',*,*,#11618,.T.);
#16561=ORIENTED_EDGE('',*,*,#11619,.T.);
#16562=ORIENTED_EDGE('',*,*,#11620,.T.);
#16563=ORIENTED_EDGE('',*,*,#11621,.T.);
#16564=ORIENTED_EDGE('',*,*,#11622,.T.);
#16565=ORIENTED_EDGE('',*,*,#11623,.T.);
#16566=ORIENTED_EDGE('',*,*,#11624,.T.);
#16567=ORIENTED_EDGE('',*,*,#11625,.T.);
#16568=ORIENTED_EDGE('',*,*,#11626,.T.);
#16569=ORIENTED_EDGE('',*,*,#11627,.T.);
#16570=ORIENTED_EDGE('',*,*,#11628,.T.);
#16571=ORIENTED_EDGE('',*,*,#11629,.T.);
#16572=ORIENTED_EDGE('',*,*,#11630,.T.);
#16573=ORIENTED_EDGE('',*,*,#11631,.T.);
#16574=ORIENTED_EDGE('',*,*,#11632,.T.);
#16575=ORIENTED_EDGE('',*,*,#11633,.T.);
#16576=ORIENTED_EDGE('',*,*,#11634,.T.);
#16577=ORIENTED_EDGE('',*,*,#11635,.T.);
#16578=ORIENTED_EDGE('',*,*,#11636,.T.);
#16579=ORIENTED_EDGE('',*,*,#11637,.T.);
#16580=ORIENTED_EDGE('',*,*,#11638,.T.);
#16581=ORIENTED_EDGE('',*,*,#11639,.T.);
#16582=ORIENTED_EDGE('',*,*,#11640,.T.);
#16583=ORIENTED_EDGE('',*,*,#11641,.T.);
#16584=ORIENTED_EDGE('',*,*,#11642,.T.);
#16585=ORIENTED_EDGE('',*,*,#11643,.T.);
#16586=ORIENTED_EDGE('',*,*,#11644,.T.);
#16587=ORIENTED_EDGE('',*,*,#11645,.T.);
#16588=ORIENTED_EDGE('',*,*,#11646,.T.);
#16589=ORIENTED_EDGE('',*,*,#11647,.T.);
#16590=ORIENTED_EDGE('',*,*,#11648,.T.);
#16591=ORIENTED_EDGE('',*,*,#11649,.T.);
#16592=ORIENTED_EDGE('',*,*,#11650,.T.);
#16593=ORIENTED_EDGE('',*,*,#11651,.T.);
#16594=ORIENTED_EDGE('',*,*,#11652,.T.);
#16595=ORIENTED_EDGE('',*,*,#11653,.T.);
#16596=ORIENTED_EDGE('',*,*,#11654,.T.);
#16597=ORIENTED_EDGE('',*,*,#11655,.T.);
#16598=ORIENTED_EDGE('',*,*,#11656,.T.);
#16599=ORIENTED_EDGE('',*,*,#11657,.T.);
#16600=ORIENTED_EDGE('',*,*,#11658,.T.);
#16601=ORIENTED_EDGE('',*,*,#11659,.F.);
#16602=ORIENTED_EDGE('',*,*,#11507,.F.);
#16603=ORIENTED_EDGE('',*,*,#11506,.T.);
#16604=ORIENTED_EDGE('',*,*,#11660,.T.);
#16605=ORIENTED_EDGE('',*,*,#11661,.T.);
#16606=ORIENTED_EDGE('',*,*,#11660,.F.);
#16607=ORIENTED_EDGE('',*,*,#11661,.F.);
#16608=ORIENTED_EDGE('',*,*,#11662,.T.);
#16609=ORIENTED_EDGE('',*,*,#11663,.F.);
#16610=ORIENTED_EDGE('',*,*,#11662,.F.);
#16611=ORIENTED_EDGE('',*,*,#11659,.T.);
#16612=ORIENTED_EDGE('',*,*,#11664,.T.);
#16613=ORIENTED_EDGE('',*,*,#11663,.T.);
#16614=ORIENTED_EDGE('',*,*,#11664,.F.);
#16615=ORIENTED_EDGE('',*,*,#11357,.T.);
#16616=ORIENTED_EDGE('',*,*,#11665,.T.);
#16617=ORIENTED_EDGE('',*,*,#11658,.F.);
#16618=ORIENTED_EDGE('',*,*,#11666,.F.);
#16619=ORIENTED_EDGE('',*,*,#11358,.T.);
#16620=ORIENTED_EDGE('',*,*,#11666,.T.);
#16621=ORIENTED_EDGE('',*,*,#11657,.F.);
#16622=ORIENTED_EDGE('',*,*,#11667,.F.);
#16623=ORIENTED_EDGE('',*,*,#11359,.T.);
#16624=ORIENTED_EDGE('',*,*,#11667,.T.);
#16625=ORIENTED_EDGE('',*,*,#11656,.F.);
#16626=ORIENTED_EDGE('',*,*,#11668,.F.);
#16627=ORIENTED_EDGE('',*,*,#11360,.T.);
#16628=ORIENTED_EDGE('',*,*,#11668,.T.);
#16629=ORIENTED_EDGE('',*,*,#11655,.F.);
#16630=ORIENTED_EDGE('',*,*,#11669,.F.);
#16631=ORIENTED_EDGE('',*,*,#11361,.T.);
#16632=ORIENTED_EDGE('',*,*,#11669,.T.);
#16633=ORIENTED_EDGE('',*,*,#11654,.F.);
#16634=ORIENTED_EDGE('',*,*,#11670,.F.);
#16635=ORIENTED_EDGE('',*,*,#11362,.T.);
#16636=ORIENTED_EDGE('',*,*,#11670,.T.);
#16637=ORIENTED_EDGE('',*,*,#11653,.F.);
#16638=ORIENTED_EDGE('',*,*,#11671,.F.);
#16639=ORIENTED_EDGE('',*,*,#11363,.T.);
#16640=ORIENTED_EDGE('',*,*,#11671,.T.);
#16641=ORIENTED_EDGE('',*,*,#11652,.F.);
#16642=ORIENTED_EDGE('',*,*,#11672,.F.);
#16643=ORIENTED_EDGE('',*,*,#11364,.T.);
#16644=ORIENTED_EDGE('',*,*,#11672,.T.);
#16645=ORIENTED_EDGE('',*,*,#11651,.F.);
#16646=ORIENTED_EDGE('',*,*,#11673,.F.);
#16647=ORIENTED_EDGE('',*,*,#11365,.T.);
#16648=ORIENTED_EDGE('',*,*,#11673,.T.);
#16649=ORIENTED_EDGE('',*,*,#11650,.F.);
#16650=ORIENTED_EDGE('',*,*,#11674,.F.);
#16651=ORIENTED_EDGE('',*,*,#11366,.T.);
#16652=ORIENTED_EDGE('',*,*,#11674,.T.);
#16653=ORIENTED_EDGE('',*,*,#11649,.F.);
#16654=ORIENTED_EDGE('',*,*,#11675,.F.);
#16655=ORIENTED_EDGE('',*,*,#11367,.T.);
#16656=ORIENTED_EDGE('',*,*,#11675,.T.);
#16657=ORIENTED_EDGE('',*,*,#11648,.F.);
#16658=ORIENTED_EDGE('',*,*,#11676,.F.);
#16659=ORIENTED_EDGE('',*,*,#11368,.T.);
#16660=ORIENTED_EDGE('',*,*,#11676,.T.);
#16661=ORIENTED_EDGE('',*,*,#11647,.F.);
#16662=ORIENTED_EDGE('',*,*,#11677,.F.);
#16663=ORIENTED_EDGE('',*,*,#11369,.T.);
#16664=ORIENTED_EDGE('',*,*,#11677,.T.);
#16665=ORIENTED_EDGE('',*,*,#11646,.F.);
#16666=ORIENTED_EDGE('',*,*,#11678,.F.);
#16667=ORIENTED_EDGE('',*,*,#11370,.T.);
#16668=ORIENTED_EDGE('',*,*,#11678,.T.);
#16669=ORIENTED_EDGE('',*,*,#11645,.F.);
#16670=ORIENTED_EDGE('',*,*,#11679,.F.);
#16671=ORIENTED_EDGE('',*,*,#11371,.T.);
#16672=ORIENTED_EDGE('',*,*,#11679,.T.);
#16673=ORIENTED_EDGE('',*,*,#11644,.F.);
#16674=ORIENTED_EDGE('',*,*,#11680,.F.);
#16675=ORIENTED_EDGE('',*,*,#11372,.T.);
#16676=ORIENTED_EDGE('',*,*,#11680,.T.);
#16677=ORIENTED_EDGE('',*,*,#11643,.F.);
#16678=ORIENTED_EDGE('',*,*,#11681,.F.);
#16679=ORIENTED_EDGE('',*,*,#11373,.T.);
#16680=ORIENTED_EDGE('',*,*,#11681,.T.);
#16681=ORIENTED_EDGE('',*,*,#11642,.F.);
#16682=ORIENTED_EDGE('',*,*,#11682,.F.);
#16683=ORIENTED_EDGE('',*,*,#11374,.T.);
#16684=ORIENTED_EDGE('',*,*,#11682,.T.);
#16685=ORIENTED_EDGE('',*,*,#11641,.F.);
#16686=ORIENTED_EDGE('',*,*,#11683,.F.);
#16687=ORIENTED_EDGE('',*,*,#11375,.T.);
#16688=ORIENTED_EDGE('',*,*,#11683,.T.);
#16689=ORIENTED_EDGE('',*,*,#11640,.F.);
#16690=ORIENTED_EDGE('',*,*,#11684,.F.);
#16691=ORIENTED_EDGE('',*,*,#11376,.T.);
#16692=ORIENTED_EDGE('',*,*,#11684,.T.);
#16693=ORIENTED_EDGE('',*,*,#11639,.F.);
#16694=ORIENTED_EDGE('',*,*,#11685,.F.);
#16695=ORIENTED_EDGE('',*,*,#11377,.T.);
#16696=ORIENTED_EDGE('',*,*,#11685,.T.);
#16697=ORIENTED_EDGE('',*,*,#11638,.F.);
#16698=ORIENTED_EDGE('',*,*,#11686,.F.);
#16699=ORIENTED_EDGE('',*,*,#11378,.T.);
#16700=ORIENTED_EDGE('',*,*,#11686,.T.);
#16701=ORIENTED_EDGE('',*,*,#11637,.F.);
#16702=ORIENTED_EDGE('',*,*,#11687,.F.);
#16703=ORIENTED_EDGE('',*,*,#11379,.T.);
#16704=ORIENTED_EDGE('',*,*,#11687,.T.);
#16705=ORIENTED_EDGE('',*,*,#11636,.F.);
#16706=ORIENTED_EDGE('',*,*,#11688,.F.);
#16707=ORIENTED_EDGE('',*,*,#11380,.T.);
#16708=ORIENTED_EDGE('',*,*,#11688,.T.);
#16709=ORIENTED_EDGE('',*,*,#11635,.F.);
#16710=ORIENTED_EDGE('',*,*,#11689,.F.);
#16711=ORIENTED_EDGE('',*,*,#11381,.T.);
#16712=ORIENTED_EDGE('',*,*,#11689,.T.);
#16713=ORIENTED_EDGE('',*,*,#11634,.F.);
#16714=ORIENTED_EDGE('',*,*,#11690,.F.);
#16715=ORIENTED_EDGE('',*,*,#11382,.T.);
#16716=ORIENTED_EDGE('',*,*,#11690,.T.);
#16717=ORIENTED_EDGE('',*,*,#11633,.F.);
#16718=ORIENTED_EDGE('',*,*,#11691,.F.);
#16719=ORIENTED_EDGE('',*,*,#11383,.T.);
#16720=ORIENTED_EDGE('',*,*,#11691,.T.);
#16721=ORIENTED_EDGE('',*,*,#11632,.F.);
#16722=ORIENTED_EDGE('',*,*,#11692,.F.);
#16723=ORIENTED_EDGE('',*,*,#11384,.T.);
#16724=ORIENTED_EDGE('',*,*,#11692,.T.);
#16725=ORIENTED_EDGE('',*,*,#11631,.F.);
#16726=ORIENTED_EDGE('',*,*,#11693,.F.);
#16727=ORIENTED_EDGE('',*,*,#11385,.T.);
#16728=ORIENTED_EDGE('',*,*,#11693,.T.);
#16729=ORIENTED_EDGE('',*,*,#11630,.F.);
#16730=ORIENTED_EDGE('',*,*,#11694,.F.);
#16731=ORIENTED_EDGE('',*,*,#11386,.T.);
#16732=ORIENTED_EDGE('',*,*,#11694,.T.);
#16733=ORIENTED_EDGE('',*,*,#11629,.F.);
#16734=ORIENTED_EDGE('',*,*,#11695,.F.);
#16735=ORIENTED_EDGE('',*,*,#11387,.T.);
#16736=ORIENTED_EDGE('',*,*,#11695,.T.);
#16737=ORIENTED_EDGE('',*,*,#11628,.F.);
#16738=ORIENTED_EDGE('',*,*,#11696,.F.);
#16739=ORIENTED_EDGE('',*,*,#11388,.T.);
#16740=ORIENTED_EDGE('',*,*,#11696,.T.);
#16741=ORIENTED_EDGE('',*,*,#11627,.F.);
#16742=ORIENTED_EDGE('',*,*,#11697,.F.);
#16743=ORIENTED_EDGE('',*,*,#11389,.T.);
#16744=ORIENTED_EDGE('',*,*,#11697,.T.);
#16745=ORIENTED_EDGE('',*,*,#11626,.F.);
#16746=ORIENTED_EDGE('',*,*,#11698,.F.);
#16747=ORIENTED_EDGE('',*,*,#11390,.T.);
#16748=ORIENTED_EDGE('',*,*,#11698,.T.);
#16749=ORIENTED_EDGE('',*,*,#11625,.F.);
#16750=ORIENTED_EDGE('',*,*,#11699,.F.);
#16751=ORIENTED_EDGE('',*,*,#11391,.T.);
#16752=ORIENTED_EDGE('',*,*,#11699,.T.);
#16753=ORIENTED_EDGE('',*,*,#11624,.F.);
#16754=ORIENTED_EDGE('',*,*,#11700,.F.);
#16755=ORIENTED_EDGE('',*,*,#11392,.T.);
#16756=ORIENTED_EDGE('',*,*,#11700,.T.);
#16757=ORIENTED_EDGE('',*,*,#11623,.F.);
#16758=ORIENTED_EDGE('',*,*,#11701,.F.);
#16759=ORIENTED_EDGE('',*,*,#11393,.T.);
#16760=ORIENTED_EDGE('',*,*,#11701,.T.);
#16761=ORIENTED_EDGE('',*,*,#11622,.F.);
#16762=ORIENTED_EDGE('',*,*,#11702,.F.);
#16763=ORIENTED_EDGE('',*,*,#11394,.T.);
#16764=ORIENTED_EDGE('',*,*,#11702,.T.);
#16765=ORIENTED_EDGE('',*,*,#11621,.F.);
#16766=ORIENTED_EDGE('',*,*,#11703,.F.);
#16767=ORIENTED_EDGE('',*,*,#11395,.T.);
#16768=ORIENTED_EDGE('',*,*,#11703,.T.);
#16769=ORIENTED_EDGE('',*,*,#11620,.F.);
#16770=ORIENTED_EDGE('',*,*,#11704,.F.);
#16771=ORIENTED_EDGE('',*,*,#11396,.T.);
#16772=ORIENTED_EDGE('',*,*,#11704,.T.);
#16773=ORIENTED_EDGE('',*,*,#11619,.F.);
#16774=ORIENTED_EDGE('',*,*,#11705,.F.);
#16775=ORIENTED_EDGE('',*,*,#11397,.T.);
#16776=ORIENTED_EDGE('',*,*,#11705,.T.);
#16777=ORIENTED_EDGE('',*,*,#11618,.F.);
#16778=ORIENTED_EDGE('',*,*,#11706,.F.);
#16779=ORIENTED_EDGE('',*,*,#11398,.T.);
#16780=ORIENTED_EDGE('',*,*,#11706,.T.);
#16781=ORIENTED_EDGE('',*,*,#11617,.F.);
#16782=ORIENTED_EDGE('',*,*,#11707,.F.);
#16783=ORIENTED_EDGE('',*,*,#11399,.T.);
#16784=ORIENTED_EDGE('',*,*,#11707,.T.);
#16785=ORIENTED_EDGE('',*,*,#11616,.F.);
#16786=ORIENTED_EDGE('',*,*,#11708,.F.);
#16787=ORIENTED_EDGE('',*,*,#11400,.T.);
#16788=ORIENTED_EDGE('',*,*,#11708,.T.);
#16789=ORIENTED_EDGE('',*,*,#11615,.F.);
#16790=ORIENTED_EDGE('',*,*,#11709,.F.);
#16791=ORIENTED_EDGE('',*,*,#11401,.T.);
#16792=ORIENTED_EDGE('',*,*,#11709,.T.);
#16793=ORIENTED_EDGE('',*,*,#11614,.F.);
#16794=ORIENTED_EDGE('',*,*,#11710,.F.);
#16795=ORIENTED_EDGE('',*,*,#11402,.T.);
#16796=ORIENTED_EDGE('',*,*,#11710,.T.);
#16797=ORIENTED_EDGE('',*,*,#11613,.F.);
#16798=ORIENTED_EDGE('',*,*,#11711,.F.);
#16799=ORIENTED_EDGE('',*,*,#11403,.T.);
#16800=ORIENTED_EDGE('',*,*,#11711,.T.);
#16801=ORIENTED_EDGE('',*,*,#11612,.F.);
#16802=ORIENTED_EDGE('',*,*,#11712,.F.);
#16803=ORIENTED_EDGE('',*,*,#11404,.T.);
#16804=ORIENTED_EDGE('',*,*,#11712,.T.);
#16805=ORIENTED_EDGE('',*,*,#11611,.F.);
#16806=ORIENTED_EDGE('',*,*,#11713,.F.);
#16807=ORIENTED_EDGE('',*,*,#11405,.T.);
#16808=ORIENTED_EDGE('',*,*,#11713,.T.);
#16809=ORIENTED_EDGE('',*,*,#11610,.F.);
#16810=ORIENTED_EDGE('',*,*,#11714,.F.);
#16811=ORIENTED_EDGE('',*,*,#11406,.T.);
#16812=ORIENTED_EDGE('',*,*,#11714,.T.);
#16813=ORIENTED_EDGE('',*,*,#11609,.F.);
#16814=ORIENTED_EDGE('',*,*,#11715,.F.);
#16815=ORIENTED_EDGE('',*,*,#11407,.T.);
#16816=ORIENTED_EDGE('',*,*,#11715,.T.);
#16817=ORIENTED_EDGE('',*,*,#11608,.F.);
#16818=ORIENTED_EDGE('',*,*,#11716,.F.);
#16819=ORIENTED_EDGE('',*,*,#11408,.T.);
#16820=ORIENTED_EDGE('',*,*,#11716,.T.);
#16821=ORIENTED_EDGE('',*,*,#11607,.F.);
#16822=ORIENTED_EDGE('',*,*,#11717,.F.);
#16823=ORIENTED_EDGE('',*,*,#11409,.T.);
#16824=ORIENTED_EDGE('',*,*,#11717,.T.);
#16825=ORIENTED_EDGE('',*,*,#11606,.F.);
#16826=ORIENTED_EDGE('',*,*,#11718,.F.);
#16827=ORIENTED_EDGE('',*,*,#11410,.T.);
#16828=ORIENTED_EDGE('',*,*,#11718,.T.);
#16829=ORIENTED_EDGE('',*,*,#11605,.F.);
#16830=ORIENTED_EDGE('',*,*,#11719,.F.);
#16831=ORIENTED_EDGE('',*,*,#11411,.T.);
#16832=ORIENTED_EDGE('',*,*,#11719,.T.);
#16833=ORIENTED_EDGE('',*,*,#11604,.F.);
#16834=ORIENTED_EDGE('',*,*,#11720,.F.);
#16835=ORIENTED_EDGE('',*,*,#11412,.T.);
#16836=ORIENTED_EDGE('',*,*,#11720,.T.);
#16837=ORIENTED_EDGE('',*,*,#11603,.F.);
#16838=ORIENTED_EDGE('',*,*,#11721,.F.);
#16839=ORIENTED_EDGE('',*,*,#11413,.T.);
#16840=ORIENTED_EDGE('',*,*,#11721,.T.);
#16841=ORIENTED_EDGE('',*,*,#11602,.F.);
#16842=ORIENTED_EDGE('',*,*,#11722,.F.);
#16843=ORIENTED_EDGE('',*,*,#11414,.T.);
#16844=ORIENTED_EDGE('',*,*,#11722,.T.);
#16845=ORIENTED_EDGE('',*,*,#11601,.F.);
#16846=ORIENTED_EDGE('',*,*,#11723,.F.);
#16847=ORIENTED_EDGE('',*,*,#11415,.T.);
#16848=ORIENTED_EDGE('',*,*,#11723,.T.);
#16849=ORIENTED_EDGE('',*,*,#11600,.F.);
#16850=ORIENTED_EDGE('',*,*,#11724,.F.);
#16851=ORIENTED_EDGE('',*,*,#11416,.T.);
#16852=ORIENTED_EDGE('',*,*,#11724,.T.);
#16853=ORIENTED_EDGE('',*,*,#11599,.F.);
#16854=ORIENTED_EDGE('',*,*,#11725,.F.);
#16855=ORIENTED_EDGE('',*,*,#11417,.T.);
#16856=ORIENTED_EDGE('',*,*,#11725,.T.);
#16857=ORIENTED_EDGE('',*,*,#11598,.F.);
#16858=ORIENTED_EDGE('',*,*,#11726,.F.);
#16859=ORIENTED_EDGE('',*,*,#11418,.T.);
#16860=ORIENTED_EDGE('',*,*,#11726,.T.);
#16861=ORIENTED_EDGE('',*,*,#11597,.F.);
#16862=ORIENTED_EDGE('',*,*,#11727,.F.);
#16863=ORIENTED_EDGE('',*,*,#11419,.T.);
#16864=ORIENTED_EDGE('',*,*,#11727,.T.);
#16865=ORIENTED_EDGE('',*,*,#11596,.F.);
#16866=ORIENTED_EDGE('',*,*,#11728,.F.);
#16867=ORIENTED_EDGE('',*,*,#11420,.T.);
#16868=ORIENTED_EDGE('',*,*,#11728,.T.);
#16869=ORIENTED_EDGE('',*,*,#11595,.F.);
#16870=ORIENTED_EDGE('',*,*,#11729,.F.);
#16871=ORIENTED_EDGE('',*,*,#11421,.T.);
#16872=ORIENTED_EDGE('',*,*,#11729,.T.);
#16873=ORIENTED_EDGE('',*,*,#11594,.F.);
#16874=ORIENTED_EDGE('',*,*,#11730,.F.);
#16875=ORIENTED_EDGE('',*,*,#11422,.T.);
#16876=ORIENTED_EDGE('',*,*,#11730,.T.);
#16877=ORIENTED_EDGE('',*,*,#11593,.F.);
#16878=ORIENTED_EDGE('',*,*,#11731,.F.);
#16879=ORIENTED_EDGE('',*,*,#11423,.T.);
#16880=ORIENTED_EDGE('',*,*,#11731,.T.);
#16881=ORIENTED_EDGE('',*,*,#11592,.F.);
#16882=ORIENTED_EDGE('',*,*,#11732,.F.);
#16883=ORIENTED_EDGE('',*,*,#11424,.T.);
#16884=ORIENTED_EDGE('',*,*,#11732,.T.);
#16885=ORIENTED_EDGE('',*,*,#11591,.F.);
#16886=ORIENTED_EDGE('',*,*,#11733,.F.);
#16887=ORIENTED_EDGE('',*,*,#11425,.T.);
#16888=ORIENTED_EDGE('',*,*,#11733,.T.);
#16889=ORIENTED_EDGE('',*,*,#11590,.F.);
#16890=ORIENTED_EDGE('',*,*,#11734,.F.);
#16891=ORIENTED_EDGE('',*,*,#11426,.T.);
#16892=ORIENTED_EDGE('',*,*,#11734,.T.);
#16893=ORIENTED_EDGE('',*,*,#11589,.F.);
#16894=ORIENTED_EDGE('',*,*,#11735,.F.);
#16895=ORIENTED_EDGE('',*,*,#11427,.T.);
#16896=ORIENTED_EDGE('',*,*,#11735,.T.);
#16897=ORIENTED_EDGE('',*,*,#11588,.F.);
#16898=ORIENTED_EDGE('',*,*,#11736,.F.);
#16899=ORIENTED_EDGE('',*,*,#11428,.T.);
#16900=ORIENTED_EDGE('',*,*,#11736,.T.);
#16901=ORIENTED_EDGE('',*,*,#11587,.F.);
#16902=ORIENTED_EDGE('',*,*,#11737,.F.);
#16903=ORIENTED_EDGE('',*,*,#11429,.T.);
#16904=ORIENTED_EDGE('',*,*,#11737,.T.);
#16905=ORIENTED_EDGE('',*,*,#11586,.F.);
#16906=ORIENTED_EDGE('',*,*,#11738,.F.);
#16907=ORIENTED_EDGE('',*,*,#11430,.T.);
#16908=ORIENTED_EDGE('',*,*,#11738,.T.);
#16909=ORIENTED_EDGE('',*,*,#11585,.F.);
#16910=ORIENTED_EDGE('',*,*,#11739,.F.);
#16911=ORIENTED_EDGE('',*,*,#11431,.T.);
#16912=ORIENTED_EDGE('',*,*,#11739,.T.);
#16913=ORIENTED_EDGE('',*,*,#11584,.F.);
#16914=ORIENTED_EDGE('',*,*,#11740,.F.);
#16915=ORIENTED_EDGE('',*,*,#11432,.T.);
#16916=ORIENTED_EDGE('',*,*,#11740,.T.);
#16917=ORIENTED_EDGE('',*,*,#11583,.F.);
#16918=ORIENTED_EDGE('',*,*,#11741,.F.);
#16919=ORIENTED_EDGE('',*,*,#11433,.T.);
#16920=ORIENTED_EDGE('',*,*,#11741,.T.);
#16921=ORIENTED_EDGE('',*,*,#11582,.F.);
#16922=ORIENTED_EDGE('',*,*,#11742,.F.);
#16923=ORIENTED_EDGE('',*,*,#11434,.T.);
#16924=ORIENTED_EDGE('',*,*,#11742,.T.);
#16925=ORIENTED_EDGE('',*,*,#11581,.F.);
#16926=ORIENTED_EDGE('',*,*,#11743,.F.);
#16927=ORIENTED_EDGE('',*,*,#11435,.T.);
#16928=ORIENTED_EDGE('',*,*,#11743,.T.);
#16929=ORIENTED_EDGE('',*,*,#11580,.F.);
#16930=ORIENTED_EDGE('',*,*,#11744,.F.);
#16931=ORIENTED_EDGE('',*,*,#11436,.T.);
#16932=ORIENTED_EDGE('',*,*,#11744,.T.);
#16933=ORIENTED_EDGE('',*,*,#11579,.F.);
#16934=ORIENTED_EDGE('',*,*,#11745,.F.);
#16935=ORIENTED_EDGE('',*,*,#11437,.T.);
#16936=ORIENTED_EDGE('',*,*,#11745,.T.);
#16937=ORIENTED_EDGE('',*,*,#11578,.F.);
#16938=ORIENTED_EDGE('',*,*,#11746,.F.);
#16939=ORIENTED_EDGE('',*,*,#11438,.T.);
#16940=ORIENTED_EDGE('',*,*,#11746,.T.);
#16941=ORIENTED_EDGE('',*,*,#11577,.F.);
#16942=ORIENTED_EDGE('',*,*,#11747,.F.);
#16943=ORIENTED_EDGE('',*,*,#11439,.T.);
#16944=ORIENTED_EDGE('',*,*,#11747,.T.);
#16945=ORIENTED_EDGE('',*,*,#11576,.F.);
#16946=ORIENTED_EDGE('',*,*,#11748,.F.);
#16947=ORIENTED_EDGE('',*,*,#11440,.T.);
#16948=ORIENTED_EDGE('',*,*,#11748,.T.);
#16949=ORIENTED_EDGE('',*,*,#11575,.F.);
#16950=ORIENTED_EDGE('',*,*,#11749,.F.);
#16951=ORIENTED_EDGE('',*,*,#11441,.T.);
#16952=ORIENTED_EDGE('',*,*,#11749,.T.);
#16953=ORIENTED_EDGE('',*,*,#11574,.F.);
#16954=ORIENTED_EDGE('',*,*,#11750,.F.);
#16955=ORIENTED_EDGE('',*,*,#11442,.T.);
#16956=ORIENTED_EDGE('',*,*,#11750,.T.);
#16957=ORIENTED_EDGE('',*,*,#11573,.F.);
#16958=ORIENTED_EDGE('',*,*,#11751,.F.);
#16959=ORIENTED_EDGE('',*,*,#11443,.T.);
#16960=ORIENTED_EDGE('',*,*,#11751,.T.);
#16961=ORIENTED_EDGE('',*,*,#11572,.F.);
#16962=ORIENTED_EDGE('',*,*,#11752,.F.);
#16963=ORIENTED_EDGE('',*,*,#11444,.T.);
#16964=ORIENTED_EDGE('',*,*,#11752,.T.);
#16965=ORIENTED_EDGE('',*,*,#11571,.F.);
#16966=ORIENTED_EDGE('',*,*,#11753,.F.);
#16967=ORIENTED_EDGE('',*,*,#11445,.T.);
#16968=ORIENTED_EDGE('',*,*,#11753,.T.);
#16969=ORIENTED_EDGE('',*,*,#11570,.F.);
#16970=ORIENTED_EDGE('',*,*,#11754,.F.);
#16971=ORIENTED_EDGE('',*,*,#11446,.T.);
#16972=ORIENTED_EDGE('',*,*,#11754,.T.);
#16973=ORIENTED_EDGE('',*,*,#11569,.F.);
#16974=ORIENTED_EDGE('',*,*,#11755,.F.);
#16975=ORIENTED_EDGE('',*,*,#11447,.T.);
#16976=ORIENTED_EDGE('',*,*,#11755,.T.);
#16977=ORIENTED_EDGE('',*,*,#11568,.F.);
#16978=ORIENTED_EDGE('',*,*,#11756,.F.);
#16979=ORIENTED_EDGE('',*,*,#11448,.T.);
#16980=ORIENTED_EDGE('',*,*,#11756,.T.);
#16981=ORIENTED_EDGE('',*,*,#11567,.F.);
#16982=ORIENTED_EDGE('',*,*,#11757,.F.);
#16983=ORIENTED_EDGE('',*,*,#11449,.T.);
#16984=ORIENTED_EDGE('',*,*,#11757,.T.);
#16985=ORIENTED_EDGE('',*,*,#11566,.F.);
#16986=ORIENTED_EDGE('',*,*,#11758,.F.);
#16987=ORIENTED_EDGE('',*,*,#11450,.T.);
#16988=ORIENTED_EDGE('',*,*,#11758,.T.);
#16989=ORIENTED_EDGE('',*,*,#11565,.F.);
#16990=ORIENTED_EDGE('',*,*,#11759,.F.);
#16991=ORIENTED_EDGE('',*,*,#11451,.T.);
#16992=ORIENTED_EDGE('',*,*,#11759,.T.);
#16993=ORIENTED_EDGE('',*,*,#11564,.F.);
#16994=ORIENTED_EDGE('',*,*,#11760,.F.);
#16995=ORIENTED_EDGE('',*,*,#11452,.T.);
#16996=ORIENTED_EDGE('',*,*,#11760,.T.);
#16997=ORIENTED_EDGE('',*,*,#11563,.F.);
#16998=ORIENTED_EDGE('',*,*,#11761,.F.);
#16999=ORIENTED_EDGE('',*,*,#11453,.T.);
#17000=ORIENTED_EDGE('',*,*,#11761,.T.);
#17001=ORIENTED_EDGE('',*,*,#11562,.F.);
#17002=ORIENTED_EDGE('',*,*,#11762,.F.);
#17003=ORIENTED_EDGE('',*,*,#11454,.T.);
#17004=ORIENTED_EDGE('',*,*,#11762,.T.);
#17005=ORIENTED_EDGE('',*,*,#11561,.F.);
#17006=ORIENTED_EDGE('',*,*,#11763,.F.);
#17007=ORIENTED_EDGE('',*,*,#11455,.T.);
#17008=ORIENTED_EDGE('',*,*,#11763,.T.);
#17009=ORIENTED_EDGE('',*,*,#11560,.F.);
#17010=ORIENTED_EDGE('',*,*,#11764,.F.);
#17011=ORIENTED_EDGE('',*,*,#11456,.T.);
#17012=ORIENTED_EDGE('',*,*,#11764,.T.);
#17013=ORIENTED_EDGE('',*,*,#11559,.F.);
#17014=ORIENTED_EDGE('',*,*,#11765,.F.);
#17015=ORIENTED_EDGE('',*,*,#11457,.T.);
#17016=ORIENTED_EDGE('',*,*,#11765,.T.);
#17017=ORIENTED_EDGE('',*,*,#11558,.F.);
#17018=ORIENTED_EDGE('',*,*,#11766,.F.);
#17019=ORIENTED_EDGE('',*,*,#11458,.T.);
#17020=ORIENTED_EDGE('',*,*,#11766,.T.);
#17021=ORIENTED_EDGE('',*,*,#11557,.F.);
#17022=ORIENTED_EDGE('',*,*,#11767,.F.);
#17023=ORIENTED_EDGE('',*,*,#11459,.T.);
#17024=ORIENTED_EDGE('',*,*,#11767,.T.);
#17025=ORIENTED_EDGE('',*,*,#11556,.F.);
#17026=ORIENTED_EDGE('',*,*,#11768,.F.);
#17027=ORIENTED_EDGE('',*,*,#11460,.T.);
#17028=ORIENTED_EDGE('',*,*,#11768,.T.);
#17029=ORIENTED_EDGE('',*,*,#11555,.F.);
#17030=ORIENTED_EDGE('',*,*,#11769,.F.);
#17031=ORIENTED_EDGE('',*,*,#11461,.T.);
#17032=ORIENTED_EDGE('',*,*,#11769,.T.);
#17033=ORIENTED_EDGE('',*,*,#11554,.F.);
#17034=ORIENTED_EDGE('',*,*,#11770,.F.);
#17035=ORIENTED_EDGE('',*,*,#11462,.T.);
#17036=ORIENTED_EDGE('',*,*,#11770,.T.);
#17037=ORIENTED_EDGE('',*,*,#11553,.F.);
#17038=ORIENTED_EDGE('',*,*,#11771,.F.);
#17039=ORIENTED_EDGE('',*,*,#11463,.T.);
#17040=ORIENTED_EDGE('',*,*,#11771,.T.);
#17041=ORIENTED_EDGE('',*,*,#11552,.F.);
#17042=ORIENTED_EDGE('',*,*,#11772,.F.);
#17043=ORIENTED_EDGE('',*,*,#11464,.T.);
#17044=ORIENTED_EDGE('',*,*,#11772,.T.);
#17045=ORIENTED_EDGE('',*,*,#11551,.F.);
#17046=ORIENTED_EDGE('',*,*,#11773,.F.);
#17047=ORIENTED_EDGE('',*,*,#11465,.T.);
#17048=ORIENTED_EDGE('',*,*,#11773,.T.);
#17049=ORIENTED_EDGE('',*,*,#11550,.F.);
#17050=ORIENTED_EDGE('',*,*,#11774,.F.);
#17051=ORIENTED_EDGE('',*,*,#11466,.T.);
#17052=ORIENTED_EDGE('',*,*,#11774,.T.);
#17053=ORIENTED_EDGE('',*,*,#11549,.F.);
#17054=ORIENTED_EDGE('',*,*,#11775,.F.);
#17055=ORIENTED_EDGE('',*,*,#11467,.T.);
#17056=ORIENTED_EDGE('',*,*,#11775,.T.);
#17057=ORIENTED_EDGE('',*,*,#11548,.F.);
#17058=ORIENTED_EDGE('',*,*,#11776,.F.);
#17059=ORIENTED_EDGE('',*,*,#11468,.T.);
#17060=ORIENTED_EDGE('',*,*,#11776,.T.);
#17061=ORIENTED_EDGE('',*,*,#11547,.F.);
#17062=ORIENTED_EDGE('',*,*,#11777,.F.);
#17063=ORIENTED_EDGE('',*,*,#11469,.T.);
#17064=ORIENTED_EDGE('',*,*,#11777,.T.);
#17065=ORIENTED_EDGE('',*,*,#11546,.F.);
#17066=ORIENTED_EDGE('',*,*,#11778,.F.);
#17067=ORIENTED_EDGE('',*,*,#11470,.T.);
#17068=ORIENTED_EDGE('',*,*,#11778,.T.);
#17069=ORIENTED_EDGE('',*,*,#11545,.F.);
#17070=ORIENTED_EDGE('',*,*,#11779,.F.);
#17071=ORIENTED_EDGE('',*,*,#11471,.T.);
#17072=ORIENTED_EDGE('',*,*,#11779,.T.);
#17073=ORIENTED_EDGE('',*,*,#11544,.F.);
#17074=ORIENTED_EDGE('',*,*,#11780,.F.);
#17075=ORIENTED_EDGE('',*,*,#11472,.T.);
#17076=ORIENTED_EDGE('',*,*,#11780,.T.);
#17077=ORIENTED_EDGE('',*,*,#11543,.F.);
#17078=ORIENTED_EDGE('',*,*,#11781,.F.);
#17079=ORIENTED_EDGE('',*,*,#11473,.T.);
#17080=ORIENTED_EDGE('',*,*,#11781,.T.);
#17081=ORIENTED_EDGE('',*,*,#11542,.F.);
#17082=ORIENTED_EDGE('',*,*,#11782,.F.);
#17083=ORIENTED_EDGE('',*,*,#11474,.T.);
#17084=ORIENTED_EDGE('',*,*,#11782,.T.);
#17085=ORIENTED_EDGE('',*,*,#11541,.F.);
#17086=ORIENTED_EDGE('',*,*,#11783,.F.);
#17087=ORIENTED_EDGE('',*,*,#11475,.T.);
#17088=ORIENTED_EDGE('',*,*,#11783,.T.);
#17089=ORIENTED_EDGE('',*,*,#11540,.F.);
#17090=ORIENTED_EDGE('',*,*,#11784,.F.);
#17091=ORIENTED_EDGE('',*,*,#11476,.T.);
#17092=ORIENTED_EDGE('',*,*,#11784,.T.);
#17093=ORIENTED_EDGE('',*,*,#11539,.F.);
#17094=ORIENTED_EDGE('',*,*,#11785,.F.);
#17095=ORIENTED_EDGE('',*,*,#11477,.T.);
#17096=ORIENTED_EDGE('',*,*,#11785,.T.);
#17097=ORIENTED_EDGE('',*,*,#11538,.F.);
#17098=ORIENTED_EDGE('',*,*,#11786,.F.);
#17099=ORIENTED_EDGE('',*,*,#11478,.T.);
#17100=ORIENTED_EDGE('',*,*,#11786,.T.);
#17101=ORIENTED_EDGE('',*,*,#11537,.F.);
#17102=ORIENTED_EDGE('',*,*,#11787,.F.);
#17103=ORIENTED_EDGE('',*,*,#11479,.T.);
#17104=ORIENTED_EDGE('',*,*,#11787,.T.);
#17105=ORIENTED_EDGE('',*,*,#11536,.F.);
#17106=ORIENTED_EDGE('',*,*,#11788,.F.);
#17107=ORIENTED_EDGE('',*,*,#11480,.T.);
#17108=ORIENTED_EDGE('',*,*,#11788,.T.);
#17109=ORIENTED_EDGE('',*,*,#11535,.F.);
#17110=ORIENTED_EDGE('',*,*,#11789,.F.);
#17111=ORIENTED_EDGE('',*,*,#11481,.T.);
#17112=ORIENTED_EDGE('',*,*,#11789,.T.);
#17113=ORIENTED_EDGE('',*,*,#11534,.F.);
#17114=ORIENTED_EDGE('',*,*,#11790,.F.);
#17115=ORIENTED_EDGE('',*,*,#11482,.T.);
#17116=ORIENTED_EDGE('',*,*,#11790,.T.);
#17117=ORIENTED_EDGE('',*,*,#11533,.F.);
#17118=ORIENTED_EDGE('',*,*,#11791,.F.);
#17119=ORIENTED_EDGE('',*,*,#11483,.T.);
#17120=ORIENTED_EDGE('',*,*,#11791,.T.);
#17121=ORIENTED_EDGE('',*,*,#11532,.F.);
#17122=ORIENTED_EDGE('',*,*,#11792,.F.);
#17123=ORIENTED_EDGE('',*,*,#11484,.T.);
#17124=ORIENTED_EDGE('',*,*,#11792,.T.);
#17125=ORIENTED_EDGE('',*,*,#11531,.F.);
#17126=ORIENTED_EDGE('',*,*,#11793,.F.);
#17127=ORIENTED_EDGE('',*,*,#11485,.T.);
#17128=ORIENTED_EDGE('',*,*,#11793,.T.);
#17129=ORIENTED_EDGE('',*,*,#11530,.F.);
#17130=ORIENTED_EDGE('',*,*,#11794,.F.);
#17131=ORIENTED_EDGE('',*,*,#11486,.T.);
#17132=ORIENTED_EDGE('',*,*,#11794,.T.);
#17133=ORIENTED_EDGE('',*,*,#11529,.F.);
#17134=ORIENTED_EDGE('',*,*,#11795,.F.);
#17135=ORIENTED_EDGE('',*,*,#11487,.T.);
#17136=ORIENTED_EDGE('',*,*,#11795,.T.);
#17137=ORIENTED_EDGE('',*,*,#11528,.F.);
#17138=ORIENTED_EDGE('',*,*,#11796,.F.);
#17139=ORIENTED_EDGE('',*,*,#11488,.T.);
#17140=ORIENTED_EDGE('',*,*,#11796,.T.);
#17141=ORIENTED_EDGE('',*,*,#11527,.F.);
#17142=ORIENTED_EDGE('',*,*,#11797,.F.);
#17143=ORIENTED_EDGE('',*,*,#11489,.T.);
#17144=ORIENTED_EDGE('',*,*,#11797,.T.);
#17145=ORIENTED_EDGE('',*,*,#11526,.F.);
#17146=ORIENTED_EDGE('',*,*,#11798,.F.);
#17147=ORIENTED_EDGE('',*,*,#11490,.T.);
#17148=ORIENTED_EDGE('',*,*,#11798,.T.);
#17149=ORIENTED_EDGE('',*,*,#11525,.F.);
#17150=ORIENTED_EDGE('',*,*,#11799,.F.);
#17151=ORIENTED_EDGE('',*,*,#11491,.T.);
#17152=ORIENTED_EDGE('',*,*,#11799,.T.);
#17153=ORIENTED_EDGE('',*,*,#11524,.F.);
#17154=ORIENTED_EDGE('',*,*,#11800,.F.);
#17155=ORIENTED_EDGE('',*,*,#11492,.T.);
#17156=ORIENTED_EDGE('',*,*,#11800,.T.);
#17157=ORIENTED_EDGE('',*,*,#11523,.F.);
#17158=ORIENTED_EDGE('',*,*,#11801,.F.);
#17159=ORIENTED_EDGE('',*,*,#11493,.T.);
#17160=ORIENTED_EDGE('',*,*,#11801,.T.);
#17161=ORIENTED_EDGE('',*,*,#11522,.F.);
#17162=ORIENTED_EDGE('',*,*,#11802,.F.);
#17163=ORIENTED_EDGE('',*,*,#11494,.T.);
#17164=ORIENTED_EDGE('',*,*,#11802,.T.);
#17165=ORIENTED_EDGE('',*,*,#11521,.F.);
#17166=ORIENTED_EDGE('',*,*,#11803,.F.);
#17167=ORIENTED_EDGE('',*,*,#11495,.T.);
#17168=ORIENTED_EDGE('',*,*,#11803,.T.);
#17169=ORIENTED_EDGE('',*,*,#11520,.F.);
#17170=ORIENTED_EDGE('',*,*,#11804,.F.);
#17171=ORIENTED_EDGE('',*,*,#11496,.T.);
#17172=ORIENTED_EDGE('',*,*,#11804,.T.);
#17173=ORIENTED_EDGE('',*,*,#11519,.F.);
#17174=ORIENTED_EDGE('',*,*,#11805,.F.);
#17175=ORIENTED_EDGE('',*,*,#11497,.T.);
#17176=ORIENTED_EDGE('',*,*,#11805,.T.);
#17177=ORIENTED_EDGE('',*,*,#11518,.F.);
#17178=ORIENTED_EDGE('',*,*,#11806,.F.);
#17179=ORIENTED_EDGE('',*,*,#11498,.T.);
#17180=ORIENTED_EDGE('',*,*,#11806,.T.);
#17181=ORIENTED_EDGE('',*,*,#11517,.F.);
#17182=ORIENTED_EDGE('',*,*,#11807,.F.);
#17183=ORIENTED_EDGE('',*,*,#11499,.T.);
#17184=ORIENTED_EDGE('',*,*,#11807,.T.);
#17185=ORIENTED_EDGE('',*,*,#11516,.F.);
#17186=ORIENTED_EDGE('',*,*,#11808,.F.);
#17187=ORIENTED_EDGE('',*,*,#11500,.T.);
#17188=ORIENTED_EDGE('',*,*,#11808,.T.);
#17189=ORIENTED_EDGE('',*,*,#11515,.F.);
#17190=ORIENTED_EDGE('',*,*,#11809,.F.);
#17191=ORIENTED_EDGE('',*,*,#11501,.T.);
#17192=ORIENTED_EDGE('',*,*,#11809,.T.);
#17193=ORIENTED_EDGE('',*,*,#11514,.F.);
#17194=ORIENTED_EDGE('',*,*,#11810,.F.);
#17195=ORIENTED_EDGE('',*,*,#11502,.T.);
#17196=ORIENTED_EDGE('',*,*,#11810,.T.);
#17197=ORIENTED_EDGE('',*,*,#11513,.F.);
#17198=ORIENTED_EDGE('',*,*,#11811,.F.);
#17199=ORIENTED_EDGE('',*,*,#11503,.T.);
#17200=ORIENTED_EDGE('',*,*,#11811,.T.);
#17201=ORIENTED_EDGE('',*,*,#11512,.F.);
#17202=ORIENTED_EDGE('',*,*,#11812,.F.);
#17203=ORIENTED_EDGE('',*,*,#11504,.T.);
#17204=ORIENTED_EDGE('',*,*,#11812,.T.);
#17205=ORIENTED_EDGE('',*,*,#11511,.F.);
#17206=ORIENTED_EDGE('',*,*,#11813,.F.);
#17207=ORIENTED_EDGE('',*,*,#11505,.T.);
#17208=ORIENTED_EDGE('',*,*,#11813,.T.);
#17209=ORIENTED_EDGE('',*,*,#11510,.F.);
#17210=ORIENTED_EDGE('',*,*,#11814,.F.);
#17211=ORIENTED_EDGE('',*,*,#11356,.T.);
#17212=ORIENTED_EDGE('',*,*,#11814,.T.);
#17213=ORIENTED_EDGE('',*,*,#11509,.F.);
#17214=ORIENTED_EDGE('',*,*,#11665,.F.);
#17215=CYLINDRICAL_SURFACE('',#18420,3.442);
#17216=CYLINDRICAL_SURFACE('',#18422,3.442);
#17217=CYLINDRICAL_SURFACE('',#18423,3.442);
#17218=CYLINDRICAL_SURFACE('',#18424,3.442);
#17219=CYLINDRICAL_SURFACE('',#18425,3.442);
#17220=CYLINDRICAL_SURFACE('',#18426,3.442);
#17221=CYLINDRICAL_SURFACE('',#18427,3.442);
#17222=CYLINDRICAL_SURFACE('',#18428,3.442);
#17223=CYLINDRICAL_SURFACE('',#18429,3.442);
#17224=CYLINDRICAL_SURFACE('',#18430,3.442);
#17225=CYLINDRICAL_SURFACE('',#18431,3.442);
#17226=CYLINDRICAL_SURFACE('',#18432,3.442);
#17227=CYLINDRICAL_SURFACE('',#18433,3.442);
#17228=CYLINDRICAL_SURFACE('',#18434,3.442);
#17229=CYLINDRICAL_SURFACE('',#18435,3.442);
#17230=CYLINDRICAL_SURFACE('',#18436,3.442);
#17231=CYLINDRICAL_SURFACE('',#18460,2.872);
#17232=CYLINDRICAL_SURFACE('',#18462,2.872);
#17233=CYLINDRICAL_SURFACE('',#18463,2.872);
#17234=CYLINDRICAL_SURFACE('',#18464,2.872);
#17235=CYLINDRICAL_SURFACE('',#18465,2.872);
#17236=CYLINDRICAL_SURFACE('',#18466,2.872);
#17237=CYLINDRICAL_SURFACE('',#18467,2.872);
#17238=CYLINDRICAL_SURFACE('',#18468,2.872);
#17239=CYLINDRICAL_SURFACE('',#18469,2.872);
#17240=CYLINDRICAL_SURFACE('',#18470,2.872);
#17241=CYLINDRICAL_SURFACE('',#18471,2.872);
#17242=CYLINDRICAL_SURFACE('',#18472,2.872);
#17243=CYLINDRICAL_SURFACE('',#18473,2.872);
#17244=CYLINDRICAL_SURFACE('',#18474,2.872);
#17245=CYLINDRICAL_SURFACE('',#18475,2.872);
#17246=CYLINDRICAL_SURFACE('',#18476,2.872);
#17247=CYLINDRICAL_SURFACE('',#18535,35.);
#17248=CYLINDRICAL_SURFACE('',#18540,35.);
#17249=CYLINDRICAL_SURFACE('',#18545,35.);
#17250=CYLINDRICAL_SURFACE('',#18550,35.);
#17251=CYLINDRICAL_SURFACE('',#18555,35.);
#17252=CYLINDRICAL_SURFACE('',#18560,35.);
#17253=CYLINDRICAL_SURFACE('',#18565,35.);
#17254=CYLINDRICAL_SURFACE('',#18570,35.);
#17255=CYLINDRICAL_SURFACE('',#18575,35.);
#17256=CYLINDRICAL_SURFACE('',#18580,35.);
#17257=CYLINDRICAL_SURFACE('',#18585,35.);
#17258=CYLINDRICAL_SURFACE('',#18590,35.);
#17259=CYLINDRICAL_SURFACE('',#18597,9.2);
#17260=CYLINDRICAL_SURFACE('',#18604,9.2);
#17261=CYLINDRICAL_SURFACE('',#18613,33.);
#17262=CYLINDRICAL_SURFACE('',#18625,33.);
#17263=CYLINDRICAL_SURFACE('',#18637,33.);
#17264=CYLINDRICAL_SURFACE('',#18649,33.);
#17265=CYLINDRICAL_SURFACE('',#18661,33.);
#17266=CYLINDRICAL_SURFACE('',#18687,8.);
#17267=CYLINDRICAL_SURFACE('',#18689,8.);
#17268=CYLINDRICAL_SURFACE('',#18692,33.);
#17269=CYLINDRICAL_SURFACE('',#18702,33.);
#17270=CYLINDRICAL_SURFACE('',#18712,33.);
#17271=CYLINDRICAL_SURFACE('',#18722,33.);
#17272=CYLINDRICAL_SURFACE('',#18732,33.);
#17273=CYLINDRICAL_SURFACE('',#18742,33.);
#17274=CYLINDRICAL_SURFACE('',#18748,33.);
#17275=CYLINDRICAL_SURFACE('',#18758,8.);
#17276=CYLINDRICAL_SURFACE('',#18767,2.872);
#17277=CYLINDRICAL_SURFACE('',#18773,8.);
#17278=CYLINDRICAL_SURFACE('',#18778,8.);
#17279=CYLINDRICAL_SURFACE('',#18783,8.);
#17280=CYLINDRICAL_SURFACE('',#18788,8.);
#17281=CYLINDRICAL_SURFACE('',#18793,8.);
#17282=CYLINDRICAL_SURFACE('',#18798,8.);
#17283=CYLINDRICAL_SURFACE('',#18803,8.);
#17284=CYLINDRICAL_SURFACE('',#18808,8.);
#17285=CYLINDRICAL_SURFACE('',#18813,8.);
#17286=CYLINDRICAL_SURFACE('',#18822,8.5);
#17287=CYLINDRICAL_SURFACE('',#18828,9.2);
#17288=CYLINDRICAL_SURFACE('',#18830,7.7);
#17289=CYLINDRICAL_SURFACE('',#18894,5.5);
#17290=CYLINDRICAL_SURFACE('',#18900,3.3);
#17291=CYLINDRICAL_SURFACE('',#18904,3.5);
#17292=CYLINDRICAL_SURFACE('',#18908,2.9);
#17293=CYLINDRICAL_SURFACE('',#18911,3.442);
#17294=CYLINDRICAL_SURFACE('',#18925,8.5);
#17295=CYLINDRICAL_SURFACE('',#18933,3.505);
#17296=CYLINDRICAL_SURFACE('',#18962,17.);
#17297=CYLINDRICAL_SURFACE('',#18965,2.65);
#17298=CYLINDRICAL_SURFACE('',#18970,2.65);
#17299=CYLINDRICAL_SURFACE('',#18975,2.65);
#17300=CYLINDRICAL_SURFACE('',#18980,1.);
#17301=CYLINDRICAL_SURFACE('',#19161,5.85);
#17302=CYLINDRICAL_SURFACE('',#19164,0.600000000000001);
#17303=CYLINDRICAL_SURFACE('',#19168,0.6);
#17304=CYLINDRICAL_SURFACE('',#19172,0.600000000000001);
#17305=CYLINDRICAL_SURFACE('',#19176,0.600000000000001);
#17306=CYLINDRICAL_SURFACE('',#19180,0.6);
#17307=CYLINDRICAL_SURFACE('',#19184,0.600000000000001);
#17308=CYLINDRICAL_SURFACE('',#19188,6.6);
#17309=CYLINDRICAL_SURFACE('',#19195,7.6);
#17310=CYLINDRICAL_SURFACE('',#19200,5.75);
#17311=CYLINDRICAL_SURFACE('',#19206,8.5);
#17312=CYLINDRICAL_SURFACE('',#19214,7.6);
#17313=CYLINDRICAL_SURFACE('',#19221,3.505);
#17314=CYLINDRICAL_SURFACE('',#19237,39.);
#17315=CYLINDRICAL_SURFACE('',#19297,3.525);
#17316=CYLINDRICAL_SURFACE('',#19365,8.7);
#17317=CYLINDRICAL_SURFACE('',#19430,3.55);
#17318=CYLINDRICAL_SURFACE('',#19435,6.5);
#17319=CYLINDRICAL_SURFACE('',#19444,0.6);
#17320=CYLINDRICAL_SURFACE('',#19451,0.6);
#17321=CYLINDRICAL_SURFACE('',#19458,0.6);
#17322=CYLINDRICAL_SURFACE('',#19465,0.6);
#17323=CYLINDRICAL_SURFACE('',#19469,1.1);
#17324=CYLINDRICAL_SURFACE('',#19470,1.1);
#17325=CYLINDRICAL_SURFACE('',#19471,1.1);
#17326=CYLINDRICAL_SURFACE('',#19472,1.1);
#17327=CYLINDRICAL_SURFACE('',#19473,8.45);
#17328=CYLINDRICAL_SURFACE('',#19480,8.8);
#17329=CYLINDRICAL_SURFACE('',#19485,8.8);
#17330=CYLINDRICAL_SURFACE('',#19492,5.52);
#17331=CYLINDRICAL_SURFACE('',#19501,0.55);
#17332=CYLINDRICAL_SURFACE('',#19511,0.55);
#17333=ADVANCED_FACE('',(#1305),#17215,.T.);
#17334=ADVANCED_FACE('',(#1306),#17216,.T.);
#17335=ADVANCED_FACE('',(#1307),#17217,.T.);
#17336=ADVANCED_FACE('',(#1308),#17218,.T.);
#17337=ADVANCED_FACE('',(#1309),#17219,.T.);
#17338=ADVANCED_FACE('',(#1310),#17220,.T.);
#17339=ADVANCED_FACE('',(#1311),#17221,.T.);
#17340=ADVANCED_FACE('',(#1312),#17222,.T.);
#17341=ADVANCED_FACE('',(#1313),#17223,.T.);
#17342=ADVANCED_FACE('',(#1314),#17224,.T.);
#17343=ADVANCED_FACE('',(#1315),#17225,.T.);
#17344=ADVANCED_FACE('',(#1316),#17226,.T.);
#17345=ADVANCED_FACE('',(#1317),#17227,.T.);
#17346=ADVANCED_FACE('',(#1318),#17228,.T.);
#17347=ADVANCED_FACE('',(#1319),#17229,.T.);
#17348=ADVANCED_FACE('',(#1320),#17230,.T.);
#17349=ADVANCED_FACE('',(#1321),#1064,.T.);
#17350=ADVANCED_FACE('',(#1322),#17231,.T.);
#17351=ADVANCED_FACE('',(#1323),#17232,.T.);
#17352=ADVANCED_FACE('',(#1324),#17233,.T.);
#17353=ADVANCED_FACE('',(#1325),#17234,.T.);
#17354=ADVANCED_FACE('',(#1326),#17235,.T.);
#17355=ADVANCED_FACE('',(#1327),#17236,.T.);
#17356=ADVANCED_FACE('',(#1328),#17237,.T.);
#17357=ADVANCED_FACE('',(#1329),#17238,.T.);
#17358=ADVANCED_FACE('',(#1330),#17239,.T.);
#17359=ADVANCED_FACE('',(#1331),#17240,.T.);
#17360=ADVANCED_FACE('',(#1332),#17241,.T.);
#17361=ADVANCED_FACE('',(#1333),#17242,.T.);
#17362=ADVANCED_FACE('',(#1334),#17243,.T.);
#17363=ADVANCED_FACE('',(#1335),#17244,.T.);
#17364=ADVANCED_FACE('',(#1336),#17245,.T.);
#17365=ADVANCED_FACE('',(#1337),#17246,.T.);
#17366=ADVANCED_FACE('',(#1338),#827,.T.);
#17367=ADVANCED_FACE('',(#1339),#828,.T.);
#17368=ADVANCED_FACE('',(#1340,#197),#264,.T.);
#17369=ADVANCED_FACE('',(#1341),#265,.T.);
#17370=ADVANCED_FACE('',(#1342),#266,.T.);
#17371=ADVANCED_FACE('',(#1343),#267,.T.);
#17372=ADVANCED_FACE('',(#1344),#268,.T.);
#17373=ADVANCED_FACE('',(#1345),#269,.T.);
#17374=ADVANCED_FACE('',(#1346),#270,.T.);
#17375=ADVANCED_FACE('',(#1347),#271,.T.);
#17376=ADVANCED_FACE('',(#1348),#272,.T.);
#17377=ADVANCED_FACE('',(#1349),#273,.T.);
#17378=ADVANCED_FACE('',(#1350),#274,.T.);
#17379=ADVANCED_FACE('',(#1351),#275,.T.);
#17380=ADVANCED_FACE('',(#1352),#276,.T.);
#17381=ADVANCED_FACE('',(#1353),#277,.T.);
#17382=ADVANCED_FACE('',(#1354),#278,.T.);
#17383=ADVANCED_FACE('',(#1355),#279,.T.);
#17384=ADVANCED_FACE('',(#1356),#280,.T.);
#17385=ADVANCED_FACE('',(#1357),#281,.T.);
#17386=ADVANCED_FACE('',(#1358),#282,.T.);
#17387=ADVANCED_FACE('',(#1359),#283,.T.);
#17388=ADVANCED_FACE('',(#1360),#284,.T.);
#17389=ADVANCED_FACE('',(#1361),#285,.T.);
#17390=ADVANCED_FACE('',(#1362),#286,.T.);
#17391=ADVANCED_FACE('',(#1363),#287,.T.);
#17392=ADVANCED_FACE('',(#1364),#288,.T.);
#17393=ADVANCED_FACE('',(#1365),#289,.T.);
#17394=ADVANCED_FACE('',(#1366),#290,.T.);
#17395=ADVANCED_FACE('',(#1367),#291,.T.);
#17396=ADVANCED_FACE('',(#1368),#292,.T.);
#17397=ADVANCED_FACE('',(#1369),#293,.T.);
#17398=ADVANCED_FACE('',(#1370),#294,.T.);
#17399=ADVANCED_FACE('',(#1371),#295,.T.);
#17400=ADVANCED_FACE('',(#1372),#296,.T.);
#17401=ADVANCED_FACE('',(#1373),#297,.T.);
#17402=ADVANCED_FACE('',(#1374),#298,.T.);
#17403=ADVANCED_FACE('',(#1375),#299,.T.);
#17404=ADVANCED_FACE('',(#1376),#300,.T.);
#17405=ADVANCED_FACE('',(#1377),#301,.T.);
#17406=ADVANCED_FACE('',(#1378),#302,.T.);
#17407=ADVANCED_FACE('',(#1379),#303,.T.);
#17408=ADVANCED_FACE('',(#1380),#304,.T.);
#17409=ADVANCED_FACE('',(#1381),#305,.T.);
#17410=ADVANCED_FACE('',(#1382),#306,.T.);
#17411=ADVANCED_FACE('',(#1383),#307,.T.);
#17412=ADVANCED_FACE('',(#1384),#308,.T.);
#17413=ADVANCED_FACE('',(#1385),#309,.T.);
#17414=ADVANCED_FACE('',(#1386),#310,.T.);
#17415=ADVANCED_FACE('',(#1387),#311,.T.);
#17416=ADVANCED_FACE('',(#1388),#829,.T.);
#17417=ADVANCED_FACE('',(#1389),#17247,.T.);
#17418=ADVANCED_FACE('',(#1390),#97,.T.);
#17419=ADVANCED_FACE('',(#1391),#830,.T.);
#17420=ADVANCED_FACE('',(#1392),#17248,.T.);
#17421=ADVANCED_FACE('',(#1393),#98,.T.);
#17422=ADVANCED_FACE('',(#1394),#831,.T.);
#17423=ADVANCED_FACE('',(#1395),#17249,.T.);
#17424=ADVANCED_FACE('',(#1396),#99,.T.);
#17425=ADVANCED_FACE('',(#1397),#832,.T.);
#17426=ADVANCED_FACE('',(#1398),#17250,.T.);
#17427=ADVANCED_FACE('',(#1399),#100,.T.);
#17428=ADVANCED_FACE('',(#1400),#833,.T.);
#17429=ADVANCED_FACE('',(#1401),#17251,.T.);
#17430=ADVANCED_FACE('',(#1402),#101,.T.);
#17431=ADVANCED_FACE('',(#1403),#834,.T.);
#17432=ADVANCED_FACE('',(#1404),#17252,.T.);
#17433=ADVANCED_FACE('',(#1405),#102,.T.);
#17434=ADVANCED_FACE('',(#1406),#835,.T.);
#17435=ADVANCED_FACE('',(#1407),#17253,.T.);
#17436=ADVANCED_FACE('',(#1408),#103,.T.);
#17437=ADVANCED_FACE('',(#1409),#836,.T.);
#17438=ADVANCED_FACE('',(#1410),#17254,.T.);
#17439=ADVANCED_FACE('',(#1411),#104,.T.);
#17440=ADVANCED_FACE('',(#1412),#837,.T.);
#17441=ADVANCED_FACE('',(#1413),#17255,.T.);
#17442=ADVANCED_FACE('',(#1414),#105,.T.);
#17443=ADVANCED_FACE('',(#1415),#838,.T.);
#17444=ADVANCED_FACE('',(#1416),#17256,.T.);
#17445=ADVANCED_FACE('',(#1417),#106,.T.);
#17446=ADVANCED_FACE('',(#1418),#839,.T.);
#17447=ADVANCED_FACE('',(#1419),#17257,.T.);
#17448=ADVANCED_FACE('',(#1420),#107,.T.);
#17449=ADVANCED_FACE('',(#1421),#840,.T.);
#17450=ADVANCED_FACE('',(#1422),#17258,.T.);
#17451=ADVANCED_FACE('',(#1423),#108,.T.);
#17452=ADVANCED_FACE('',(#1424),#841,.T.);
#17453=ADVANCED_FACE('',(#1425,#198),#312,.F.);
#17454=ADVANCED_FACE('',(#1426),#17259,.T.);
#17455=ADVANCED_FACE('',(#1427),#842,.T.);
#17456=ADVANCED_FACE('',(#1428,#199),#313,.F.);
#17457=ADVANCED_FACE('',(#1429),#17260,.T.);
#17458=ADVANCED_FACE('',(#1430),#314,.T.);
#17459=ADVANCED_FACE('',(#1431),#843,.F.);
#17460=ADVANCED_FACE('',(#1432),#844,.T.);
#17461=ADVANCED_FACE('',(#1433),#17261,.T.);
#17462=ADVANCED_FACE('',(#1434),#315,.T.);
#17463=ADVANCED_FACE('',(#1435),#845,.F.);
#17464=ADVANCED_FACE('',(#1436),#316,.T.);
#17465=ADVANCED_FACE('',(#1437),#846,.T.);
#17466=ADVANCED_FACE('',(#1438),#17262,.T.);
#17467=ADVANCED_FACE('',(#1439),#317,.T.);
#17468=ADVANCED_FACE('',(#1440),#847,.F.);
#17469=ADVANCED_FACE('',(#1441),#318,.T.);
#17470=ADVANCED_FACE('',(#1442),#848,.T.);
#17471=ADVANCED_FACE('',(#1443),#17263,.T.);
#17472=ADVANCED_FACE('',(#1444),#319,.T.);
#17473=ADVANCED_FACE('',(#1445),#849,.F.);
#17474=ADVANCED_FACE('',(#1446),#320,.T.);
#17475=ADVANCED_FACE('',(#1447),#850,.T.);
#17476=ADVANCED_FACE('',(#1448),#17264,.T.);
#17477=ADVANCED_FACE('',(#1449),#321,.T.);
#17478=ADVANCED_FACE('',(#1450),#851,.F.);
#17479=ADVANCED_FACE('',(#1451),#322,.T.);
#17480=ADVANCED_FACE('',(#1452),#852,.T.);
#17481=ADVANCED_FACE('',(#1453),#17265,.T.);
#17482=ADVANCED_FACE('',(#1454),#323,.T.);
#17483=ADVANCED_FACE('',(#1455),#853,.F.);
#17484=ADVANCED_FACE('',(#1456,#200),#324,.T.);
#17485=ADVANCED_FACE('',(#1457),#854,.T.);
#17486=ADVANCED_FACE('',(#1458),#325,.T.);
#17487=ADVANCED_FACE('',(#1459),#17266,.F.);
#17488=ADVANCED_FACE('',(#1460),#17267,.F.);
#17489=ADVANCED_FACE('',(#1461),#326,.T.);
#17490=ADVANCED_FACE('',(#1462),#17268,.T.);
#17491=ADVANCED_FACE('',(#1463),#327,.T.);
#17492=ADVANCED_FACE('',(#1464),#855,.F.);
#17493=ADVANCED_FACE('',(#1465),#856,.T.);
#17494=ADVANCED_FACE('',(#1466),#328,.T.);
#17495=ADVANCED_FACE('',(#1467),#17269,.T.);
#17496=ADVANCED_FACE('',(#1468),#329,.T.);
#17497=ADVANCED_FACE('',(#1469),#857,.F.);
#17498=ADVANCED_FACE('',(#1470),#858,.T.);
#17499=ADVANCED_FACE('',(#1471),#330,.T.);
#17500=ADVANCED_FACE('',(#1472),#17270,.T.);
#17501=ADVANCED_FACE('',(#1473),#331,.T.);
#17502=ADVANCED_FACE('',(#1474),#859,.F.);
#17503=ADVANCED_FACE('',(#1475),#860,.T.);
#17504=ADVANCED_FACE('',(#1476),#332,.T.);
#17505=ADVANCED_FACE('',(#1477),#17271,.T.);
#17506=ADVANCED_FACE('',(#1478),#333,.T.);
#17507=ADVANCED_FACE('',(#1479),#861,.F.);
#17508=ADVANCED_FACE('',(#1480),#862,.T.);
#17509=ADVANCED_FACE('',(#1481),#334,.T.);
#17510=ADVANCED_FACE('',(#1482),#17272,.T.);
#17511=ADVANCED_FACE('',(#1483),#335,.T.);
#17512=ADVANCED_FACE('',(#1484),#863,.F.);
#17513=ADVANCED_FACE('',(#1485),#864,.T.);
#17514=ADVANCED_FACE('',(#1486),#336,.T.);
#17515=ADVANCED_FACE('',(#1487),#17273,.T.);
#17516=ADVANCED_FACE('',(#1488),#865,.T.);
#17517=ADVANCED_FACE('',(#1489),#17274,.T.);
#17518=ADVANCED_FACE('',(#1490),#337,.T.);
#17519=ADVANCED_FACE('',(#1491),#866,.F.);
#17520=ADVANCED_FACE('',(#1492),#338,.T.);
#17521=ADVANCED_FACE('',(#1493),#867,.T.);
#17522=ADVANCED_FACE('',(#1494),#17275,.F.);
#17523=ADVANCED_FACE('',(#1495),#339,.F.);
#17524=ADVANCED_FACE('',(#1496),#109,.F.);
#17525=ADVANCED_FACE('',(#1497),#340,.T.);
#17526=ADVANCED_FACE('',(#1498),#17276,.T.);
#17527=ADVANCED_FACE('',(#1499),#110,.F.);
#17528=ADVANCED_FACE('',(#1500),#341,.T.);
#17529=ADVANCED_FACE('',(#1501),#1065,.T.);
#17530=ADVANCED_FACE('',(#1502),#868,.T.);
#17531=ADVANCED_FACE('',(#1503),#342,.T.);
#17532=ADVANCED_FACE('',(#1504),#17277,.F.);
#17533=ADVANCED_FACE('',(#1505),#869,.T.);
#17534=ADVANCED_FACE('',(#1506),#870,.T.);
#17535=ADVANCED_FACE('',(#1507),#343,.T.);
#17536=ADVANCED_FACE('',(#1508),#17278,.F.);
#17537=ADVANCED_FACE('',(#1509),#871,.T.);
#17538=ADVANCED_FACE('',(#1510),#872,.T.);
#17539=ADVANCED_FACE('',(#1511),#344,.T.);
#17540=ADVANCED_FACE('',(#1512),#17279,.F.);
#17541=ADVANCED_FACE('',(#1513),#873,.T.);
#17542=ADVANCED_FACE('',(#1514),#874,.T.);
#17543=ADVANCED_FACE('',(#1515),#345,.T.);
#17544=ADVANCED_FACE('',(#1516),#17280,.F.);
#17545=ADVANCED_FACE('',(#1517),#875,.T.);
#17546=ADVANCED_FACE('',(#1518),#876,.T.);
#17547=ADVANCED_FACE('',(#1519),#346,.T.);
#17548=ADVANCED_FACE('',(#1520),#17281,.F.);
#17549=ADVANCED_FACE('',(#1521),#877,.T.);
#17550=ADVANCED_FACE('',(#1522),#878,.T.);
#17551=ADVANCED_FACE('',(#1523),#347,.T.);
#17552=ADVANCED_FACE('',(#1524),#17282,.F.);
#17553=ADVANCED_FACE('',(#1525),#879,.T.);
#17554=ADVANCED_FACE('',(#1526),#880,.T.);
#17555=ADVANCED_FACE('',(#1527),#348,.T.);
#17556=ADVANCED_FACE('',(#1528),#17283,.F.);
#17557=ADVANCED_FACE('',(#1529),#881,.T.);
#17558=ADVANCED_FACE('',(#1530),#882,.T.);
#17559=ADVANCED_FACE('',(#1531),#349,.T.);
#17560=ADVANCED_FACE('',(#1532),#17284,.F.);
#17561=ADVANCED_FACE('',(#1533),#883,.T.);
#17562=ADVANCED_FACE('',(#1534),#884,.T.);
#17563=ADVANCED_FACE('',(#1535),#350,.T.);
#17564=ADVANCED_FACE('',(#1536),#17285,.F.);
#17565=ADVANCED_FACE('',(#1537),#885,.T.);
#17566=ADVANCED_FACE('',(#1538),#886,.T.);
#17567=ADVANCED_FACE('',(#1539),#351,.T.);
#17568=ADVANCED_FACE('',(#1540),#887,.T.);
#17569=ADVANCED_FACE('',(#1541),#888,.T.);
#17570=ADVANCED_FACE('',(#1542),#352,.T.);
#17571=ADVANCED_FACE('',(#1543),#889,.T.);
#17572=ADVANCED_FACE('',(#1544),#890,.T.);
#17573=ADVANCED_FACE('',(#1545),#17286,.T.);
#17574=ADVANCED_FACE('',(#1546,#201),#353,.F.);
#17575=ADVANCED_FACE('',(#1547,#202),#354,.F.);
#17576=ADVANCED_FACE('',(#1548),#17287,.T.);
#17577=ADVANCED_FACE('',(#1549),#17288,.T.);
#17578=ADVANCED_FACE('',(#1550),#355,.T.);
#17579=ADVANCED_FACE('',(#1551),#356,.T.);
#17580=ADVANCED_FACE('',(#1552),#1066,.T.);
#17581=ADVANCED_FACE('',(#1553),#111,.F.);
#17582=ADVANCED_FACE('',(#1554),#357,.T.);
#17583=ADVANCED_FACE('',(#1555),#358,.T.);
#17584=ADVANCED_FACE('',(#1556),#1067,.T.);
#17585=ADVANCED_FACE('',(#1557),#112,.F.);
#17586=ADVANCED_FACE('',(#1558),#359,.T.);
#17587=ADVANCED_FACE('',(#1559),#360,.T.);
#17588=ADVANCED_FACE('',(#1560),#1068,.T.);
#17589=ADVANCED_FACE('',(#1561),#113,.F.);
#17590=ADVANCED_FACE('',(#1562),#361,.T.);
#17591=ADVANCED_FACE('',(#1563),#362,.T.);
#17592=ADVANCED_FACE('',(#1564),#1069,.T.);
#17593=ADVANCED_FACE('',(#1565),#114,.F.);
#17594=ADVANCED_FACE('',(#1566),#363,.T.);
#17595=ADVANCED_FACE('',(#1567),#364,.T.);
#17596=ADVANCED_FACE('',(#1568),#1070,.T.);
#17597=ADVANCED_FACE('',(#1569),#115,.F.);
#17598=ADVANCED_FACE('',(#1570),#365,.T.);
#17599=ADVANCED_FACE('',(#1571),#366,.T.);
#17600=ADVANCED_FACE('',(#1572),#1071,.T.);
#17601=ADVANCED_FACE('',(#1573),#116,.F.);
#17602=ADVANCED_FACE('',(#1574),#367,.T.);
#17603=ADVANCED_FACE('',(#1575),#368,.T.);
#17604=ADVANCED_FACE('',(#1576),#1072,.T.);
#17605=ADVANCED_FACE('',(#1577),#117,.F.);
#17606=ADVANCED_FACE('',(#1578),#369,.T.);
#17607=ADVANCED_FACE('',(#1579),#370,.T.);
#17608=ADVANCED_FACE('',(#1580),#1073,.T.);
#17609=ADVANCED_FACE('',(#1581),#118,.F.);
#17610=ADVANCED_FACE('',(#1582),#371,.T.);
#17611=ADVANCED_FACE('',(#1583),#372,.T.);
#17612=ADVANCED_FACE('',(#1584),#1074,.T.);
#17613=ADVANCED_FACE('',(#1585),#119,.F.);
#17614=ADVANCED_FACE('',(#1586),#373,.T.);
#17615=ADVANCED_FACE('',(#1587),#374,.T.);
#17616=ADVANCED_FACE('',(#1588),#1075,.T.);
#17617=ADVANCED_FACE('',(#1589),#120,.F.);
#17618=ADVANCED_FACE('',(#1590),#375,.T.);
#17619=ADVANCED_FACE('',(#1591),#376,.T.);
#17620=ADVANCED_FACE('',(#1592),#1076,.T.);
#17621=ADVANCED_FACE('',(#1593),#121,.F.);
#17622=ADVANCED_FACE('',(#1594),#377,.T.);
#17623=ADVANCED_FACE('',(#1595),#378,.T.);
#17624=ADVANCED_FACE('',(#1596),#1077,.T.);
#17625=ADVANCED_FACE('',(#1597),#122,.F.);
#17626=ADVANCED_FACE('',(#1598),#379,.T.);
#17627=ADVANCED_FACE('',(#1599),#380,.T.);
#17628=ADVANCED_FACE('',(#1600),#381,.T.);
#17629=ADVANCED_FACE('',(#1601),#382,.T.);
#17630=ADVANCED_FACE('',(#1602),#383,.T.);
#17631=ADVANCED_FACE('',(#1603),#384,.T.);
#17632=ADVANCED_FACE('',(#1604),#385,.T.);
#17633=ADVANCED_FACE('',(#1605),#386,.F.);
#17634=ADVANCED_FACE('',(#1606),#387,.T.);
#17635=ADVANCED_FACE('',(#1607),#388,.T.);
#17636=ADVANCED_FACE('',(#1608),#389,.T.);
#17637=ADVANCED_FACE('',(#1609),#390,.T.);
#17638=ADVANCED_FACE('',(#1610),#391,.T.);
#17639=ADVANCED_FACE('',(#1611),#392,.T.);
#17640=ADVANCED_FACE('',(#1612,#203),#393,.T.);
#17641=ADVANCED_FACE('',(#1613),#891,.T.);
#17642=ADVANCED_FACE('',(#1614),#892,.T.);
#17643=ADVANCED_FACE('',(#1615),#893,.T.);
#17644=ADVANCED_FACE('',(#1616),#894,.T.);
#17645=ADVANCED_FACE('',(#1617,#204),#394,.T.);
#17646=ADVANCED_FACE('',(#1618),#895,.T.);
#17647=ADVANCED_FACE('',(#1619),#896,.T.);
#17648=ADVANCED_FACE('',(#1620),#17289,.T.);
#17649=ADVANCED_FACE('',(#1621),#897,.T.);
#17650=ADVANCED_FACE('',(#1622,#205),#395,.T.);
#17651=ADVANCED_FACE('',(#1623),#17290,.T.);
#17652=ADVANCED_FACE('',(#1624),#898,.T.);
#17653=ADVANCED_FACE('',(#1625),#17291,.T.);
#17654=ADVANCED_FACE('',(#1626),#899,.T.);
#17655=ADVANCED_FACE('',(#1627),#17292,.T.);
#17656=ADVANCED_FACE('',(#1628),#900,.T.);
#17657=ADVANCED_FACE('',(#1629),#17293,.T.);
#17658=ADVANCED_FACE('',(#1630),#901,.T.);
#17659=ADVANCED_FACE('',(#1631),#396,.T.);
#17660=ADVANCED_FACE('',(#1632),#123,.T.);
#17661=ADVANCED_FACE('',(#1633),#397,.T.);
#17662=ADVANCED_FACE('',(#1634),#1078,.T.);
#17663=ADVANCED_FACE('',(#1635),#124,.T.);
#17664=ADVANCED_FACE('',(#1636),#125,.T.);
#17665=ADVANCED_FACE('',(#1637),#1079,.T.);
#17666=ADVANCED_FACE('',(#1638),#126,.T.);
#17667=ADVANCED_FACE('',(#1639),#398,.T.);
#17668=ADVANCED_FACE('',(#1640),#399,.T.);
#17669=ADVANCED_FACE('',(#1641),#400,.F.);
#17670=ADVANCED_FACE('',(#1642),#902,.T.);
#17671=ADVANCED_FACE('',(#1643),#17294,.T.);
#17672=ADVANCED_FACE('',(#1644),#903,.T.);
#17673=ADVANCED_FACE('',(#1645,#206),#401,.T.);
#17674=ADVANCED_FACE('',(#1646),#904,.F.);
#17675=ADVANCED_FACE('',(#1647),#17295,.F.);
#17676=ADVANCED_FACE('',(#1648),#905,.F.);
#17677=ADVANCED_FACE('',(#1649,#207),#402,.T.);
#17678=ADVANCED_FACE('',(#1650),#403,.T.);
#17679=ADVANCED_FACE('',(#1651,#208),#404,.T.);
#17680=ADVANCED_FACE('',(#1652),#405,.T.);
#17681=ADVANCED_FACE('',(#1653,#209,#210,#211,#212,#213,#214,#215,#216,
#217,#218),#406,.F.);
#17682=ADVANCED_FACE('',(#1654),#906,.T.);
#17683=ADVANCED_FACE('',(#1655),#407,.T.);
#17684=ADVANCED_FACE('',(#1656),#907,.T.);
#17685=ADVANCED_FACE('',(#1657),#408,.T.);
#17686=ADVANCED_FACE('',(#1658),#409,.T.);
#17687=ADVANCED_FACE('',(#1659,#219,#220,#221,#222,#223,#224,#225,#226,
#227,#228),#410,.T.);
#17688=ADVANCED_FACE('',(#1660),#17296,.T.);
#17689=ADVANCED_FACE('',(#1661),#908,.F.);
#17690=ADVANCED_FACE('',(#1662),#17297,.F.);
#17691=ADVANCED_FACE('',(#1663),#909,.F.);
#17692=ADVANCED_FACE('',(#1664),#910,.F.);
#17693=ADVANCED_FACE('',(#1665),#17298,.F.);
#17694=ADVANCED_FACE('',(#1666),#911,.F.);
#17695=ADVANCED_FACE('',(#1667),#912,.F.);
#17696=ADVANCED_FACE('',(#1668),#17299,.F.);
#17697=ADVANCED_FACE('',(#1669),#913,.F.);
#17698=ADVANCED_FACE('',(#1670),#914,.F.);
#17699=ADVANCED_FACE('',(#1671),#17300,.F.);
#17700=ADVANCED_FACE('',(#1672),#411,.F.);
#17701=ADVANCED_FACE('',(#1673),#412,.F.);
#17702=ADVANCED_FACE('',(#1674),#413,.F.);
#17703=ADVANCED_FACE('',(#1675),#414,.F.);
#17704=ADVANCED_FACE('',(#1676),#415,.F.);
#17705=ADVANCED_FACE('',(#1677),#416,.F.);
#17706=ADVANCED_FACE('',(#1678),#417,.F.);
#17707=ADVANCED_FACE('',(#1679),#418,.F.);
#17708=ADVANCED_FACE('',(#1680),#419,.F.);
#17709=ADVANCED_FACE('',(#1681),#420,.F.);
#17710=ADVANCED_FACE('',(#1682),#421,.F.);
#17711=ADVANCED_FACE('',(#1683),#422,.F.);
#17712=ADVANCED_FACE('',(#1684),#423,.F.);
#17713=ADVANCED_FACE('',(#1685),#424,.F.);
#17714=ADVANCED_FACE('',(#1686),#425,.F.);
#17715=ADVANCED_FACE('',(#1687),#426,.F.);
#17716=ADVANCED_FACE('',(#1688),#427,.F.);
#17717=ADVANCED_FACE('',(#1689),#428,.F.);
#17718=ADVANCED_FACE('',(#1690),#429,.F.);
#17719=ADVANCED_FACE('',(#1691),#430,.F.);
#17720=ADVANCED_FACE('',(#1692),#431,.F.);
#17721=ADVANCED_FACE('',(#1693),#432,.F.);
#17722=ADVANCED_FACE('',(#1694),#433,.F.);
#17723=ADVANCED_FACE('',(#1695),#434,.F.);
#17724=ADVANCED_FACE('',(#1696),#435,.F.);
#17725=ADVANCED_FACE('',(#1697),#436,.F.);
#17726=ADVANCED_FACE('',(#1698),#437,.F.);
#17727=ADVANCED_FACE('',(#1699),#438,.F.);
#17728=ADVANCED_FACE('',(#1700),#439,.F.);
#17729=ADVANCED_FACE('',(#1701),#440,.F.);
#17730=ADVANCED_FACE('',(#1702),#441,.F.);
#17731=ADVANCED_FACE('',(#1703),#442,.F.);
#17732=ADVANCED_FACE('',(#1704),#443,.F.);
#17733=ADVANCED_FACE('',(#1705),#444,.F.);
#17734=ADVANCED_FACE('',(#1706),#445,.F.);
#17735=ADVANCED_FACE('',(#1707),#446,.F.);
#17736=ADVANCED_FACE('',(#1708),#447,.F.);
#17737=ADVANCED_FACE('',(#1709),#448,.F.);
#17738=ADVANCED_FACE('',(#1710),#449,.F.);
#17739=ADVANCED_FACE('',(#1711),#450,.F.);
#17740=ADVANCED_FACE('',(#1712),#451,.F.);
#17741=ADVANCED_FACE('',(#1713),#452,.F.);
#17742=ADVANCED_FACE('',(#1714),#453,.F.);
#17743=ADVANCED_FACE('',(#1715),#454,.F.);
#17744=ADVANCED_FACE('',(#1716),#455,.F.);
#17745=ADVANCED_FACE('',(#1717),#456,.F.);
#17746=ADVANCED_FACE('',(#1718),#457,.F.);
#17747=ADVANCED_FACE('',(#1719),#458,.F.);
#17748=ADVANCED_FACE('',(#1720),#459,.F.);
#17749=ADVANCED_FACE('',(#1721),#460,.F.);
#17750=ADVANCED_FACE('',(#1722),#461,.F.);
#17751=ADVANCED_FACE('',(#1723),#462,.F.);
#17752=ADVANCED_FACE('',(#1724),#463,.F.);
#17753=ADVANCED_FACE('',(#1725),#464,.F.);
#17754=ADVANCED_FACE('',(#1726),#465,.F.);
#17755=ADVANCED_FACE('',(#1727),#466,.F.);
#17756=ADVANCED_FACE('',(#1728),#467,.F.);
#17757=ADVANCED_FACE('',(#1729),#468,.F.);
#17758=ADVANCED_FACE('',(#1730),#469,.F.);
#17759=ADVANCED_FACE('',(#1731),#470,.F.);
#17760=ADVANCED_FACE('',(#1732),#471,.F.);
#17761=ADVANCED_FACE('',(#1733),#472,.F.);
#17762=ADVANCED_FACE('',(#1734),#473,.F.);
#17763=ADVANCED_FACE('',(#1735),#474,.F.);
#17764=ADVANCED_FACE('',(#1736),#475,.F.);
#17765=ADVANCED_FACE('',(#1737),#476,.F.);
#17766=ADVANCED_FACE('',(#1738),#477,.F.);
#17767=ADVANCED_FACE('',(#1739),#478,.F.);
#17768=ADVANCED_FACE('',(#1740),#479,.F.);
#17769=ADVANCED_FACE('',(#1741),#480,.F.);
#17770=ADVANCED_FACE('',(#1742),#481,.F.);
#17771=ADVANCED_FACE('',(#1743),#482,.F.);
#17772=ADVANCED_FACE('',(#1744),#483,.F.);
#17773=ADVANCED_FACE('',(#1745),#484,.F.);
#17774=ADVANCED_FACE('',(#1746),#485,.F.);
#17775=ADVANCED_FACE('',(#1747),#486,.F.);
#17776=ADVANCED_FACE('',(#1748),#487,.F.);
#17777=ADVANCED_FACE('',(#1749),#488,.F.);
#17778=ADVANCED_FACE('',(#1750),#489,.F.);
#17779=ADVANCED_FACE('',(#1751),#490,.F.);
#17780=ADVANCED_FACE('',(#1752),#491,.F.);
#17781=ADVANCED_FACE('',(#1753),#492,.F.);
#17782=ADVANCED_FACE('',(#1754),#493,.F.);
#17783=ADVANCED_FACE('',(#1755),#494,.F.);
#17784=ADVANCED_FACE('',(#1756),#495,.F.);
#17785=ADVANCED_FACE('',(#1757),#496,.F.);
#17786=ADVANCED_FACE('',(#1758),#497,.F.);
#17787=ADVANCED_FACE('',(#1759),#498,.F.);
#17788=ADVANCED_FACE('',(#1760),#499,.F.);
#17789=ADVANCED_FACE('',(#1761),#500,.F.);
#17790=ADVANCED_FACE('',(#1762),#501,.F.);
#17791=ADVANCED_FACE('',(#1763),#502,.F.);
#17792=ADVANCED_FACE('',(#1764),#503,.F.);
#17793=ADVANCED_FACE('',(#1765),#504,.F.);
#17794=ADVANCED_FACE('',(#1766),#505,.F.);
#17795=ADVANCED_FACE('',(#1767),#506,.F.);
#17796=ADVANCED_FACE('',(#1768),#507,.F.);
#17797=ADVANCED_FACE('',(#1769),#508,.F.);
#17798=ADVANCED_FACE('',(#1770),#509,.F.);
#17799=ADVANCED_FACE('',(#1771),#510,.F.);
#17800=ADVANCED_FACE('',(#1772),#511,.F.);
#17801=ADVANCED_FACE('',(#1773),#512,.F.);
#17802=ADVANCED_FACE('',(#1774),#513,.F.);
#17803=ADVANCED_FACE('',(#1775),#514,.F.);
#17804=ADVANCED_FACE('',(#1776),#515,.F.);
#17805=ADVANCED_FACE('',(#1777),#516,.F.);
#17806=ADVANCED_FACE('',(#1778),#517,.F.);
#17807=ADVANCED_FACE('',(#1779),#518,.F.);
#17808=ADVANCED_FACE('',(#1780),#519,.F.);
#17809=ADVANCED_FACE('',(#1781),#520,.F.);
#17810=ADVANCED_FACE('',(#1782),#521,.F.);
#17811=ADVANCED_FACE('',(#1783),#522,.F.);
#17812=ADVANCED_FACE('',(#1784),#523,.F.);
#17813=ADVANCED_FACE('',(#1785),#524,.F.);
#17814=ADVANCED_FACE('',(#1786),#525,.F.);
#17815=ADVANCED_FACE('',(#1787),#526,.F.);
#17816=ADVANCED_FACE('',(#1788),#527,.F.);
#17817=ADVANCED_FACE('',(#1789),#528,.F.);
#17818=ADVANCED_FACE('',(#1790),#529,.F.);
#17819=ADVANCED_FACE('',(#1791),#530,.F.);
#17820=ADVANCED_FACE('',(#1792),#531,.F.);
#17821=ADVANCED_FACE('',(#1793),#532,.F.);
#17822=ADVANCED_FACE('',(#1794),#533,.F.);
#17823=ADVANCED_FACE('',(#1795),#534,.F.);
#17824=ADVANCED_FACE('',(#1796),#535,.F.);
#17825=ADVANCED_FACE('',(#1797),#536,.F.);
#17826=ADVANCED_FACE('',(#1798),#537,.F.);
#17827=ADVANCED_FACE('',(#1799),#538,.F.);
#17828=ADVANCED_FACE('',(#1800),#539,.F.);
#17829=ADVANCED_FACE('',(#1801),#540,.F.);
#17830=ADVANCED_FACE('',(#1802),#541,.F.);
#17831=ADVANCED_FACE('',(#1803),#542,.F.);
#17832=ADVANCED_FACE('',(#1804),#543,.F.);
#17833=ADVANCED_FACE('',(#1805),#544,.F.);
#17834=ADVANCED_FACE('',(#1806),#545,.F.);
#17835=ADVANCED_FACE('',(#1807),#546,.F.);
#17836=ADVANCED_FACE('',(#1808),#547,.F.);
#17837=ADVANCED_FACE('',(#1809),#548,.F.);
#17838=ADVANCED_FACE('',(#1810),#549,.F.);
#17839=ADVANCED_FACE('',(#1811),#550,.F.);
#17840=ADVANCED_FACE('',(#1812),#551,.F.);
#17841=ADVANCED_FACE('',(#1813),#552,.F.);
#17842=ADVANCED_FACE('',(#1814),#553,.F.);
#17843=ADVANCED_FACE('',(#1815),#554,.F.);
#17844=ADVANCED_FACE('',(#1816),#555,.F.);
#17845=ADVANCED_FACE('',(#1817),#556,.F.);
#17846=ADVANCED_FACE('',(#1818),#557,.F.);
#17847=ADVANCED_FACE('',(#1819),#558,.F.);
#17848=ADVANCED_FACE('',(#1820),#559,.F.);
#17849=ADVANCED_FACE('',(#1821),#560,.F.);
#17850=ADVANCED_FACE('',(#1822),#561,.F.);
#17851=ADVANCED_FACE('',(#1823),#562,.F.);
#17852=ADVANCED_FACE('',(#1824),#563,.F.);
#17853=ADVANCED_FACE('',(#1825),#564,.F.);
#17854=ADVANCED_FACE('',(#1826),#565,.F.);
#17855=ADVANCED_FACE('',(#1827),#566,.F.);
#17856=ADVANCED_FACE('',(#1828),#567,.F.);
#17857=ADVANCED_FACE('',(#1829),#568,.F.);
#17858=ADVANCED_FACE('',(#1830),#569,.F.);
#17859=ADVANCED_FACE('',(#1831),#570,.F.);
#17860=ADVANCED_FACE('',(#1832),#571,.F.);
#17861=ADVANCED_FACE('',(#1833),#572,.F.);
#17862=ADVANCED_FACE('',(#1834),#573,.F.);
#17863=ADVANCED_FACE('',(#1835),#574,.F.);
#17864=ADVANCED_FACE('',(#1836),#575,.F.);
#17865=ADVANCED_FACE('',(#1837),#576,.F.);
#17866=ADVANCED_FACE('',(#1838),#577,.F.);
#17867=ADVANCED_FACE('',(#1839),#578,.F.);
#17868=ADVANCED_FACE('',(#1840),#579,.F.);
#17869=ADVANCED_FACE('',(#1841),#580,.F.);
#17870=ADVANCED_FACE('',(#1842),#581,.F.);
#17871=ADVANCED_FACE('',(#1843),#582,.F.);
#17872=ADVANCED_FACE('',(#1844),#583,.F.);
#17873=ADVANCED_FACE('',(#1845),#584,.F.);
#17874=ADVANCED_FACE('',(#1846),#585,.F.);
#17875=ADVANCED_FACE('',(#1847),#586,.F.);
#17876=ADVANCED_FACE('',(#1848),#587,.F.);
#17877=ADVANCED_FACE('',(#1849),#588,.F.);
#17878=ADVANCED_FACE('',(#1850),#589,.F.);
#17879=ADVANCED_FACE('',(#1851),#590,.F.);
#17880=ADVANCED_FACE('',(#1852),#17301,.F.);
#17881=ADVANCED_FACE('',(#1853),#591,.T.);
#17882=ADVANCED_FACE('',(#1854),#17302,.F.);
#17883=ADVANCED_FACE('',(#1855),#592,.F.);
#17884=ADVANCED_FACE('',(#1856),#17303,.F.);
#17885=ADVANCED_FACE('',(#1857),#593,.F.);
#17886=ADVANCED_FACE('',(#1858),#17304,.F.);
#17887=ADVANCED_FACE('',(#1859),#594,.F.);
#17888=ADVANCED_FACE('',(#1860),#17305,.F.);
#17889=ADVANCED_FACE('',(#1861),#595,.F.);
#17890=ADVANCED_FACE('',(#1862),#17306,.F.);
#17891=ADVANCED_FACE('',(#1863),#596,.F.);
#17892=ADVANCED_FACE('',(#1864),#17307,.F.);
#17893=ADVANCED_FACE('',(#1865),#597,.F.);
#17894=ADVANCED_FACE('',(#1866),#17308,.T.);
#17895=ADVANCED_FACE('',(#1867,#229),#598,.F.);
#17896=ADVANCED_FACE('',(#1868,#230),#599,.F.);
#17897=ADVANCED_FACE('',(#1869),#17309,.T.);
#17898=ADVANCED_FACE('',(#1870),#915,.T.);
#17899=ADVANCED_FACE('',(#1871),#17310,.T.);
#17900=ADVANCED_FACE('',(#1872,#231,#232,#233,#234,#235,#236,#237),#600,
 .T.);
#17901=ADVANCED_FACE('',(#1873),#916,.T.);
#17902=ADVANCED_FACE('',(#1874),#17311,.T.);
#17903=ADVANCED_FACE('',(#1875),#917,.T.);
#17904=ADVANCED_FACE('',(#1876,#238),#601,.T.);
#17905=ADVANCED_FACE('',(#1877),#918,.T.);
#17906=ADVANCED_FACE('',(#1878),#17312,.T.);
#17907=ADVANCED_FACE('',(#1879),#919,.T.);
#17908=ADVANCED_FACE('',(#1880,#239),#602,.T.);
#17909=ADVANCED_FACE('',(#1881),#920,.F.);
#17910=ADVANCED_FACE('',(#1882),#17313,.F.);
#17911=ADVANCED_FACE('',(#1883),#921,.F.);
#17912=ADVANCED_FACE('',(#1884,#240),#603,.T.);
#17913=ADVANCED_FACE('',(#1885),#127,.T.);
#17914=ADVANCED_FACE('',(#1886),#604,.T.);
#17915=ADVANCED_FACE('',(#1887),#1080,.T.);
#17916=ADVANCED_FACE('',(#1888),#128,.T.);
#17917=ADVANCED_FACE('',(#1889),#129,.T.);
#17918=ADVANCED_FACE('',(#1890),#1081,.T.);
#17919=ADVANCED_FACE('',(#1891),#130,.T.);
#17920=ADVANCED_FACE('',(#1892),#605,.T.);
#17921=ADVANCED_FACE('',(#1893),#606,.T.);
#17922=ADVANCED_FACE('',(#1894),#607,.F.);
#17923=ADVANCED_FACE('',(#1895),#1082,.T.);
#17924=ADVANCED_FACE('',(#1896),#922,.T.);
#17925=ADVANCED_FACE('',(#1897),#17314,.T.);
#17926=ADVANCED_FACE('',(#1898),#923,.T.);
#17927=ADVANCED_FACE('',(#1899),#924,.T.);
#17928=ADVANCED_FACE('',(#1900),#925,.T.);
#17929=ADVANCED_FACE('',(#1901),#926,.T.);
#17930=ADVANCED_FACE('',(#1902),#927,.T.);
#17931=ADVANCED_FACE('',(#1903),#928,.T.);
#17932=ADVANCED_FACE('',(#1904),#929,.T.);
#17933=ADVANCED_FACE('',(#1905),#930,.T.);
#17934=ADVANCED_FACE('',(#1906),#931,.T.);
#17935=ADVANCED_FACE('',(#1907),#932,.T.);
#17936=ADVANCED_FACE('',(#1908),#933,.T.);
#17937=ADVANCED_FACE('',(#1909),#934,.T.);
#17938=ADVANCED_FACE('',(#1910),#935,.T.);
#17939=ADVANCED_FACE('',(#1911),#936,.F.);
#17940=ADVANCED_FACE('',(#1912),#17315,.F.);
#17941=ADVANCED_FACE('',(#1913,#241),#608,.T.);
#17942=ADVANCED_FACE('',(#1914),#937,.F.);
#17943=ADVANCED_FACE('',(#1915,#242),#609,.T.);
#17944=ADVANCED_FACE('',(#1916),#131,.F.);
#17945=ADVANCED_FACE('',(#1917),#610,.T.);
#17946=ADVANCED_FACE('',(#1918),#1083,.T.);
#17947=ADVANCED_FACE('',(#1919),#132,.T.);
#17948=ADVANCED_FACE('',(#1920),#938,.T.);
#17949=ADVANCED_FACE('',(#1921),#133,.F.);
#17950=ADVANCED_FACE('',(#1922),#611,.T.);
#17951=ADVANCED_FACE('',(#1923),#1084,.T.);
#17952=ADVANCED_FACE('',(#1924),#134,.T.);
#17953=ADVANCED_FACE('',(#1925),#939,.T.);
#17954=ADVANCED_FACE('',(#1926),#135,.F.);
#17955=ADVANCED_FACE('',(#1927),#612,.T.);
#17956=ADVANCED_FACE('',(#1928),#1085,.T.);
#17957=ADVANCED_FACE('',(#1929),#136,.T.);
#17958=ADVANCED_FACE('',(#1930),#940,.T.);
#17959=ADVANCED_FACE('',(#1931),#137,.F.);
#17960=ADVANCED_FACE('',(#1932),#613,.T.);
#17961=ADVANCED_FACE('',(#1933),#1086,.T.);
#17962=ADVANCED_FACE('',(#1934),#138,.T.);
#17963=ADVANCED_FACE('',(#1935),#941,.T.);
#17964=ADVANCED_FACE('',(#1936),#139,.F.);
#17965=ADVANCED_FACE('',(#1937),#614,.T.);
#17966=ADVANCED_FACE('',(#1938),#1087,.T.);
#17967=ADVANCED_FACE('',(#1939),#140,.T.);
#17968=ADVANCED_FACE('',(#1940),#942,.T.);
#17969=ADVANCED_FACE('',(#1941),#141,.F.);
#17970=ADVANCED_FACE('',(#1942),#615,.T.);
#17971=ADVANCED_FACE('',(#1943),#1088,.T.);
#17972=ADVANCED_FACE('',(#1944),#142,.T.);
#17973=ADVANCED_FACE('',(#1945),#943,.T.);
#17974=ADVANCED_FACE('',(#1946),#143,.F.);
#17975=ADVANCED_FACE('',(#1947),#616,.T.);
#17976=ADVANCED_FACE('',(#1948),#1089,.T.);
#17977=ADVANCED_FACE('',(#1949),#144,.T.);
#17978=ADVANCED_FACE('',(#1950),#944,.T.);
#17979=ADVANCED_FACE('',(#1951),#145,.F.);
#17980=ADVANCED_FACE('',(#1952),#617,.T.);
#17981=ADVANCED_FACE('',(#1953),#1090,.T.);
#17982=ADVANCED_FACE('',(#1954),#146,.T.);
#17983=ADVANCED_FACE('',(#1955),#945,.T.);
#17984=ADVANCED_FACE('',(#1956),#147,.F.);
#17985=ADVANCED_FACE('',(#1957),#618,.T.);
#17986=ADVANCED_FACE('',(#1958),#1091,.T.);
#17987=ADVANCED_FACE('',(#1959),#148,.T.);
#17988=ADVANCED_FACE('',(#1960),#946,.T.);
#17989=ADVANCED_FACE('',(#1961),#149,.F.);
#17990=ADVANCED_FACE('',(#1962),#619,.T.);
#17991=ADVANCED_FACE('',(#1963),#1092,.T.);
#17992=ADVANCED_FACE('',(#1964),#150,.T.);
#17993=ADVANCED_FACE('',(#1965),#947,.T.);
#17994=ADVANCED_FACE('',(#1966),#151,.F.);
#17995=ADVANCED_FACE('',(#1967),#620,.T.);
#17996=ADVANCED_FACE('',(#1968),#1093,.T.);
#17997=ADVANCED_FACE('',(#1969),#152,.T.);
#17998=ADVANCED_FACE('',(#1970),#948,.T.);
#17999=ADVANCED_FACE('',(#1971),#153,.F.);
#18000=ADVANCED_FACE('',(#1972),#621,.T.);
#18001=ADVANCED_FACE('',(#1973),#1094,.T.);
#18002=ADVANCED_FACE('',(#1974),#154,.T.);
#18003=ADVANCED_FACE('',(#1975),#949,.T.);
#18004=ADVANCED_FACE('',(#1976),#155,.F.);
#18005=ADVANCED_FACE('',(#1977),#622,.T.);
#18006=ADVANCED_FACE('',(#1978),#1095,.T.);
#18007=ADVANCED_FACE('',(#1979),#156,.T.);
#18008=ADVANCED_FACE('',(#1980),#950,.T.);
#18009=ADVANCED_FACE('',(#1981),#1096,.T.);
#18010=ADVANCED_FACE('',(#1982),#157,.F.);
#18011=ADVANCED_FACE('',(#1983),#623,.T.);
#18012=ADVANCED_FACE('',(#1984),#1097,.T.);
#18013=ADVANCED_FACE('',(#1985),#158,.T.);
#18014=ADVANCED_FACE('',(#1986),#951,.T.);
#18015=ADVANCED_FACE('',(#1987),#952,.T.);
#18016=ADVANCED_FACE('',(#1988),#953,.T.);
#18017=ADVANCED_FACE('',(#1989),#17316,.T.);
#18018=ADVANCED_FACE('',(#1990),#954,.T.);
#18019=ADVANCED_FACE('',(#1991),#624,.T.);
#18020=ADVANCED_FACE('',(#1992),#625,.T.);
#18021=ADVANCED_FACE('',(#1993),#159,.T.);
#18022=ADVANCED_FACE('',(#1994),#626,.T.);
#18023=ADVANCED_FACE('',(#1995),#627,.T.);
#18024=ADVANCED_FACE('',(#1996),#160,.T.);
#18025=ADVANCED_FACE('',(#1997),#628,.T.);
#18026=ADVANCED_FACE('',(#1998),#629,.T.);
#18027=ADVANCED_FACE('',(#1999),#161,.T.);
#18028=ADVANCED_FACE('',(#2000),#630,.T.);
#18029=ADVANCED_FACE('',(#2001),#631,.T.);
#18030=ADVANCED_FACE('',(#2002),#955,.T.);
#18031=ADVANCED_FACE('',(#2003),#632,.T.);
#18032=ADVANCED_FACE('',(#2004),#633,.T.);
#18033=ADVANCED_FACE('',(#2005),#634,.T.);
#18034=ADVANCED_FACE('',(#2006),#635,.T.);
#18035=ADVANCED_FACE('',(#2007),#162,.T.);
#18036=ADVANCED_FACE('',(#2008),#163,.T.);
#18037=ADVANCED_FACE('',(#2009),#636,.T.);
#18038=ADVANCED_FACE('',(#2010),#637,.T.);
#18039=ADVANCED_FACE('',(#2011),#164,.T.);
#18040=ADVANCED_FACE('',(#2012),#165,.T.);
#18041=ADVANCED_FACE('',(#2013),#638,.T.);
#18042=ADVANCED_FACE('',(#2014),#639,.T.);
#18043=ADVANCED_FACE('',(#2015),#166,.T.);
#18044=ADVANCED_FACE('',(#2016),#640,.T.);
#18045=ADVANCED_FACE('',(#2017),#641,.T.);
#18046=ADVANCED_FACE('',(#2018),#167,.T.);
#18047=ADVANCED_FACE('',(#2019),#168,.T.);
#18048=ADVANCED_FACE('',(#2020),#642,.T.);
#18049=ADVANCED_FACE('',(#2021),#643,.T.);
#18050=ADVANCED_FACE('',(#2022),#169,.T.);
#18051=ADVANCED_FACE('',(#2023),#170,.T.);
#18052=ADVANCED_FACE('',(#2024),#644,.T.);
#18053=ADVANCED_FACE('',(#2025),#645,.T.);
#18054=ADVANCED_FACE('',(#2026),#171,.T.);
#18055=ADVANCED_FACE('',(#2027),#172,.T.);
#18056=ADVANCED_FACE('',(#2028),#646,.T.);
#18057=ADVANCED_FACE('',(#2029),#647,.T.);
#18058=ADVANCED_FACE('',(#2030),#173,.T.);
#18059=ADVANCED_FACE('',(#2031),#174,.T.);
#18060=ADVANCED_FACE('',(#2032),#175,.T.);
#18061=ADVANCED_FACE('',(#2033),#176,.T.);
#18062=ADVANCED_FACE('',(#2034),#177,.T.);
#18063=ADVANCED_FACE('',(#2035),#178,.T.);
#18064=ADVANCED_FACE('',(#2036),#179,.T.);
#18065=ADVANCED_FACE('',(#2037),#180,.T.);
#18066=ADVANCED_FACE('',(#2038),#181,.T.);
#18067=ADVANCED_FACE('',(#2039),#182,.T.);
#18068=ADVANCED_FACE('',(#2040),#183,.T.);
#18069=ADVANCED_FACE('',(#2041),#184,.T.);
#18070=ADVANCED_FACE('',(#2042),#185,.T.);
#18071=ADVANCED_FACE('',(#2043),#186,.T.);
#18072=ADVANCED_FACE('',(#2044),#187,.T.);
#18073=ADVANCED_FACE('',(#2045),#188,.T.);
#18074=ADVANCED_FACE('',(#2046),#189,.T.);
#18075=ADVANCED_FACE('',(#2047),#190,.T.);
#18076=ADVANCED_FACE('',(#2048),#191,.T.);
#18077=ADVANCED_FACE('',(#2049),#192,.T.);
#18078=ADVANCED_FACE('',(#2050),#193,.T.);
#18079=ADVANCED_FACE('',(#2051),#194,.T.);
#18080=ADVANCED_FACE('',(#2052),#195,.T.);
#18081=ADVANCED_FACE('',(#2053),#196,.T.);
#18082=ADVANCED_FACE('',(#2054),#648,.T.);
#18083=ADVANCED_FACE('',(#2055),#649,.T.);
#18084=ADVANCED_FACE('',(#2056),#650,.T.);
#18085=ADVANCED_FACE('',(#2057),#651,.T.);
#18086=ADVANCED_FACE('',(#2058,#243),#652,.T.);
#18087=ADVANCED_FACE('',(#2059),#956,.T.);
#18088=ADVANCED_FACE('',(#2060),#957,.T.);
#18089=ADVANCED_FACE('',(#2061),#958,.T.);
#18090=ADVANCED_FACE('',(#2062),#959,.T.);
#18091=ADVANCED_FACE('',(#2063),#960,.T.);
#18092=ADVANCED_FACE('',(#2064),#961,.T.);
#18093=ADVANCED_FACE('',(#2065),#962,.T.);
#18094=ADVANCED_FACE('',(#2066),#963,.T.);
#18095=ADVANCED_FACE('',(#2067),#964,.F.);
#18096=ADVANCED_FACE('',(#2068),#965,.F.);
#18097=ADVANCED_FACE('',(#2069),#653,.T.);
#18098=ADVANCED_FACE('',(#2070),#654,.T.);
#18099=ADVANCED_FACE('',(#2071),#655,.T.);
#18100=ADVANCED_FACE('',(#2072),#656,.T.);
#18101=ADVANCED_FACE('',(#2073),#657,.T.);
#18102=ADVANCED_FACE('',(#2074),#658,.T.);
#18103=ADVANCED_FACE('',(#2075),#659,.T.);
#18104=ADVANCED_FACE('',(#2076),#660,.T.);
#18105=ADVANCED_FACE('',(#2077),#17317,.F.);
#18106=ADVANCED_FACE('',(#2078,#244),#661,.T.);
#18107=ADVANCED_FACE('',(#2079),#966,.T.);
#18108=ADVANCED_FACE('',(#2080),#17318,.T.);
#18109=ADVANCED_FACE('',(#2081),#967,.T.);
#18110=ADVANCED_FACE('',(#2082,#245),#662,.T.);
#18111=ADVANCED_FACE('',(#2083),#663,.T.);
#18112=ADVANCED_FACE('',(#2084),#17319,.F.);
#18113=ADVANCED_FACE('',(#2085),#664,.F.);
#18114=ADVANCED_FACE('',(#2086),#665,.T.);
#18115=ADVANCED_FACE('',(#2087),#17320,.F.);
#18116=ADVANCED_FACE('',(#2088),#666,.F.);
#18117=ADVANCED_FACE('',(#2089),#667,.T.);
#18118=ADVANCED_FACE('',(#2090),#17321,.F.);
#18119=ADVANCED_FACE('',(#2091),#668,.F.);
#18120=ADVANCED_FACE('',(#2092),#669,.T.);
#18121=ADVANCED_FACE('',(#2093),#17322,.F.);
#18122=ADVANCED_FACE('',(#2094),#670,.F.);
#18123=ADVANCED_FACE('',(#2095),#17323,.F.);
#18124=ADVANCED_FACE('',(#2096),#17324,.F.);
#18125=ADVANCED_FACE('',(#2097),#17325,.F.);
#18126=ADVANCED_FACE('',(#2098),#17326,.F.);
#18127=ADVANCED_FACE('',(#2099,#246,#247,#248),#17327,.T.);
#18128=ADVANCED_FACE('',(#2100,#249),#671,.F.);
#18129=ADVANCED_FACE('',(#2101,#250),#672,.F.);
#18130=ADVANCED_FACE('',(#2102),#17328,.T.);
#18131=ADVANCED_FACE('',(#2103),#968,.T.);
#18132=ADVANCED_FACE('',(#2104),#17329,.T.);
#18133=ADVANCED_FACE('',(#2105),#969,.T.);
#18134=ADVANCED_FACE('',(#2106,#251),#673,.T.);
#18135=ADVANCED_FACE('',(#2107),#970,.F.);
#18136=ADVANCED_FACE('',(#2108,#252,#253,#254,#255,#256,#257,#258),#17330,
 .F.);
#18137=ADVANCED_FACE('',(#2109),#971,.F.);
#18138=ADVANCED_FACE('',(#2110,#259),#674,.T.);
#18139=ADVANCED_FACE('',(#2111),#972,.F.);
#18140=ADVANCED_FACE('',(#2112),#17331,.F.);
#18141=ADVANCED_FACE('',(#2113,#260,#261),#675,.F.);
#18142=ADVANCED_FACE('',(#2114),#973,.F.);
#18143=ADVANCED_FACE('',(#2115,#262,#263),#676,.T.);
#18144=ADVANCED_FACE('',(#2116),#974,.F.);
#18145=ADVANCED_FACE('',(#2117),#17332,.F.);
#18146=ADVANCED_FACE('',(#2118),#975,.F.);
#18147=ADVANCED_FACE('',(#2119),#677,.T.);
#18148=ADVANCED_FACE('',(#2120),#678,.T.);
#18149=ADVANCED_FACE('',(#2121),#679,.T.);
#18150=ADVANCED_FACE('',(#2122),#680,.T.);
#18151=ADVANCED_FACE('',(#2123),#681,.T.);
#18152=ADVANCED_FACE('',(#2124),#682,.T.);
#18153=ADVANCED_FACE('',(#2125),#683,.T.);
#18154=ADVANCED_FACE('',(#2126),#684,.T.);
#18155=ADVANCED_FACE('',(#2127),#685,.T.);
#18156=ADVANCED_FACE('',(#2128),#686,.T.);
#18157=ADVANCED_FACE('',(#2129),#687,.T.);
#18158=ADVANCED_FACE('',(#2130),#688,.T.);
#18159=ADVANCED_FACE('',(#2131),#689,.T.);
#18160=ADVANCED_FACE('',(#2132),#690,.T.);
#18161=ADVANCED_FACE('',(#2133),#691,.T.);
#18162=ADVANCED_FACE('',(#2134),#692,.T.);
#18163=ADVANCED_FACE('',(#2135),#693,.T.);
#18164=ADVANCED_FACE('',(#2136),#694,.T.);
#18165=ADVANCED_FACE('',(#2137),#695,.T.);
#18166=ADVANCED_FACE('',(#2138),#696,.T.);
#18167=ADVANCED_FACE('',(#2139),#697,.T.);
#18168=ADVANCED_FACE('',(#2140),#698,.T.);
#18169=ADVANCED_FACE('',(#2141),#699,.T.);
#18170=ADVANCED_FACE('',(#2142),#700,.T.);
#18171=ADVANCED_FACE('',(#2143),#701,.T.);
#18172=ADVANCED_FACE('',(#2144),#702,.T.);
#18173=ADVANCED_FACE('',(#2145),#703,.T.);
#18174=ADVANCED_FACE('',(#2146),#704,.T.);
#18175=ADVANCED_FACE('',(#2147),#705,.T.);
#18176=ADVANCED_FACE('',(#2148),#706,.T.);
#18177=ADVANCED_FACE('',(#2149),#707,.T.);
#18178=ADVANCED_FACE('',(#2150),#708,.T.);
#18179=ADVANCED_FACE('',(#2151),#709,.T.);
#18180=ADVANCED_FACE('',(#2152),#710,.T.);
#18181=ADVANCED_FACE('',(#2153),#711,.T.);
#18182=ADVANCED_FACE('',(#2154),#712,.T.);
#18183=ADVANCED_FACE('',(#2155),#713,.T.);
#18184=ADVANCED_FACE('',(#2156),#714,.T.);
#18185=ADVANCED_FACE('',(#2157),#715,.T.);
#18186=ADVANCED_FACE('',(#2158),#716,.T.);
#18187=ADVANCED_FACE('',(#2159),#717,.T.);
#18188=ADVANCED_FACE('',(#2160),#718,.T.);
#18189=ADVANCED_FACE('',(#2161),#719,.T.);
#18190=ADVANCED_FACE('',(#2162),#720,.T.);
#18191=ADVANCED_FACE('',(#2163),#721,.T.);
#18192=ADVANCED_FACE('',(#2164),#722,.T.);
#18193=ADVANCED_FACE('',(#2165),#723,.T.);
#18194=ADVANCED_FACE('',(#2166),#724,.T.);
#18195=ADVANCED_FACE('',(#2167),#725,.T.);
#18196=ADVANCED_FACE('',(#2168),#726,.T.);
#18197=ADVANCED_FACE('',(#2169),#727,.T.);
#18198=ADVANCED_FACE('',(#2170),#728,.T.);
#18199=ADVANCED_FACE('',(#2171),#729,.T.);
#18200=ADVANCED_FACE('',(#2172),#730,.T.);
#18201=ADVANCED_FACE('',(#2173),#731,.T.);
#18202=ADVANCED_FACE('',(#2174),#732,.T.);
#18203=ADVANCED_FACE('',(#2175),#733,.T.);
#18204=ADVANCED_FACE('',(#2176),#734,.T.);
#18205=ADVANCED_FACE('',(#2177),#735,.T.);
#18206=ADVANCED_FACE('',(#2178),#736,.T.);
#18207=ADVANCED_FACE('',(#2179),#737,.T.);
#18208=ADVANCED_FACE('',(#2180),#738,.T.);
#18209=ADVANCED_FACE('',(#2181),#739,.T.);
#18210=ADVANCED_FACE('',(#2182),#740,.T.);
#18211=ADVANCED_FACE('',(#2183),#741,.T.);
#18212=ADVANCED_FACE('',(#2184),#742,.T.);
#18213=ADVANCED_FACE('',(#2185),#743,.T.);
#18214=ADVANCED_FACE('',(#2186),#744,.T.);
#18215=ADVANCED_FACE('',(#2187),#745,.T.);
#18216=ADVANCED_FACE('',(#2188),#746,.T.);
#18217=ADVANCED_FACE('',(#2189),#747,.T.);
#18218=ADVANCED_FACE('',(#2190),#748,.T.);
#18219=ADVANCED_FACE('',(#2191),#749,.T.);
#18220=ADVANCED_FACE('',(#2192),#750,.T.);
#18221=ADVANCED_FACE('',(#2193),#751,.T.);
#18222=ADVANCED_FACE('',(#2194),#752,.T.);
#18223=ADVANCED_FACE('',(#2195),#753,.T.);
#18224=ADVANCED_FACE('',(#2196),#754,.T.);
#18225=ADVANCED_FACE('',(#2197),#755,.T.);
#18226=ADVANCED_FACE('',(#2198),#756,.T.);
#18227=ADVANCED_FACE('',(#2199),#757,.T.);
#18228=ADVANCED_FACE('',(#2200),#758,.T.);
#18229=ADVANCED_FACE('',(#2201),#759,.T.);
#18230=ADVANCED_FACE('',(#2202),#760,.T.);
#18231=ADVANCED_FACE('',(#2203),#761,.T.);
#18232=ADVANCED_FACE('',(#2204),#762,.T.);
#18233=ADVANCED_FACE('',(#2205),#763,.T.);
#18234=ADVANCED_FACE('',(#2206),#764,.T.);
#18235=ADVANCED_FACE('',(#2207),#765,.T.);
#18236=ADVANCED_FACE('',(#2208),#766,.T.);
#18237=ADVANCED_FACE('',(#2209),#767,.T.);
#18238=ADVANCED_FACE('',(#2210),#768,.T.);
#18239=ADVANCED_FACE('',(#2211),#769,.T.);
#18240=ADVANCED_FACE('',(#2212),#770,.T.);
#18241=ADVANCED_FACE('',(#2213),#771,.T.);
#18242=ADVANCED_FACE('',(#2214),#772,.T.);
#18243=ADVANCED_FACE('',(#2215),#773,.T.);
#18244=ADVANCED_FACE('',(#2216),#774,.T.);
#18245=ADVANCED_FACE('',(#2217),#775,.T.);
#18246=ADVANCED_FACE('',(#2218),#776,.T.);
#18247=ADVANCED_FACE('',(#2219),#777,.T.);
#18248=ADVANCED_FACE('',(#2220),#778,.T.);
#18249=ADVANCED_FACE('',(#2221),#779,.T.);
#18250=ADVANCED_FACE('',(#2222),#780,.T.);
#18251=ADVANCED_FACE('',(#2223),#781,.T.);
#18252=ADVANCED_FACE('',(#2224),#782,.T.);
#18253=ADVANCED_FACE('',(#2225),#783,.T.);
#18254=ADVANCED_FACE('',(#2226),#784,.T.);
#18255=ADVANCED_FACE('',(#2227),#785,.T.);
#18256=ADVANCED_FACE('',(#2228),#786,.T.);
#18257=ADVANCED_FACE('',(#2229),#787,.T.);
#18258=ADVANCED_FACE('',(#2230),#788,.T.);
#18259=ADVANCED_FACE('',(#2231),#789,.T.);
#18260=ADVANCED_FACE('',(#2232),#790,.T.);
#18261=ADVANCED_FACE('',(#2233),#791,.T.);
#18262=ADVANCED_FACE('',(#2234),#792,.T.);
#18263=ADVANCED_FACE('',(#2235),#793,.T.);
#18264=ADVANCED_FACE('',(#2236),#794,.T.);
#18265=ADVANCED_FACE('',(#2237),#795,.T.);
#18266=ADVANCED_FACE('',(#2238),#796,.T.);
#18267=ADVANCED_FACE('',(#2239),#797,.T.);
#18268=ADVANCED_FACE('',(#2240),#798,.T.);
#18269=ADVANCED_FACE('',(#2241),#799,.T.);
#18270=ADVANCED_FACE('',(#2242),#800,.T.);
#18271=ADVANCED_FACE('',(#2243),#801,.T.);
#18272=ADVANCED_FACE('',(#2244),#802,.T.);
#18273=ADVANCED_FACE('',(#2245),#803,.T.);
#18274=ADVANCED_FACE('',(#2246),#804,.T.);
#18275=ADVANCED_FACE('',(#2247),#805,.T.);
#18276=ADVANCED_FACE('',(#2248),#806,.T.);
#18277=ADVANCED_FACE('',(#2249),#807,.T.);
#18278=ADVANCED_FACE('',(#2250),#808,.T.);
#18279=ADVANCED_FACE('',(#2251),#809,.T.);
#18280=ADVANCED_FACE('',(#2252),#810,.T.);
#18281=ADVANCED_FACE('',(#2253),#811,.T.);
#18282=ADVANCED_FACE('',(#2254),#812,.T.);
#18283=ADVANCED_FACE('',(#2255),#813,.T.);
#18284=ADVANCED_FACE('',(#2256),#814,.T.);
#18285=ADVANCED_FACE('',(#2257),#815,.T.);
#18286=ADVANCED_FACE('',(#2258),#816,.T.);
#18287=ADVANCED_FACE('',(#2259),#817,.T.);
#18288=ADVANCED_FACE('',(#2260),#818,.T.);
#18289=ADVANCED_FACE('',(#2261),#819,.T.);
#18290=ADVANCED_FACE('',(#2262),#820,.T.);
#18291=ADVANCED_FACE('',(#2263),#821,.T.);
#18292=ADVANCED_FACE('',(#2264),#822,.T.);
#18293=ADVANCED_FACE('',(#2265),#823,.T.);
#18294=ADVANCED_FACE('',(#2266),#824,.T.);
#18295=ADVANCED_FACE('',(#2267),#825,.T.);
#18296=ADVANCED_FACE('',(#2268),#826,.T.);
#18297=CLOSED_SHELL('',(#17333,#17334,#17335,#17336,#17337,#17338,#17339,
#17340,#17341,#17342,#17343,#17344,#17345,#17346,#17347,#17348,#17349,#17350,
#17351,#17352,#17353,#17354,#17355,#17356,#17357,#17358,#17359,#17360,#17361,
#17362,#17363,#17364,#17365,#17366,#17367,#17368,#17369,#17370,#17371,#17372,
#17373,#17374,#17375,#17376,#17377,#17378,#17379,#17380,#17381,#17382,#17383,
#17384,#17385,#17386,#17387,#17388,#17389,#17390,#17391,#17392,#17393,#17394,
#17395,#17396,#17397,#17398,#17399,#17400,#17401,#17402,#17403,#17404,#17405,
#17406,#17407,#17408,#17409,#17410,#17411,#17412,#17413,#17414,#17415,#17416,
#17417,#17418,#17419,#17420,#17421,#17422,#17423,#17424,#17425,#17426,#17427,
#17428,#17429,#17430,#17431,#17432,#17433,#17434,#17435,#17436,#17437,#17438,
#17439,#17440,#17441,#17442,#17443,#17444,#17445,#17446,#17447,#17448,#17449,
#17450,#17451,#17452,#17453,#17454,#17455,#17456,#17457,#17458,#17459,#17460,
#17461,#17462,#17463,#17464,#17465,#17466,#17467,#17468,#17469,#17470,#17471,
#17472,#17473,#17474,#17475,#17476,#17477,#17478,#17479,#17480,#17481,#17482,
#17483,#17484,#17485,#17486,#17487,#17488,#17489,#17490,#17491,#17492,#17493,
#17494,#17495,#17496,#17497,#17498,#17499,#17500,#17501,#17502,#17503,#17504,
#17505,#17506,#17507,#17508,#17509,#17510,#17511,#17512,#17513,#17514,#17515,
#17516,#17517,#17518,#17519,#17520,#17521,#17522,#17523,#17524,#17525,#17526,
#17527,#17528,#17529,#17530,#17531,#17532,#17533,#17534,#17535,#17536,#17537,
#17538,#17539,#17540,#17541,#17542,#17543,#17544,#17545,#17546,#17547,#17548,
#17549,#17550,#17551,#17552,#17553,#17554,#17555,#17556,#17557,#17558,#17559,
#17560,#17561,#17562,#17563,#17564,#17565,#17566,#17567,#17568,#17569,#17570,
#17571,#17572,#17573,#17574,#17575,#17576,#17577,#17578,#17579,#17580,#17581,
#17582,#17583,#17584,#17585,#17586,#17587,#17588,#17589,#17590,#17591,#17592,
#17593,#17594,#17595,#17596,#17597,#17598,#17599,#17600,#17601,#17602,#17603,
#17604,#17605,#17606,#17607,#17608,#17609,#17610,#17611,#17612,#17613,#17614,
#17615,#17616,#17617,#17618,#17619,#17620,#17621,#17622,#17623,#17624,#17625,
#17626,#17627,#17628,#17629,#17630,#17631,#17632,#17633,#17634,#17635,#17636,
#17637,#17638,#17639,#17640,#17641,#17642,#17643,#17644,#17645,#17646,#17647,
#17648,#17649,#17650,#17651,#17652,#17653,#17654,#17655,#17656,#17657,#17658,
#17659));
#18298=CLOSED_SHELL('',(#17660,#17661,#17662,#17663,#17664,#17665,#17666,
#17667,#17668,#17669));
#18299=CLOSED_SHELL('',(#17670,#17671,#17672,#17673,#17674,#17675,#17676,
#17677));
#18300=CLOSED_SHELL('',(#17678,#17679,#17680,#17681,#17682,#17683,#17684,
#17685,#17686,#17687,#17688,#17689,#17690,#17691,#17692,#17693,#17694,#17695,
#17696,#17697,#17698,#17699,#17700,#17701,#17702,#17703,#17704,#17705,#17706,
#17707,#17708,#17709,#17710,#17711,#17712,#17713,#17714,#17715,#17716,#17717,
#17718,#17719,#17720,#17721,#17722,#17723,#17724,#17725,#17726,#17727,#17728,
#17729,#17730,#17731,#17732,#17733,#17734,#17735,#17736,#17737,#17738,#17739,
#17740,#17741,#17742,#17743,#17744,#17745,#17746,#17747,#17748,#17749,#17750,
#17751,#17752,#17753,#17754,#17755,#17756,#17757,#17758,#17759,#17760,#17761,
#17762,#17763,#17764,#17765,#17766,#17767,#17768,#17769,#17770,#17771,#17772,
#17773,#17774,#17775,#17776,#17777,#17778,#17779,#17780,#17781,#17782,#17783,
#17784,#17785,#17786,#17787,#17788,#17789,#17790,#17791,#17792,#17793,#17794,
#17795,#17796,#17797,#17798,#17799,#17800,#17801,#17802,#17803,#17804,#17805,
#17806,#17807,#17808,#17809,#17810,#17811,#17812,#17813,#17814,#17815,#17816,
#17817,#17818,#17819,#17820,#17821,#17822,#17823,#17824,#17825,#17826,#17827,
#17828,#17829,#17830,#17831,#17832,#17833,#17834,#17835,#17836,#17837,#17838,
#17839,#17840,#17841,#17842,#17843,#17844,#17845,#17846,#17847,#17848,#17849,
#17850,#17851,#17852,#17853,#17854,#17855,#17856,#17857,#17858,#17859,#17860,
#17861,#17862,#17863,#17864,#17865,#17866,#17867,#17868,#17869,#17870,#17871,
#17872,#17873,#17874,#17875,#17876,#17877,#17878,#17879,#17880,#17881));
#18301=CLOSED_SHELL('',(#17882,#17883,#17884,#17885,#17886,#17887,#17888,
#17889,#17890,#17891,#17892,#17893,#17894,#17895,#17896,#17897,#17898,#17899,
#17900,#17901,#17902,#17903,#17904,#17905,#17906,#17907,#17908,#17909,#17910,
#17911,#17912));
#18302=CLOSED_SHELL('',(#17913,#17914,#17915,#17916,#17917,#17918,#17919,
#17920,#17921,#17922));
#18303=CLOSED_SHELL('',(#17923,#17924,#17925,#17926,#17927,#17928,#17929,
#17930,#17931,#17932,#17933,#17934,#17935,#17936,#17937,#17938,#17939,#17940,
#17941,#17942,#17943,#17944,#17945,#17946,#17947,#17948,#17949,#17950,#17951,
#17952,#17953,#17954,#17955,#17956,#17957,#17958,#17959,#17960,#17961,#17962,
#17963,#17964,#17965,#17966,#17967,#17968,#17969,#17970,#17971,#17972,#17973,
#17974,#17975,#17976,#17977,#17978,#17979,#17980,#17981,#17982,#17983,#17984,
#17985,#17986,#17987,#17988,#17989,#17990,#17991,#17992,#17993,#17994,#17995,
#17996,#17997,#17998,#17999,#18000,#18001,#18002,#18003,#18004,#18005,#18006,
#18007,#18008,#18009,#18010,#18011,#18012,#18013,#18014,#18015,#18016,#18017,
#18018));
#18304=CLOSED_SHELL('',(#18019,#18020,#18021,#18022,#18023,#18024,#18025,
#18026,#18027,#18028,#18029,#18030,#18031,#18032,#18033,#18034,#18035,#18036,
#18037,#18038,#18039,#18040,#18041,#18042,#18043,#18044,#18045,#18046,#18047,
#18048,#18049,#18050,#18051,#18052,#18053,#18054,#18055,#18056,#18057,#18058,
#18059,#18060,#18061,#18062,#18063,#18064,#18065,#18066,#18067,#18068,#18069,
#18070,#18071,#18072,#18073,#18074,#18075,#18076,#18077,#18078,#18079,#18080,
#18081,#18082,#18083,#18084,#18085,#18086,#18087,#18088,#18089,#18090,#18091,
#18092,#18093,#18094,#18095,#18096,#18097,#18098,#18099,#18100,#18101,#18102,
#18103,#18104,#18105,#18106,#18107,#18108,#18109,#18110));
#18305=CLOSED_SHELL('',(#18111,#18112,#18113,#18114,#18115,#18116,#18117,
#18118,#18119,#18120,#18121,#18122,#18123,#18124,#18125,#18126,#18127,#18128,
#18129,#18130,#18131,#18132,#18133,#18134,#18135,#18136,#18137,#18138));
#18306=CLOSED_SHELL('',(#18139,#18140,#18141,#18142,#18143,#18144,#18145,
#18146,#18147,#18148,#18149,#18150,#18151,#18152,#18153,#18154,#18155,#18156,
#18157,#18158,#18159,#18160,#18161,#18162,#18163,#18164,#18165,#18166,#18167,
#18168,#18169,#18170,#18171,#18172,#18173,#18174,#18175,#18176,#18177,#18178,
#18179,#18180,#18181,#18182,#18183,#18184,#18185,#18186,#18187,#18188,#18189,
#18190,#18191,#18192,#18193,#18194,#18195,#18196,#18197,#18198,#18199,#18200,
#18201,#18202,#18203,#18204,#18205,#18206,#18207,#18208,#18209,#18210,#18211,
#18212,#18213,#18214,#18215,#18216,#18217,#18218,#18219,#18220,#18221,#18222,
#18223,#18224,#18225,#18226,#18227,#18228,#18229,#18230,#18231,#18232,#18233,
#18234,#18235,#18236,#18237,#18238,#18239,#18240,#18241,#18242,#18243,#18244,
#18245,#18246,#18247,#18248,#18249,#18250,#18251,#18252,#18253,#18254,#18255,
#18256,#18257,#18258,#18259,#18260,#18261,#18262,#18263,#18264,#18265,#18266,
#18267,#18268,#18269,#18270,#18271,#18272,#18273,#18274,#18275,#18276,#18277,
#18278,#18279,#18280,#18281,#18282,#18283,#18284,#18285,#18286,#18287,#18288,
#18289,#18290,#18291,#18292,#18293,#18294,#18295,#18296));
#18307=DERIVED_UNIT_ELEMENT(#18327,1.);
#18308=DERIVED_UNIT_ELEMENT(#60367,-3.);
#18309=DERIVED_UNIT_ELEMENT(#18327,1.);
#18310=DERIVED_UNIT_ELEMENT(#60367,-3.);
#18311=DERIVED_UNIT_ELEMENT(#18327,1.);
#18312=DERIVED_UNIT_ELEMENT(#60367,-3.);
#18313=DERIVED_UNIT_ELEMENT(#18327,1.);
#18314=DERIVED_UNIT_ELEMENT(#60367,-3.);
#18315=DERIVED_UNIT_ELEMENT(#18327,1.);
#18316=DERIVED_UNIT_ELEMENT(#60367,-3.);
#18317=DERIVED_UNIT_ELEMENT(#18327,1.);
#18318=DERIVED_UNIT_ELEMENT(#60367,-3.);
#18319=DERIVED_UNIT_ELEMENT(#18327,1.);
#18320=DERIVED_UNIT_ELEMENT(#60367,-3.);
#18321=DERIVED_UNIT_ELEMENT(#18327,1.);
#18322=DERIVED_UNIT_ELEMENT(#60367,-3.);
#18323=DERIVED_UNIT_ELEMENT(#18327,1.);
#18324=DERIVED_UNIT_ELEMENT(#60367,-3.);
#18325=DERIVED_UNIT_ELEMENT(#18327,1.);
#18326=DERIVED_UNIT_ELEMENT(#60367,-3.);
#18327=(
MASS_UNIT()
NAMED_UNIT(*)
SI_UNIT(.KILO.,.GRAM.)
);
#18328=DERIVED_UNIT((#18307,#18308));
#18329=DERIVED_UNIT((#18309,#18310));
#18330=DERIVED_UNIT((#18311,#18312));
#18331=DERIVED_UNIT((#18313,#18314));
#18332=DERIVED_UNIT((#18315,#18316));
#18333=DERIVED_UNIT((#18317,#18318));
#18334=DERIVED_UNIT((#18319,#18320));
#18335=DERIVED_UNIT((#18321,#18322));
#18336=DERIVED_UNIT((#18323,#18324));
#18337=DERIVED_UNIT((#18325,#18326));
#18338=MEASURE_REPRESENTATION_ITEM('density measure',
POSITIVE_RATIO_MEASURE(7850.),#18328);
#18339=MEASURE_REPRESENTATION_ITEM('density measure',
POSITIVE_RATIO_MEASURE(7850.),#18329);
#18340=MEASURE_REPRESENTATION_ITEM('density measure',
POSITIVE_RATIO_MEASURE(7850.),#18330);
#18341=MEASURE_REPRESENTATION_ITEM('density measure',
POSITIVE_RATIO_MEASURE(7850.),#18331);
#18342=MEASURE_REPRESENTATION_ITEM('density measure',
POSITIVE_RATIO_MEASURE(7850.),#18332);
#18343=MEASURE_REPRESENTATION_ITEM('density measure',
POSITIVE_RATIO_MEASURE(7850.),#18333);
#18344=MEASURE_REPRESENTATION_ITEM('density measure',
POSITIVE_RATIO_MEASURE(7850.),#18334);
#18345=MEASURE_REPRESENTATION_ITEM('density measure',
POSITIVE_RATIO_MEASURE(7850.),#18335);
#18346=MEASURE_REPRESENTATION_ITEM('density measure',
POSITIVE_RATIO_MEASURE(7850.),#18336);
#18347=MEASURE_REPRESENTATION_ITEM('density measure',
POSITIVE_RATIO_MEASURE(7850.),#18337);
#18348=PROPERTY_DEFINITION_REPRESENTATION(#18398,#18368);
#18349=PROPERTY_DEFINITION_REPRESENTATION(#18399,#18369);
#18350=PROPERTY_DEFINITION_REPRESENTATION(#18400,#18370);
#18351=PROPERTY_DEFINITION_REPRESENTATION(#18401,#18371);
#18352=PROPERTY_DEFINITION_REPRESENTATION(#18402,#18372);
#18353=PROPERTY_DEFINITION_REPRESENTATION(#18403,#18373);
#18354=PROPERTY_DEFINITION_REPRESENTATION(#18404,#18374);
#18355=PROPERTY_DEFINITION_REPRESENTATION(#18405,#18375);
#18356=PROPERTY_DEFINITION_REPRESENTATION(#18406,#18376);
#18357=PROPERTY_DEFINITION_REPRESENTATION(#18407,#18377);
#18358=PROPERTY_DEFINITION_REPRESENTATION(#18408,#18378);
#18359=PROPERTY_DEFINITION_REPRESENTATION(#18409,#18379);
#18360=PROPERTY_DEFINITION_REPRESENTATION(#18410,#18380);
#18361=PROPERTY_DEFINITION_REPRESENTATION(#18411,#18381);
#18362=PROPERTY_DEFINITION_REPRESENTATION(#18412,#18382);
#18363=PROPERTY_DEFINITION_REPRESENTATION(#18413,#18383);
#18364=PROPERTY_DEFINITION_REPRESENTATION(#18414,#18384);
#18365=PROPERTY_DEFINITION_REPRESENTATION(#18415,#18385);
#18366=PROPERTY_DEFINITION_REPRESENTATION(#18416,#18386);
#18367=PROPERTY_DEFINITION_REPRESENTATION(#18417,#18387);
#18368=REPRESENTATION('material name',(#18388),#60355);
#18369=REPRESENTATION('density',(#18338),#60355);
#18370=REPRESENTATION('material name',(#18389),#60356);
#18371=REPRESENTATION('density',(#18339),#60356);
#18372=REPRESENTATION('material name',(#18390),#60357);
#18373=REPRESENTATION('density',(#18340),#60357);
#18374=REPRESENTATION('material name',(#18391),#60358);
#18375=REPRESENTATION('density',(#18341),#60358);
#18376=REPRESENTATION('material name',(#18392),#60359);
#18377=REPRESENTATION('density',(#18342),#60359);
#18378=REPRESENTATION('material name',(#18393),#60360);
#18379=REPRESENTATION('density',(#18343),#60360);
#18380=REPRESENTATION('material name',(#18394),#60361);
#18381=REPRESENTATION('density',(#18344),#60361);
#18382=REPRESENTATION('material name',(#18395),#60362);
#18383=REPRESENTATION('density',(#18345),#60362);
#18384=REPRESENTATION('material name',(#18396),#60363);
#18385=REPRESENTATION('density',(#18346),#60363);
#18386=REPRESENTATION('material name',(#18397),#60364);
#18387=REPRESENTATION('density',(#18347),#60364);
#18388=DESCRIPTIVE_REPRESENTATION_ITEM('Steel','Steel');
#18389=DESCRIPTIVE_REPRESENTATION_ITEM('Steel','Steel');
#18390=DESCRIPTIVE_REPRESENTATION_ITEM('Steel','Steel');
#18391=DESCRIPTIVE_REPRESENTATION_ITEM('Steel','Steel');
#18392=DESCRIPTIVE_REPRESENTATION_ITEM('Steel','Steel');
#18393=DESCRIPTIVE_REPRESENTATION_ITEM('Steel','Steel');
#18394=DESCRIPTIVE_REPRESENTATION_ITEM('Steel','Steel');
#18395=DESCRIPTIVE_REPRESENTATION_ITEM('Steel','Steel');
#18396=DESCRIPTIVE_REPRESENTATION_ITEM('Steel','Steel');
#18397=DESCRIPTIVE_REPRESENTATION_ITEM('Steel','Steel');
#18398=PROPERTY_DEFINITION('material property','material name',#60419);
#18399=PROPERTY_DEFINITION('material property','density of part',#60419);
#18400=PROPERTY_DEFINITION('material property','material name',#60420);
#18401=PROPERTY_DEFINITION('material property','density of part',#60420);
#18402=PROPERTY_DEFINITION('material property','material name',#60421);
#18403=PROPERTY_DEFINITION('material property','density of part',#60421);
#18404=PROPERTY_DEFINITION('material property','material name',#60422);
#18405=PROPERTY_DEFINITION('material property','density of part',#60422);
#18406=PROPERTY_DEFINITION('material property','material name',#60423);
#18407=PROPERTY_DEFINITION('material property','density of part',#60423);
#18408=PROPERTY_DEFINITION('material property','material name',#60424);
#18409=PROPERTY_DEFINITION('material property','density of part',#60424);
#18410=PROPERTY_DEFINITION('material property','material name',#60425);
#18411=PROPERTY_DEFINITION('material property','density of part',#60425);
#18412=PROPERTY_DEFINITION('material property','material name',#60426);
#18413=PROPERTY_DEFINITION('material property','density of part',#60426);
#18414=PROPERTY_DEFINITION('material property','material name',#60427);
#18415=PROPERTY_DEFINITION('material property','density of part',#60427);
#18416=PROPERTY_DEFINITION('material property','material name',#60428);
#18417=PROPERTY_DEFINITION('material property','density of part',#60428);
#18418=AXIS2_PLACEMENT_3D('',#23610,#19678,#19679);
#18419=AXIS2_PLACEMENT_3D('',#23611,#19680,#19681);
#18420=AXIS2_PLACEMENT_3D('',#23612,#19682,#19683);
#18421=AXIS2_PLACEMENT_3D('',#23628,#19685,#19686);
#18422=AXIS2_PLACEMENT_3D('',#23636,#19687,#19688);
#18423=AXIS2_PLACEMENT_3D('',#23684,#19690,#19691);
#18424=AXIS2_PLACEMENT_3D('',#23732,#19693,#19694);
#18425=AXIS2_PLACEMENT_3D('',#23786,#19696,#19697);
#18426=AXIS2_PLACEMENT_3D('',#23834,#19699,#19700);
#18427=AXIS2_PLACEMENT_3D('',#23882,#19702,#19703);
#18428=AXIS2_PLACEMENT_3D('',#23936,#19705,#19706);
#18429=AXIS2_PLACEMENT_3D('',#23984,#19708,#19709);
#18430=AXIS2_PLACEMENT_3D('',#24032,#19711,#19712);
#18431=AXIS2_PLACEMENT_3D('',#24086,#19714,#19715);
#18432=AXIS2_PLACEMENT_3D('',#24134,#19717,#19718);
#18433=AXIS2_PLACEMENT_3D('',#24182,#19720,#19721);
#18434=AXIS2_PLACEMENT_3D('',#24236,#19723,#19724);
#18435=AXIS2_PLACEMENT_3D('',#24284,#19726,#19727);
#18436=AXIS2_PLACEMENT_3D('',#24332,#19729,#19730);
#18437=AXIS2_PLACEMENT_3D('',#24702,#19732,#19733);
#18438=AXIS2_PLACEMENT_3D('',#24772,#19734,#19735);
#18439=AXIS2_PLACEMENT_3D('',#24791,#19736,#19737);
#18440=AXIS2_PLACEMENT_3D('',#24942,#19738,#19739);
#18441=AXIS2_PLACEMENT_3D('',#24959,#19740,#19741);
#18442=AXIS2_PLACEMENT_3D('',#25110,#19742,#19743);
#18443=AXIS2_PLACEMENT_3D('',#25129,#19744,#19745);
#18444=AXIS2_PLACEMENT_3D('',#25280,#19746,#19747);
#18445=AXIS2_PLACEMENT_3D('',#25299,#19748,#19749);
#18446=AXIS2_PLACEMENT_3D('',#25450,#19750,#19751);
#18447=AXIS2_PLACEMENT_3D('',#25467,#19752,#19753);
#18448=AXIS2_PLACEMENT_3D('',#25618,#19754,#19755);
#18449=AXIS2_PLACEMENT_3D('',#25637,#19756,#19757);
#18450=AXIS2_PLACEMENT_3D('',#25788,#19758,#19759);
#18451=AXIS2_PLACEMENT_3D('',#25807,#19760,#19761);
#18452=AXIS2_PLACEMENT_3D('',#25958,#19762,#19763);
#18453=AXIS2_PLACEMENT_3D('',#25975,#19764,#19765);
#18454=AXIS2_PLACEMENT_3D('',#26126,#19766,#19767);
#18455=AXIS2_PLACEMENT_3D('',#26145,#19768,#19769);
#18456=AXIS2_PLACEMENT_3D('',#26296,#19770,#19771);
#18457=AXIS2_PLACEMENT_3D('',#26315,#19772,#19773);
#18458=AXIS2_PLACEMENT_3D('',#26466,#19774,#19775);
#18459=AXIS2_PLACEMENT_3D('',#26483,#19776,#19777);
#18460=AXIS2_PLACEMENT_3D('',#26590,#19778,#19779);
#18461=AXIS2_PLACEMENT_3D('',#26602,#19781,#19782);
#18462=AXIS2_PLACEMENT_3D('',#26608,#19783,#19784);
#18463=AXIS2_PLACEMENT_3D('',#26633,#19786,#19787);
#18464=AXIS2_PLACEMENT_3D('',#26658,#19789,#19790);
#18465=AXIS2_PLACEMENT_3D('',#26682,#19792,#19793);
#18466=AXIS2_PLACEMENT_3D('',#26707,#19795,#19796);
#18467=AXIS2_PLACEMENT_3D('',#26732,#19798,#19799);
#18468=AXIS2_PLACEMENT_3D('',#26756,#19801,#19802);
#18469=AXIS2_PLACEMENT_3D('',#26781,#19804,#19805);
#18470=AXIS2_PLACEMENT_3D('',#26806,#19807,#19808);
#18471=AXIS2_PLACEMENT_3D('',#26830,#19810,#19811);
#18472=AXIS2_PLACEMENT_3D('',#26855,#19813,#19814);
#18473=AXIS2_PLACEMENT_3D('',#26880,#19816,#19817);
#18474=AXIS2_PLACEMENT_3D('',#26904,#19819,#19820);
#18475=AXIS2_PLACEMENT_3D('',#26929,#19822,#19823);
#18476=AXIS2_PLACEMENT_3D('',#26954,#19825,#19826);
#18477=AXIS2_PLACEMENT_3D('',#26978,#19828,#19829);
#18478=AXIS2_PLACEMENT_3D('',#26980,#19830,#19831);
#18479=AXIS2_PLACEMENT_3D('',#26984,#19833,#19834);
#18480=AXIS2_PLACEMENT_3D('',#26985,#19835,#19836);
#18481=AXIS2_PLACEMENT_3D('',#26986,#19837,#19838);
#18482=AXIS2_PLACEMENT_3D('',#26989,#19840,#19841);
#18483=AXIS2_PLACEMENT_3D('',#26990,#19842,#19843);
#18484=AXIS2_PLACEMENT_3D('',#26992,#19844,#19845);
#18485=AXIS2_PLACEMENT_3D('',#26993,#19846,#19847);
#18486=AXIS2_PLACEMENT_3D('',#27004,#19853,#19854);
#18487=AXIS2_PLACEMENT_3D('',#27010,#19858,#19859);
#18488=AXIS2_PLACEMENT_3D('',#27016,#19863,#19864);
#18489=AXIS2_PLACEMENT_3D('',#27022,#19868,#19869);
#18490=AXIS2_PLACEMENT_3D('',#27033,#19875,#19876);
#18491=AXIS2_PLACEMENT_3D('',#27039,#19880,#19881);
#18492=AXIS2_PLACEMENT_3D('',#27045,#19885,#19886);
#18493=AXIS2_PLACEMENT_3D('',#27048,#19889,#19890);
#18494=AXIS2_PLACEMENT_3D('',#27059,#19896,#19897);
#18495=AXIS2_PLACEMENT_3D('',#27065,#19901,#19902);
#18496=AXIS2_PLACEMENT_3D('',#27071,#19906,#19907);
#18497=AXIS2_PLACEMENT_3D('',#27074,#19910,#19911);
#18498=AXIS2_PLACEMENT_3D('',#27085,#19917,#19918);
#18499=AXIS2_PLACEMENT_3D('',#27091,#19922,#19923);
#18500=AXIS2_PLACEMENT_3D('',#27097,#19927,#19928);
#18501=AXIS2_PLACEMENT_3D('',#27100,#19931,#19932);
#18502=AXIS2_PLACEMENT_3D('',#27111,#19938,#19939);
#18503=AXIS2_PLACEMENT_3D('',#27117,#19943,#19944);
#18504=AXIS2_PLACEMENT_3D('',#27123,#19948,#19949);
#18505=AXIS2_PLACEMENT_3D('',#27126,#19952,#19953);
#18506=AXIS2_PLACEMENT_3D('',#27137,#19959,#19960);
#18507=AXIS2_PLACEMENT_3D('',#27142,#19964,#19965);
#18508=AXIS2_PLACEMENT_3D('',#27146,#19968,#19969);
#18509=AXIS2_PLACEMENT_3D('',#27152,#19973,#19974);
#18510=AXIS2_PLACEMENT_3D('',#27163,#19980,#19981);
#18511=AXIS2_PLACEMENT_3D('',#27168,#19985,#19986);
#18512=AXIS2_PLACEMENT_3D('',#27172,#19989,#19990);
#18513=AXIS2_PLACEMENT_3D('',#27183,#19996,#19997);
#18514=AXIS2_PLACEMENT_3D('',#27189,#20001,#20002);
#18515=AXIS2_PLACEMENT_3D('',#27195,#20006,#20007);
#18516=AXIS2_PLACEMENT_3D('',#27201,#20011,#20012);
#18517=AXIS2_PLACEMENT_3D('',#27212,#20018,#20019);
#18518=AXIS2_PLACEMENT_3D('',#27217,#20023,#20024);
#18519=AXIS2_PLACEMENT_3D('',#27221,#20027,#20028);
#18520=AXIS2_PLACEMENT_3D('',#27227,#20032,#20033);
#18521=AXIS2_PLACEMENT_3D('',#27238,#20039,#20040);
#18522=AXIS2_PLACEMENT_3D('',#27243,#20044,#20045);
#18523=AXIS2_PLACEMENT_3D('',#27247,#20048,#20049);
#18524=AXIS2_PLACEMENT_3D('',#27253,#20053,#20054);
#18525=AXIS2_PLACEMENT_3D('',#27264,#20060,#20061);
#18526=AXIS2_PLACEMENT_3D('',#27269,#20065,#20066);
#18527=AXIS2_PLACEMENT_3D('',#27273,#20069,#20070);
#18528=AXIS2_PLACEMENT_3D('',#27279,#20074,#20075);
#18529=AXIS2_PLACEMENT_3D('',#27290,#20081,#20082);
#18530=AXIS2_PLACEMENT_3D('',#27295,#20086,#20087);
#18531=AXIS2_PLACEMENT_3D('',#27299,#20090,#20091);
#18532=AXIS2_PLACEMENT_3D('',#27302,#20094,#20095);
#18533=AXIS2_PLACEMENT_3D('',#27310,#20096,#20097);
#18534=AXIS2_PLACEMENT_3D('',#27316,#20098,#20099);
#18535=AXIS2_PLACEMENT_3D('',#27317,#20100,#20101);
#18536=AXIS2_PLACEMENT_3D('',#27417,#20102,#20103);
#18537=AXIS2_PLACEMENT_3D('',#27811,#20104,#20105);
#18538=AXIS2_PLACEMENT_3D('',#27819,#20106,#20107);
#18539=AXIS2_PLACEMENT_3D('',#27825,#20108,#20109);
#18540=AXIS2_PLACEMENT_3D('',#27826,#20110,#20111);
#18541=AXIS2_PLACEMENT_3D('',#27920,#20112,#20113);
#18542=AXIS2_PLACEMENT_3D('',#28247,#20114,#20115);
#18543=AXIS2_PLACEMENT_3D('',#28255,#20116,#20117);
#18544=AXIS2_PLACEMENT_3D('',#28261,#20118,#20119);
#18545=AXIS2_PLACEMENT_3D('',#28262,#20120,#20121);
#18546=AXIS2_PLACEMENT_3D('',#28362,#20122,#20123);
#18547=AXIS2_PLACEMENT_3D('',#28719,#20124,#20125);
#18548=AXIS2_PLACEMENT_3D('',#28727,#20126,#20127);
#18549=AXIS2_PLACEMENT_3D('',#28733,#20128,#20129);
#18550=AXIS2_PLACEMENT_3D('',#28734,#20130,#20131);
#18551=AXIS2_PLACEMENT_3D('',#28834,#20132,#20133);
#18552=AXIS2_PLACEMENT_3D('',#29181,#20134,#20135);
#18553=AXIS2_PLACEMENT_3D('',#29189,#20136,#20137);
#18554=AXIS2_PLACEMENT_3D('',#29195,#20138,#20139);
#18555=AXIS2_PLACEMENT_3D('',#29196,#20140,#20141);
#18556=AXIS2_PLACEMENT_3D('',#29290,#20142,#20143);
#18557=AXIS2_PLACEMENT_3D('',#29617,#20144,#20145);
#18558=AXIS2_PLACEMENT_3D('',#29625,#20146,#20147);
#18559=AXIS2_PLACEMENT_3D('',#29631,#20148,#20149);
#18560=AXIS2_PLACEMENT_3D('',#29632,#20150,#20151);
#18561=AXIS2_PLACEMENT_3D('',#29732,#20152,#20153);
#18562=AXIS2_PLACEMENT_3D('',#30089,#20154,#20155);
#18563=AXIS2_PLACEMENT_3D('',#30097,#20156,#20157);
#18564=AXIS2_PLACEMENT_3D('',#30103,#20158,#20159);
#18565=AXIS2_PLACEMENT_3D('',#30104,#20160,#20161);
#18566=AXIS2_PLACEMENT_3D('',#30204,#20162,#20163);
#18567=AXIS2_PLACEMENT_3D('',#30551,#20164,#20165);
#18568=AXIS2_PLACEMENT_3D('',#30559,#20166,#20167);
#18569=AXIS2_PLACEMENT_3D('',#30565,#20168,#20169);
#18570=AXIS2_PLACEMENT_3D('',#30566,#20170,#20171);
#18571=AXIS2_PLACEMENT_3D('',#30660,#20172,#20173);
#18572=AXIS2_PLACEMENT_3D('',#30987,#20174,#20175);
#18573=AXIS2_PLACEMENT_3D('',#30995,#20176,#20177);
#18574=AXIS2_PLACEMENT_3D('',#31001,#20178,#20179);
#18575=AXIS2_PLACEMENT_3D('',#31002,#20180,#20181);
#18576=AXIS2_PLACEMENT_3D('',#31102,#20182,#20183);
#18577=AXIS2_PLACEMENT_3D('',#31459,#20184,#20185);
#18578=AXIS2_PLACEMENT_3D('',#31467,#20186,#20187);
#18579=AXIS2_PLACEMENT_3D('',#31473,#20188,#20189);
#18580=AXIS2_PLACEMENT_3D('',#31474,#20190,#20191);
#18581=AXIS2_PLACEMENT_3D('',#31574,#20192,#20193);
#18582=AXIS2_PLACEMENT_3D('',#31921,#20194,#20195);
#18583=AXIS2_PLACEMENT_3D('',#31929,#20196,#20197);
#18584=AXIS2_PLACEMENT_3D('',#31935,#20198,#20199);
#18585=AXIS2_PLACEMENT_3D('',#31936,#20200,#20201);
#18586=AXIS2_PLACEMENT_3D('',#32030,#20202,#20203);
#18587=AXIS2_PLACEMENT_3D('',#32357,#20204,#20205);
#18588=AXIS2_PLACEMENT_3D('',#32365,#20206,#20207);
#18589=AXIS2_PLACEMENT_3D('',#32371,#20208,#20209);
#18590=AXIS2_PLACEMENT_3D('',#32372,#20210,#20211);
#18591=AXIS2_PLACEMENT_3D('',#32472,#20212,#20213);
#18592=AXIS2_PLACEMENT_3D('',#32829,#20214,#20215);
#18593=AXIS2_PLACEMENT_3D('',#32831,#20216,#20217);
#18594=AXIS2_PLACEMENT_3D('',#32834,#20219,#20220);
#18595=AXIS2_PLACEMENT_3D('',#32835,#20221,#20222);
#18596=AXIS2_PLACEMENT_3D('',#32837,#20223,#20224);
#18597=AXIS2_PLACEMENT_3D('',#32838,#20225,#20226);
#18598=AXIS2_PLACEMENT_3D('',#32840,#20227,#20228);
#18599=AXIS2_PLACEMENT_3D('',#32842,#20230,#20231);
#18600=AXIS2_PLACEMENT_3D('',#32844,#20232,#20233);
#18601=AXIS2_PLACEMENT_3D('',#32847,#20235,#20236);
#18602=AXIS2_PLACEMENT_3D('',#32848,#20237,#20238);
#18603=AXIS2_PLACEMENT_3D('',#32850,#20239,#20240);
#18604=AXIS2_PLACEMENT_3D('',#32851,#20241,#20242);
#18605=AXIS2_PLACEMENT_3D('',#32854,#20244,#20245);
#18606=AXIS2_PLACEMENT_3D('',#32855,#20246,#20247);
#18607=AXIS2_PLACEMENT_3D('',#32872,#20250,#20251);
#18608=AXIS2_PLACEMENT_3D('',#32879,#20252,#20253);
#18609=AXIS2_PLACEMENT_3D('',#32889,#20254,#20255);
#18610=AXIS2_PLACEMENT_3D('',#32890,#20256,#20257);
#18611=AXIS2_PLACEMENT_3D('',#32892,#20258,#20259);
#18612=AXIS2_PLACEMENT_3D('',#32902,#20260,#20261);
#18613=AXIS2_PLACEMENT_3D('',#32903,#20262,#20263);
#18614=AXIS2_PLACEMENT_3D('',#32904,#20264,#20265);
#18615=AXIS2_PLACEMENT_3D('',#32906,#20266,#20267);
#18616=AXIS2_PLACEMENT_3D('',#32913,#20268,#20269);
#18617=AXIS2_PLACEMENT_3D('',#32915,#20271,#20272);
#18618=AXIS2_PLACEMENT_3D('',#32925,#20274,#20275);
#18619=AXIS2_PLACEMENT_3D('',#32927,#20276,#20277);
#18620=AXIS2_PLACEMENT_3D('',#32937,#20278,#20279);
#18621=AXIS2_PLACEMENT_3D('',#32938,#20280,#20281);
#18622=AXIS2_PLACEMENT_3D('',#32950,#20284,#20285);
#18623=AXIS2_PLACEMENT_3D('',#32952,#20286,#20287);
#18624=AXIS2_PLACEMENT_3D('',#32962,#20288,#20289);
#18625=AXIS2_PLACEMENT_3D('',#32963,#20290,#20291);
#18626=AXIS2_PLACEMENT_3D('',#32964,#20292,#20293);
#18627=AXIS2_PLACEMENT_3D('',#32966,#20294,#20295);
#18628=AXIS2_PLACEMENT_3D('',#32973,#20296,#20297);
#18629=AXIS2_PLACEMENT_3D('',#32975,#20299,#20300);
#18630=AXIS2_PLACEMENT_3D('',#32985,#20302,#20303);
#18631=AXIS2_PLACEMENT_3D('',#32987,#20304,#20305);
#18632=AXIS2_PLACEMENT_3D('',#32997,#20306,#20307);
#18633=AXIS2_PLACEMENT_3D('',#32998,#20308,#20309);
#18634=AXIS2_PLACEMENT_3D('',#33010,#20312,#20313);
#18635=AXIS2_PLACEMENT_3D('',#33012,#20314,#20315);
#18636=AXIS2_PLACEMENT_3D('',#33022,#20316,#20317);
#18637=AXIS2_PLACEMENT_3D('',#33023,#20318,#20319);
#18638=AXIS2_PLACEMENT_3D('',#33024,#20320,#20321);
#18639=AXIS2_PLACEMENT_3D('',#33026,#20322,#20323);
#18640=AXIS2_PLACEMENT_3D('',#33033,#20324,#20325);
#18641=AXIS2_PLACEMENT_3D('',#33035,#20327,#20328);
#18642=AXIS2_PLACEMENT_3D('',#33045,#20330,#20331);
#18643=AXIS2_PLACEMENT_3D('',#33047,#20332,#20333);
#18644=AXIS2_PLACEMENT_3D('',#33057,#20334,#20335);
#18645=AXIS2_PLACEMENT_3D('',#33058,#20336,#20337);
#18646=AXIS2_PLACEMENT_3D('',#33070,#20340,#20341);
#18647=AXIS2_PLACEMENT_3D('',#33072,#20342,#20343);
#18648=AXIS2_PLACEMENT_3D('',#33082,#20344,#20345);
#18649=AXIS2_PLACEMENT_3D('',#33083,#20346,#20347);
#18650=AXIS2_PLACEMENT_3D('',#33084,#20348,#20349);
#18651=AXIS2_PLACEMENT_3D('',#33086,#20350,#20351);
#18652=AXIS2_PLACEMENT_3D('',#33093,#20352,#20353);
#18653=AXIS2_PLACEMENT_3D('',#33095,#20355,#20356);
#18654=AXIS2_PLACEMENT_3D('',#33105,#20358,#20359);
#18655=AXIS2_PLACEMENT_3D('',#33107,#20360,#20361);
#18656=AXIS2_PLACEMENT_3D('',#33117,#20362,#20363);
#18657=AXIS2_PLACEMENT_3D('',#33118,#20364,#20365);
#18658=AXIS2_PLACEMENT_3D('',#33130,#20368,#20369);
#18659=AXIS2_PLACEMENT_3D('',#33132,#20370,#20371);
#18660=AXIS2_PLACEMENT_3D('',#33142,#20372,#20373);
#18661=AXIS2_PLACEMENT_3D('',#33143,#20374,#20375);
#18662=AXIS2_PLACEMENT_3D('',#33144,#20376,#20377);
#18663=AXIS2_PLACEMENT_3D('',#33146,#20378,#20379);
#18664=AXIS2_PLACEMENT_3D('',#33153,#20380,#20381);
#18665=AXIS2_PLACEMENT_3D('',#33155,#20383,#20384);
#18666=AXIS2_PLACEMENT_3D('',#33165,#20386,#20387);
#18667=AXIS2_PLACEMENT_3D('',#33167,#20388,#20389);
#18668=AXIS2_PLACEMENT_3D('',#33177,#20390,#20391);
#18669=AXIS2_PLACEMENT_3D('',#33178,#20392,#20393);
#18670=AXIS2_PLACEMENT_3D('',#33180,#20394,#20395);
#18671=AXIS2_PLACEMENT_3D('',#33182,#20396,#20397);
#18672=AXIS2_PLACEMENT_3D('',#33184,#20398,#20399);
#18673=AXIS2_PLACEMENT_3D('',#33186,#20400,#20401);
#18674=AXIS2_PLACEMENT_3D('',#33188,#20402,#20403);
#18675=AXIS2_PLACEMENT_3D('',#33190,#20404,#20405);
#18676=AXIS2_PLACEMENT_3D('',#33192,#20406,#20407);
#18677=AXIS2_PLACEMENT_3D('',#33194,#20408,#20409);
#18678=AXIS2_PLACEMENT_3D('',#33196,#20410,#20411);
#18679=AXIS2_PLACEMENT_3D('',#33198,#20412,#20413);
#18680=AXIS2_PLACEMENT_3D('',#33200,#20414,#20415);
#18681=AXIS2_PLACEMENT_3D('',#33202,#20416,#20417);
#18682=AXIS2_PLACEMENT_3D('',#33203,#20418,#20419);
#18683=AXIS2_PLACEMENT_3D('',#33205,#20420,#20421);
#18684=AXIS2_PLACEMENT_3D('',#33206,#20422,#20423);
#18685=AXIS2_PLACEMENT_3D('',#33212,#20424,#20425);
#18686=AXIS2_PLACEMENT_3D('',#33221,#20426,#20427);
#18687=AXIS2_PLACEMENT_3D('',#33229,#20430,#20431);
#18688=AXIS2_PLACEMENT_3D('',#33236,#20432,#20433);
#18689=AXIS2_PLACEMENT_3D('',#33243,#20434,#20435);
#18690=AXIS2_PLACEMENT_3D('',#33252,#20437,#20438);
#18691=AXIS2_PLACEMENT_3D('',#33259,#20439,#20440);
#18692=AXIS2_PLACEMENT_3D('',#33269,#20442,#20443);
#18693=AXIS2_PLACEMENT_3D('',#33270,#20444,#20445);
#18694=AXIS2_PLACEMENT_3D('',#33272,#20446,#20447);
#18695=AXIS2_PLACEMENT_3D('',#33279,#20448,#20449);
#18696=AXIS2_PLACEMENT_3D('',#33281,#20451,#20452);
#18697=AXIS2_PLACEMENT_3D('',#33291,#20454,#20455);
#18698=AXIS2_PLACEMENT_3D('',#33293,#20456,#20457);
#18699=AXIS2_PLACEMENT_3D('',#33302,#20458,#20459);
#18700=AXIS2_PLACEMENT_3D('',#33308,#20460,#20461);
#18701=AXIS2_PLACEMENT_3D('',#33317,#20462,#20463);
#18702=AXIS2_PLACEMENT_3D('',#33325,#20466,#20467);
#18703=AXIS2_PLACEMENT_3D('',#33326,#20468,#20469);
#18704=AXIS2_PLACEMENT_3D('',#33328,#20470,#20471);
#18705=AXIS2_PLACEMENT_3D('',#33335,#20472,#20473);
#18706=AXIS2_PLACEMENT_3D('',#33337,#20475,#20476);
#18707=AXIS2_PLACEMENT_3D('',#33347,#20478,#20479);
#18708=AXIS2_PLACEMENT_3D('',#33349,#20480,#20481);
#18709=AXIS2_PLACEMENT_3D('',#33358,#20482,#20483);
#18710=AXIS2_PLACEMENT_3D('',#33364,#20484,#20485);
#18711=AXIS2_PLACEMENT_3D('',#33373,#20486,#20487);
#18712=AXIS2_PLACEMENT_3D('',#33381,#20490,#20491);
#18713=AXIS2_PLACEMENT_3D('',#33382,#20492,#20493);
#18714=AXIS2_PLACEMENT_3D('',#33384,#20494,#20495);
#18715=AXIS2_PLACEMENT_3D('',#33391,#20496,#20497);
#18716=AXIS2_PLACEMENT_3D('',#33393,#20499,#20500);
#18717=AXIS2_PLACEMENT_3D('',#33403,#20502,#20503);
#18718=AXIS2_PLACEMENT_3D('',#33405,#20504,#20505);
#18719=AXIS2_PLACEMENT_3D('',#33414,#20506,#20507);
#18720=AXIS2_PLACEMENT_3D('',#33420,#20508,#20509);
#18721=AXIS2_PLACEMENT_3D('',#33429,#20510,#20511);
#18722=AXIS2_PLACEMENT_3D('',#33437,#20514,#20515);
#18723=AXIS2_PLACEMENT_3D('',#33438,#20516,#20517);
#18724=AXIS2_PLACEMENT_3D('',#33440,#20518,#20519);
#18725=AXIS2_PLACEMENT_3D('',#33447,#20520,#20521);
#18726=AXIS2_PLACEMENT_3D('',#33449,#20523,#20524);
#18727=AXIS2_PLACEMENT_3D('',#33459,#20526,#20527);
#18728=AXIS2_PLACEMENT_3D('',#33461,#20528,#20529);
#18729=AXIS2_PLACEMENT_3D('',#33470,#20530,#20531);
#18730=AXIS2_PLACEMENT_3D('',#33476,#20532,#20533);
#18731=AXIS2_PLACEMENT_3D('',#33485,#20534,#20535);
#18732=AXIS2_PLACEMENT_3D('',#33493,#20538,#20539);
#18733=AXIS2_PLACEMENT_3D('',#33494,#20540,#20541);
#18734=AXIS2_PLACEMENT_3D('',#33496,#20542,#20543);
#18735=AXIS2_PLACEMENT_3D('',#33503,#20544,#20545);
#18736=AXIS2_PLACEMENT_3D('',#33505,#20547,#20548);
#18737=AXIS2_PLACEMENT_3D('',#33515,#20550,#20551);
#18738=AXIS2_PLACEMENT_3D('',#33517,#20552,#20553);
#18739=AXIS2_PLACEMENT_3D('',#33526,#20554,#20555);
#18740=AXIS2_PLACEMENT_3D('',#33532,#20556,#20557);
#18741=AXIS2_PLACEMENT_3D('',#33541,#20558,#20559);
#18742=AXIS2_PLACEMENT_3D('',#33549,#20562,#20563);
#18743=AXIS2_PLACEMENT_3D('',#33551,#20564,#20565);
#18744=AXIS2_PLACEMENT_3D('',#33554,#20567,#20568);
#18745=AXIS2_PLACEMENT_3D('',#33556,#20569,#20570);
#18746=AXIS2_PLACEMENT_3D('',#33562,#20571,#20572);
#18747=AXIS2_PLACEMENT_3D('',#33563,#20573,#20574);
#18748=AXIS2_PLACEMENT_3D('',#33572,#20575,#20576);
#18749=AXIS2_PLACEMENT_3D('',#33573,#20577,#20578);
#18750=AXIS2_PLACEMENT_3D('',#33575,#20579,#20580);
#18751=AXIS2_PLACEMENT_3D('',#33582,#20581,#20582);
#18752=AXIS2_PLACEMENT_3D('',#33584,#20584,#20585);
#18753=AXIS2_PLACEMENT_3D('',#33594,#20587,#20588);
#18754=AXIS2_PLACEMENT_3D('',#33596,#20589,#20590);
#18755=AXIS2_PLACEMENT_3D('',#33600,#20591,#20592);
#18756=AXIS2_PLACEMENT_3D('',#33606,#20594,#20595);
#18757=AXIS2_PLACEMENT_3D('',#33614,#20596,#20597);
#18758=AXIS2_PLACEMENT_3D('',#33615,#20598,#20599);
#18759=AXIS2_PLACEMENT_3D('',#33629,#20600,#20601);
#18760=AXIS2_PLACEMENT_3D('',#33634,#20602,#20603);
#18761=AXIS2_PLACEMENT_3D('',#33731,#20604,#20605);
#18762=AXIS2_PLACEMENT_3D('',#33733,#20606,#20607);
#18763=AXIS2_PLACEMENT_3D('',#34382,#20608,#20609);
#18764=AXIS2_PLACEMENT_3D('',#34384,#20610,#20611);
#18765=AXIS2_PLACEMENT_3D('',#34385,#20612,#20613);
#18766=AXIS2_PLACEMENT_3D('',#34484,#20614,#20615);
#18767=AXIS2_PLACEMENT_3D('',#34485,#20616,#20617);
#18768=AXIS2_PLACEMENT_3D('',#34938,#20618,#20619);
#18769=AXIS2_PLACEMENT_3D('',#35216,#20620,#20621);
#18770=AXIS2_PLACEMENT_3D('',#35281,#20622,#20623);
#18771=AXIS2_PLACEMENT_3D('',#35286,#20624,#20625);
#18772=AXIS2_PLACEMENT_3D('',#35287,#20626,#20627);
#18773=AXIS2_PLACEMENT_3D('',#35288,#20628,#20629);
#18774=AXIS2_PLACEMENT_3D('',#35301,#20630,#20631);
#18775=AXIS2_PLACEMENT_3D('',#35306,#20632,#20633);
#18776=AXIS2_PLACEMENT_3D('',#35307,#20634,#20635);
#18777=AXIS2_PLACEMENT_3D('',#35308,#20636,#20637);
#18778=AXIS2_PLACEMENT_3D('',#35309,#20638,#20639);
#18779=AXIS2_PLACEMENT_3D('',#35322,#20640,#20641);
#18780=AXIS2_PLACEMENT_3D('',#35327,#20642,#20643);
#18781=AXIS2_PLACEMENT_3D('',#35328,#20644,#20645);
#18782=AXIS2_PLACEMENT_3D('',#35329,#20646,#20647);
#18783=AXIS2_PLACEMENT_3D('',#35330,#20648,#20649);
#18784=AXIS2_PLACEMENT_3D('',#35343,#20650,#20651);
#18785=AXIS2_PLACEMENT_3D('',#35348,#20652,#20653);
#18786=AXIS2_PLACEMENT_3D('',#35349,#20654,#20655);
#18787=AXIS2_PLACEMENT_3D('',#35350,#20656,#20657);
#18788=AXIS2_PLACEMENT_3D('',#35351,#20658,#20659);
#18789=AXIS2_PLACEMENT_3D('',#35364,#20660,#20661);
#18790=AXIS2_PLACEMENT_3D('',#35369,#20662,#20663);
#18791=AXIS2_PLACEMENT_3D('',#35370,#20664,#20665);
#18792=AXIS2_PLACEMENT_3D('',#35371,#20666,#20667);
#18793=AXIS2_PLACEMENT_3D('',#35372,#20668,#20669);
#18794=AXIS2_PLACEMENT_3D('',#35385,#20670,#20671);
#18795=AXIS2_PLACEMENT_3D('',#35390,#20672,#20673);
#18796=AXIS2_PLACEMENT_3D('',#35391,#20674,#20675);
#18797=AXIS2_PLACEMENT_3D('',#35392,#20676,#20677);
#18798=AXIS2_PLACEMENT_3D('',#35393,#20678,#20679);
#18799=AXIS2_PLACEMENT_3D('',#35406,#20680,#20681);
#18800=AXIS2_PLACEMENT_3D('',#35411,#20682,#20683);
#18801=AXIS2_PLACEMENT_3D('',#35412,#20684,#20685);
#18802=AXIS2_PLACEMENT_3D('',#35413,#20686,#20687);
#18803=AXIS2_PLACEMENT_3D('',#35414,#20688,#20689);
#18804=AXIS2_PLACEMENT_3D('',#35427,#20690,#20691);
#18805=AXIS2_PLACEMENT_3D('',#35432,#20692,#20693);
#18806=AXIS2_PLACEMENT_3D('',#35433,#20694,#20695);
#18807=AXIS2_PLACEMENT_3D('',#35434,#20696,#20697);
#18808=AXIS2_PLACEMENT_3D('',#35435,#20698,#20699);
#18809=AXIS2_PLACEMENT_3D('',#35448,#20700,#20701);
#18810=AXIS2_PLACEMENT_3D('',#35453,#20702,#20703);
#18811=AXIS2_PLACEMENT_3D('',#35454,#20704,#20705);
#18812=AXIS2_PLACEMENT_3D('',#35455,#20706,#20707);
#18813=AXIS2_PLACEMENT_3D('',#35456,#20708,#20709);
#18814=AXIS2_PLACEMENT_3D('',#35469,#20710,#20711);
#18815=AXIS2_PLACEMENT_3D('',#35474,#20712,#20713);
#18816=AXIS2_PLACEMENT_3D('',#35475,#20714,#20715);
#18817=AXIS2_PLACEMENT_3D('',#35476,#20716,#20717);
#18818=AXIS2_PLACEMENT_3D('',#35481,#20718,#20719);
#18819=AXIS2_PLACEMENT_3D('',#35482,#20720,#20721);
#18820=AXIS2_PLACEMENT_3D('',#35483,#20722,#20723);
#18821=AXIS2_PLACEMENT_3D('',#35488,#20724,#20725);
#18822=AXIS2_PLACEMENT_3D('',#35489,#20726,#20727);
#18823=AXIS2_PLACEMENT_3D('',#35491,#20728,#20729);
#18824=AXIS2_PLACEMENT_3D('',#35494,#20731,#20732);
#18825=AXIS2_PLACEMENT_3D('',#35495,#20733,#20734);
#18826=AXIS2_PLACEMENT_3D('',#35496,#20735,#20736);
#18827=AXIS2_PLACEMENT_3D('',#35498,#20737,#20738);
#18828=AXIS2_PLACEMENT_3D('',#35499,#20739,#20740);
#18829=AXIS2_PLACEMENT_3D('',#35501,#20741,#20742);
#18830=AXIS2_PLACEMENT_3D('',#35503,#20744,#20745);
#18831=AXIS2_PLACEMENT_3D('',#35505,#20747,#20748);
#18832=AXIS2_PLACEMENT_3D('',#35513,#20749,#20750);
#18833=AXIS2_PLACEMENT_3D('',#35514,#20751,#20752);
#18834=AXIS2_PLACEMENT_3D('',#36014,#20753,#20754);
#18835=AXIS2_PLACEMENT_3D('',#36022,#20755,#20756);
#18836=AXIS2_PLACEMENT_3D('',#36023,#20757,#20758);
#18837=AXIS2_PLACEMENT_3D('',#36533,#20759,#20760);
#18838=AXIS2_PLACEMENT_3D('',#36541,#20761,#20762);
#18839=AXIS2_PLACEMENT_3D('',#36542,#20763,#20764);
#18840=AXIS2_PLACEMENT_3D('',#37032,#20765,#20766);
#18841=AXIS2_PLACEMENT_3D('',#37040,#20767,#20768);
#18842=AXIS2_PLACEMENT_3D('',#37041,#20769,#20770);
#18843=AXIS2_PLACEMENT_3D('',#37541,#20771,#20772);
#18844=AXIS2_PLACEMENT_3D('',#37549,#20773,#20774);
#18845=AXIS2_PLACEMENT_3D('',#37550,#20775,#20776);
#18846=AXIS2_PLACEMENT_3D('',#38060,#20777,#20778);
#18847=AXIS2_PLACEMENT_3D('',#38068,#20779,#20780);
#18848=AXIS2_PLACEMENT_3D('',#38069,#20781,#20782);
#18849=AXIS2_PLACEMENT_3D('',#38559,#20783,#20784);
#18850=AXIS2_PLACEMENT_3D('',#38567,#20785,#20786);
#18851=AXIS2_PLACEMENT_3D('',#38568,#20787,#20788);
#18852=AXIS2_PLACEMENT_3D('',#39068,#20789,#20790);
#18853=AXIS2_PLACEMENT_3D('',#39076,#20791,#20792);
#18854=AXIS2_PLACEMENT_3D('',#39077,#20793,#20794);
#18855=AXIS2_PLACEMENT_3D('',#39587,#20795,#20796);
#18856=AXIS2_PLACEMENT_3D('',#39595,#20797,#20798);
#18857=AXIS2_PLACEMENT_3D('',#39596,#20799,#20800);
#18858=AXIS2_PLACEMENT_3D('',#40096,#20801,#20802);
#18859=AXIS2_PLACEMENT_3D('',#40104,#20803,#20804);
#18860=AXIS2_PLACEMENT_3D('',#40105,#20805,#20806);
#18861=AXIS2_PLACEMENT_3D('',#40605,#20807,#20808);
#18862=AXIS2_PLACEMENT_3D('',#40613,#20809,#20810);
#18863=AXIS2_PLACEMENT_3D('',#40614,#20811,#20812);
#18864=AXIS2_PLACEMENT_3D('',#41124,#20813,#20814);
#18865=AXIS2_PLACEMENT_3D('',#41132,#20815,#20816);
#18866=AXIS2_PLACEMENT_3D('',#41133,#20817,#20818);
#18867=AXIS2_PLACEMENT_3D('',#41623,#20819,#20820);
#18868=AXIS2_PLACEMENT_3D('',#41626,#20823,#20824);
#18869=AXIS2_PLACEMENT_3D('',#41628,#20826,#20827);
#18870=AXIS2_PLACEMENT_3D('',#41630,#20829,#20830);
#18871=AXIS2_PLACEMENT_3D('',#41632,#20832,#20833);
#18872=AXIS2_PLACEMENT_3D('',#41634,#20835,#20836);
#18873=AXIS2_PLACEMENT_3D('',#41636,#20838,#20839);
#18874=AXIS2_PLACEMENT_3D('',#41638,#20841,#20842);
#18875=AXIS2_PLACEMENT_3D('',#41639,#20843,#20844);
#18876=AXIS2_PLACEMENT_3D('',#41641,#20846,#20847);
#18877=AXIS2_PLACEMENT_3D('',#41643,#20849,#20850);
#18878=AXIS2_PLACEMENT_3D('',#41645,#20852,#20853);
#18879=AXIS2_PLACEMENT_3D('',#41647,#20855,#20856);
#18880=AXIS2_PLACEMENT_3D('',#41649,#20858,#20859);
#18881=AXIS2_PLACEMENT_3D('',#41651,#20861,#20862);
#18882=AXIS2_PLACEMENT_3D('',#41652,#20863,#20864);
#18883=AXIS2_PLACEMENT_3D('',#41654,#20865,#20866);
#18884=AXIS2_PLACEMENT_3D('',#41656,#20868,#20869);
#18885=AXIS2_PLACEMENT_3D('',#41658,#20871,#20872);
#18886=AXIS2_PLACEMENT_3D('',#41660,#20874,#20875);
#18887=AXIS2_PLACEMENT_3D('',#41662,#20876,#20877);
#18888=AXIS2_PLACEMENT_3D('',#41664,#20879,#20880);
#18889=AXIS2_PLACEMENT_3D('',#41666,#20881,#20882);
#18890=AXIS2_PLACEMENT_3D('',#41667,#20883,#20884);
#18891=AXIS2_PLACEMENT_3D('',#41669,#20885,#20886);
#18892=AXIS2_PLACEMENT_3D('',#41671,#20888,#20889);
#18893=AXIS2_PLACEMENT_3D('',#41673,#20890,#20891);
#18894=AXIS2_PLACEMENT_3D('',#41675,#20893,#20894);
#18895=AXIS2_PLACEMENT_3D('',#41677,#20895,#20896);
#18896=AXIS2_PLACEMENT_3D('',#41679,#20898,#20899);
#18897=AXIS2_PLACEMENT_3D('',#41681,#20900,#20901);
#18898=AXIS2_PLACEMENT_3D('',#41683,#20903,#20904);
#18899=AXIS2_PLACEMENT_3D('',#41685,#20905,#20906);
#18900=AXIS2_PLACEMENT_3D('',#41686,#20907,#20908);
#18901=AXIS2_PLACEMENT_3D('',#41688,#20909,#20910);
#18902=AXIS2_PLACEMENT_3D('',#41690,#20912,#20913);
#18903=AXIS2_PLACEMENT_3D('',#41692,#20914,#20915);
#18904=AXIS2_PLACEMENT_3D('',#41694,#20917,#20918);
#18905=AXIS2_PLACEMENT_3D('',#41696,#20919,#20920);
#18906=AXIS2_PLACEMENT_3D('',#41698,#20922,#20923);
#18907=AXIS2_PLACEMENT_3D('',#41700,#20924,#20925);
#18908=AXIS2_PLACEMENT_3D('',#41702,#20927,#20928);
#18909=AXIS2_PLACEMENT_3D('',#41704,#20929,#20930);
#18910=AXIS2_PLACEMENT_3D('',#41706,#20932,#20933);
#18911=AXIS2_PLACEMENT_3D('',#41708,#20935,#20936);
#18912=AXIS2_PLACEMENT_3D('',#41709,#20937,#20938);
#18913=AXIS2_PLACEMENT_3D('',#41710,#20939,#20940);
#18914=AXIS2_PLACEMENT_3D('',#41712,#20941,#20942);
#18915=AXIS2_PLACEMENT_3D('',#41714,#20944,#20945);
#18916=AXIS2_PLACEMENT_3D('',#41715,#20946,#20947);
#18917=AXIS2_PLACEMENT_3D('',#41830,#20948,#20949);
#18918=AXIS2_PLACEMENT_3D('',#43722,#20956,#20957);
#18919=AXIS2_PLACEMENT_3D('',#43725,#20960,#20961);
#18920=AXIS2_PLACEMENT_3D('',#43726,#20962,#20963);
#18921=AXIS2_PLACEMENT_3D('',#43727,#20964,#20965);
#18922=AXIS2_PLACEMENT_3D('',#43728,#20966,#20967);
#18923=AXIS2_PLACEMENT_3D('',#43730,#20968,#20969);
#18924=AXIS2_PLACEMENT_3D('',#43733,#20971,#20972);
#18925=AXIS2_PLACEMENT_3D('',#43734,#20973,#20974);
#18926=AXIS2_PLACEMENT_3D('',#43736,#20975,#20976);
#18927=AXIS2_PLACEMENT_3D('',#43738,#20978,#20979);
#18928=AXIS2_PLACEMENT_3D('',#43740,#20980,#20981);
#18929=AXIS2_PLACEMENT_3D('',#43742,#20983,#20984);
#18930=AXIS2_PLACEMENT_3D('',#43744,#20985,#20986);
#18931=AXIS2_PLACEMENT_3D('',#43745,#20987,#20988);
#18932=AXIS2_PLACEMENT_3D('',#43748,#20990,#20991);
#18933=AXIS2_PLACEMENT_3D('',#43749,#20992,#20993);
#18934=AXIS2_PLACEMENT_3D('',#43752,#20995,#20996);
#18935=AXIS2_PLACEMENT_3D('',#43753,#20997,#20998);
#18936=AXIS2_PLACEMENT_3D('',#43756,#21000,#21001);
#18937=AXIS2_PLACEMENT_3D('',#43757,#21002,#21003);
#18938=AXIS2_PLACEMENT_3D('',#43758,#21004,#21005);
#18939=AXIS2_PLACEMENT_3D('',#43759,#21006,#21007);
#18940=AXIS2_PLACEMENT_3D('',#43768,#21012,#21013);
#18941=AXIS2_PLACEMENT_3D('',#43775,#21017,#21018);
#18942=AXIS2_PLACEMENT_3D('',#43776,#21019,#21020);
#18943=AXIS2_PLACEMENT_3D('',#43782,#21024,#21025);
#18944=AXIS2_PLACEMENT_3D('',#43787,#21028,#21029);
#18945=AXIS2_PLACEMENT_3D('',#43789,#21030,#21031);
#18946=AXIS2_PLACEMENT_3D('',#43791,#21032,#21033);
#18947=AXIS2_PLACEMENT_3D('',#43793,#21034,#21035);
#18948=AXIS2_PLACEMENT_3D('',#43963,#21120,#21121);
#18949=AXIS2_PLACEMENT_3D('',#43964,#21122,#21123);
#18950=AXIS2_PLACEMENT_3D('',#43975,#21124,#21125);
#18951=AXIS2_PLACEMENT_3D('',#43984,#21126,#21127);
#18952=AXIS2_PLACEMENT_3D('',#43993,#21130,#21131);
#18953=AXIS2_PLACEMENT_3D('',#43995,#21132,#21133);
#18954=AXIS2_PLACEMENT_3D('',#44001,#21134,#21135);
#18955=AXIS2_PLACEMENT_3D('',#44010,#21136,#21137);
#18956=AXIS2_PLACEMENT_3D('',#44013,#21140,#21141);
#18957=AXIS2_PLACEMENT_3D('',#44015,#21143,#21144);
#18958=AXIS2_PLACEMENT_3D('',#44018,#21146,#21147);
#18959=AXIS2_PLACEMENT_3D('',#44020,#21148,#21149);
#18960=AXIS2_PLACEMENT_3D('',#44022,#21150,#21151);
#18961=AXIS2_PLACEMENT_3D('',#44192,#21236,#21237);
#18962=AXIS2_PLACEMENT_3D('',#44193,#21238,#21239);
#18963=AXIS2_PLACEMENT_3D('',#44194,#21240,#21241);
#18964=AXIS2_PLACEMENT_3D('',#44197,#21243,#21244);
#18965=AXIS2_PLACEMENT_3D('',#44198,#21245,#21246);
#18966=AXIS2_PLACEMENT_3D('',#44201,#21248,#21249);
#18967=AXIS2_PLACEMENT_3D('',#44202,#21250,#21251);
#18968=AXIS2_PLACEMENT_3D('',#44204,#21253,#21254);
#18969=AXIS2_PLACEMENT_3D('',#44207,#21256,#21257);
#18970=AXIS2_PLACEMENT_3D('',#44208,#21258,#21259);
#18971=AXIS2_PLACEMENT_3D('',#44211,#21261,#21262);
#18972=AXIS2_PLACEMENT_3D('',#44212,#21263,#21264);
#18973=AXIS2_PLACEMENT_3D('',#44214,#21266,#21267);
#18974=AXIS2_PLACEMENT_3D('',#44217,#21269,#21270);
#18975=AXIS2_PLACEMENT_3D('',#44218,#21271,#21272);
#18976=AXIS2_PLACEMENT_3D('',#44221,#21274,#21275);
#18977=AXIS2_PLACEMENT_3D('',#44222,#21276,#21277);
#18978=AXIS2_PLACEMENT_3D('',#44224,#21279,#21280);
#18979=AXIS2_PLACEMENT_3D('',#44227,#21282,#21283);
#18980=AXIS2_PLACEMENT_3D('',#44228,#21284,#21285);
#18981=AXIS2_PLACEMENT_3D('',#44271,#21287,#21288);
#18982=AXIS2_PLACEMENT_3D('',#44277,#21292,#21293);
#18983=AXIS2_PLACEMENT_3D('',#44281,#21296,#21297);
#18984=AXIS2_PLACEMENT_3D('',#44285,#21300,#21301);
#18985=AXIS2_PLACEMENT_3D('',#44289,#21304,#21305);
#18986=AXIS2_PLACEMENT_3D('',#44293,#21308,#21309);
#18987=AXIS2_PLACEMENT_3D('',#44297,#21312,#21313);
#18988=AXIS2_PLACEMENT_3D('',#44301,#21316,#21317);
#18989=AXIS2_PLACEMENT_3D('',#44305,#21320,#21321);
#18990=AXIS2_PLACEMENT_3D('',#44309,#21324,#21325);
#18991=AXIS2_PLACEMENT_3D('',#44313,#21328,#21329);
#18992=AXIS2_PLACEMENT_3D('',#44317,#21332,#21333);
#18993=AXIS2_PLACEMENT_3D('',#44321,#21336,#21337);
#18994=AXIS2_PLACEMENT_3D('',#44325,#21340,#21341);
#18995=AXIS2_PLACEMENT_3D('',#44327,#21343,#21344);
#18996=AXIS2_PLACEMENT_3D('',#44328,#21345,#21346);
#18997=AXIS2_PLACEMENT_3D('',#44334,#21350,#21351);
#18998=AXIS2_PLACEMENT_3D('',#44338,#21354,#21355);
#18999=AXIS2_PLACEMENT_3D('',#44342,#21358,#21359);
#19000=AXIS2_PLACEMENT_3D('',#44346,#21362,#21363);
#19001=AXIS2_PLACEMENT_3D('',#44350,#21366,#21367);
#19002=AXIS2_PLACEMENT_3D('',#44354,#21370,#21371);
#19003=AXIS2_PLACEMENT_3D('',#44358,#21374,#21375);
#19004=AXIS2_PLACEMENT_3D('',#44362,#21378,#21379);
#19005=AXIS2_PLACEMENT_3D('',#44366,#21382,#21383);
#19006=AXIS2_PLACEMENT_3D('',#44370,#21386,#21387);
#19007=AXIS2_PLACEMENT_3D('',#44374,#21390,#21391);
#19008=AXIS2_PLACEMENT_3D('',#44378,#21394,#21395);
#19009=AXIS2_PLACEMENT_3D('',#44382,#21398,#21399);
#19010=AXIS2_PLACEMENT_3D('',#44384,#21401,#21402);
#19011=AXIS2_PLACEMENT_3D('',#44385,#21403,#21404);
#19012=AXIS2_PLACEMENT_3D('',#44391,#21408,#21409);
#19013=AXIS2_PLACEMENT_3D('',#44395,#21412,#21413);
#19014=AXIS2_PLACEMENT_3D('',#44399,#21416,#21417);
#19015=AXIS2_PLACEMENT_3D('',#44403,#21420,#21421);
#19016=AXIS2_PLACEMENT_3D('',#44407,#21424,#21425);
#19017=AXIS2_PLACEMENT_3D('',#44411,#21428,#21429);
#19018=AXIS2_PLACEMENT_3D('',#44415,#21432,#21433);
#19019=AXIS2_PLACEMENT_3D('',#44419,#21436,#21437);
#19020=AXIS2_PLACEMENT_3D('',#44423,#21440,#21441);
#19021=AXIS2_PLACEMENT_3D('',#44427,#21444,#21445);
#19022=AXIS2_PLACEMENT_3D('',#44431,#21448,#21449);
#19023=AXIS2_PLACEMENT_3D('',#44435,#21452,#21453);
#19024=AXIS2_PLACEMENT_3D('',#44439,#21456,#21457);
#19025=AXIS2_PLACEMENT_3D('',#44441,#21459,#21460);
#19026=AXIS2_PLACEMENT_3D('',#44442,#21461,#21462);
#19027=AXIS2_PLACEMENT_3D('',#44448,#21466,#21467);
#19028=AXIS2_PLACEMENT_3D('',#44452,#21470,#21471);
#19029=AXIS2_PLACEMENT_3D('',#44456,#21474,#21475);
#19030=AXIS2_PLACEMENT_3D('',#44460,#21478,#21479);
#19031=AXIS2_PLACEMENT_3D('',#44464,#21482,#21483);
#19032=AXIS2_PLACEMENT_3D('',#44468,#21486,#21487);
#19033=AXIS2_PLACEMENT_3D('',#44472,#21490,#21491);
#19034=AXIS2_PLACEMENT_3D('',#44476,#21494,#21495);
#19035=AXIS2_PLACEMENT_3D('',#44480,#21498,#21499);
#19036=AXIS2_PLACEMENT_3D('',#44484,#21502,#21503);
#19037=AXIS2_PLACEMENT_3D('',#44488,#21506,#21507);
#19038=AXIS2_PLACEMENT_3D('',#44492,#21510,#21511);
#19039=AXIS2_PLACEMENT_3D('',#44496,#21514,#21515);
#19040=AXIS2_PLACEMENT_3D('',#44498,#21517,#21518);
#19041=AXIS2_PLACEMENT_3D('',#44499,#21519,#21520);
#19042=AXIS2_PLACEMENT_3D('',#44505,#21524,#21525);
#19043=AXIS2_PLACEMENT_3D('',#44509,#21528,#21529);
#19044=AXIS2_PLACEMENT_3D('',#44513,#21532,#21533);
#19045=AXIS2_PLACEMENT_3D('',#44517,#21536,#21537);
#19046=AXIS2_PLACEMENT_3D('',#44521,#21540,#21541);
#19047=AXIS2_PLACEMENT_3D('',#44525,#21544,#21545);
#19048=AXIS2_PLACEMENT_3D('',#44529,#21548,#21549);
#19049=AXIS2_PLACEMENT_3D('',#44533,#21552,#21553);
#19050=AXIS2_PLACEMENT_3D('',#44537,#21556,#21557);
#19051=AXIS2_PLACEMENT_3D('',#44541,#21560,#21561);
#19052=AXIS2_PLACEMENT_3D('',#44545,#21564,#21565);
#19053=AXIS2_PLACEMENT_3D('',#44549,#21568,#21569);
#19054=AXIS2_PLACEMENT_3D('',#44553,#21572,#21573);
#19055=AXIS2_PLACEMENT_3D('',#44555,#21575,#21576);
#19056=AXIS2_PLACEMENT_3D('',#44556,#21577,#21578);
#19057=AXIS2_PLACEMENT_3D('',#44562,#21582,#21583);
#19058=AXIS2_PLACEMENT_3D('',#44566,#21586,#21587);
#19059=AXIS2_PLACEMENT_3D('',#44570,#21590,#21591);
#19060=AXIS2_PLACEMENT_3D('',#44574,#21594,#21595);
#19061=AXIS2_PLACEMENT_3D('',#44578,#21598,#21599);
#19062=AXIS2_PLACEMENT_3D('',#44582,#21602,#21603);
#19063=AXIS2_PLACEMENT_3D('',#44586,#21606,#21607);
#19064=AXIS2_PLACEMENT_3D('',#44590,#21610,#21611);
#19065=AXIS2_PLACEMENT_3D('',#44594,#21614,#21615);
#19066=AXIS2_PLACEMENT_3D('',#44598,#21618,#21619);
#19067=AXIS2_PLACEMENT_3D('',#44602,#21622,#21623);
#19068=AXIS2_PLACEMENT_3D('',#44606,#21626,#21627);
#19069=AXIS2_PLACEMENT_3D('',#44610,#21630,#21631);
#19070=AXIS2_PLACEMENT_3D('',#44612,#21633,#21634);
#19071=AXIS2_PLACEMENT_3D('',#44613,#21635,#21636);
#19072=AXIS2_PLACEMENT_3D('',#44619,#21640,#21641);
#19073=AXIS2_PLACEMENT_3D('',#44623,#21644,#21645);
#19074=AXIS2_PLACEMENT_3D('',#44627,#21648,#21649);
#19075=AXIS2_PLACEMENT_3D('',#44631,#21652,#21653);
#19076=AXIS2_PLACEMENT_3D('',#44635,#21656,#21657);
#19077=AXIS2_PLACEMENT_3D('',#44639,#21660,#21661);
#19078=AXIS2_PLACEMENT_3D('',#44643,#21664,#21665);
#19079=AXIS2_PLACEMENT_3D('',#44647,#21668,#21669);
#19080=AXIS2_PLACEMENT_3D('',#44651,#21672,#21673);
#19081=AXIS2_PLACEMENT_3D('',#44655,#21676,#21677);
#19082=AXIS2_PLACEMENT_3D('',#44659,#21680,#21681);
#19083=AXIS2_PLACEMENT_3D('',#44663,#21684,#21685);
#19084=AXIS2_PLACEMENT_3D('',#44667,#21688,#21689);
#19085=AXIS2_PLACEMENT_3D('',#44669,#21691,#21692);
#19086=AXIS2_PLACEMENT_3D('',#44670,#21693,#21694);
#19087=AXIS2_PLACEMENT_3D('',#44676,#21698,#21699);
#19088=AXIS2_PLACEMENT_3D('',#44680,#21702,#21703);
#19089=AXIS2_PLACEMENT_3D('',#44684,#21706,#21707);
#19090=AXIS2_PLACEMENT_3D('',#44688,#21710,#21711);
#19091=AXIS2_PLACEMENT_3D('',#44692,#21714,#21715);
#19092=AXIS2_PLACEMENT_3D('',#44696,#21718,#21719);
#19093=AXIS2_PLACEMENT_3D('',#44700,#21722,#21723);
#19094=AXIS2_PLACEMENT_3D('',#44704,#21726,#21727);
#19095=AXIS2_PLACEMENT_3D('',#44708,#21730,#21731);
#19096=AXIS2_PLACEMENT_3D('',#44712,#21734,#21735);
#19097=AXIS2_PLACEMENT_3D('',#44716,#21738,#21739);
#19098=AXIS2_PLACEMENT_3D('',#44720,#21742,#21743);
#19099=AXIS2_PLACEMENT_3D('',#44724,#21746,#21747);
#19100=AXIS2_PLACEMENT_3D('',#44726,#21749,#21750);
#19101=AXIS2_PLACEMENT_3D('',#44727,#21751,#21752);
#19102=AXIS2_PLACEMENT_3D('',#44733,#21756,#21757);
#19103=AXIS2_PLACEMENT_3D('',#44737,#21760,#21761);
#19104=AXIS2_PLACEMENT_3D('',#44741,#21764,#21765);
#19105=AXIS2_PLACEMENT_3D('',#44745,#21768,#21769);
#19106=AXIS2_PLACEMENT_3D('',#44749,#21772,#21773);
#19107=AXIS2_PLACEMENT_3D('',#44753,#21776,#21777);
#19108=AXIS2_PLACEMENT_3D('',#44757,#21780,#21781);
#19109=AXIS2_PLACEMENT_3D('',#44761,#21784,#21785);
#19110=AXIS2_PLACEMENT_3D('',#44765,#21788,#21789);
#19111=AXIS2_PLACEMENT_3D('',#44769,#21792,#21793);
#19112=AXIS2_PLACEMENT_3D('',#44773,#21796,#21797);
#19113=AXIS2_PLACEMENT_3D('',#44777,#21800,#21801);
#19114=AXIS2_PLACEMENT_3D('',#44781,#21804,#21805);
#19115=AXIS2_PLACEMENT_3D('',#44783,#21807,#21808);
#19116=AXIS2_PLACEMENT_3D('',#44784,#21809,#21810);
#19117=AXIS2_PLACEMENT_3D('',#44790,#21814,#21815);
#19118=AXIS2_PLACEMENT_3D('',#44794,#21818,#21819);
#19119=AXIS2_PLACEMENT_3D('',#44798,#21822,#21823);
#19120=AXIS2_PLACEMENT_3D('',#44802,#21826,#21827);
#19121=AXIS2_PLACEMENT_3D('',#44806,#21830,#21831);
#19122=AXIS2_PLACEMENT_3D('',#44810,#21834,#21835);
#19123=AXIS2_PLACEMENT_3D('',#44814,#21838,#21839);
#19124=AXIS2_PLACEMENT_3D('',#44818,#21842,#21843);
#19125=AXIS2_PLACEMENT_3D('',#44822,#21846,#21847);
#19126=AXIS2_PLACEMENT_3D('',#44826,#21850,#21851);
#19127=AXIS2_PLACEMENT_3D('',#44830,#21854,#21855);
#19128=AXIS2_PLACEMENT_3D('',#44834,#21858,#21859);
#19129=AXIS2_PLACEMENT_3D('',#44838,#21862,#21863);
#19130=AXIS2_PLACEMENT_3D('',#44840,#21865,#21866);
#19131=AXIS2_PLACEMENT_3D('',#44841,#21867,#21868);
#19132=AXIS2_PLACEMENT_3D('',#44847,#21872,#21873);
#19133=AXIS2_PLACEMENT_3D('',#44851,#21876,#21877);
#19134=AXIS2_PLACEMENT_3D('',#44855,#21880,#21881);
#19135=AXIS2_PLACEMENT_3D('',#44859,#21884,#21885);
#19136=AXIS2_PLACEMENT_3D('',#44863,#21888,#21889);
#19137=AXIS2_PLACEMENT_3D('',#44867,#21892,#21893);
#19138=AXIS2_PLACEMENT_3D('',#44871,#21896,#21897);
#19139=AXIS2_PLACEMENT_3D('',#44875,#21900,#21901);
#19140=AXIS2_PLACEMENT_3D('',#44879,#21904,#21905);
#19141=AXIS2_PLACEMENT_3D('',#44883,#21908,#21909);
#19142=AXIS2_PLACEMENT_3D('',#44887,#21912,#21913);
#19143=AXIS2_PLACEMENT_3D('',#44891,#21916,#21917);
#19144=AXIS2_PLACEMENT_3D('',#44895,#21920,#21921);
#19145=AXIS2_PLACEMENT_3D('',#44897,#21923,#21924);
#19146=AXIS2_PLACEMENT_3D('',#44898,#21925,#21926);
#19147=AXIS2_PLACEMENT_3D('',#44904,#21930,#21931);
#19148=AXIS2_PLACEMENT_3D('',#44908,#21934,#21935);
#19149=AXIS2_PLACEMENT_3D('',#44912,#21938,#21939);
#19150=AXIS2_PLACEMENT_3D('',#44916,#21942,#21943);
#19151=AXIS2_PLACEMENT_3D('',#44920,#21946,#21947);
#19152=AXIS2_PLACEMENT_3D('',#44924,#21950,#21951);
#19153=AXIS2_PLACEMENT_3D('',#44928,#21954,#21955);
#19154=AXIS2_PLACEMENT_3D('',#44932,#21958,#21959);
#19155=AXIS2_PLACEMENT_3D('',#44936,#21962,#21963);
#19156=AXIS2_PLACEMENT_3D('',#44940,#21966,#21967);
#19157=AXIS2_PLACEMENT_3D('',#44944,#21970,#21971);
#19158=AXIS2_PLACEMENT_3D('',#44948,#21974,#21975);
#19159=AXIS2_PLACEMENT_3D('',#44952,#21978,#21979);
#19160=AXIS2_PLACEMENT_3D('',#44954,#21981,#21982);
#19161=AXIS2_PLACEMENT_3D('',#44955,#21983,#21984);
#19162=AXIS2_PLACEMENT_3D('',#44958,#21987,#21988);
#19163=AXIS2_PLACEMENT_3D('',#44959,#21989,#21990);
#19164=AXIS2_PLACEMENT_3D('',#44960,#21991,#21992);
#19165=AXIS2_PLACEMENT_3D('',#44962,#21993,#21994);
#19166=AXIS2_PLACEMENT_3D('',#44965,#21996,#21997);
#19167=AXIS2_PLACEMENT_3D('',#44966,#21998,#21999);
#19168=AXIS2_PLACEMENT_3D('',#44967,#22000,#22001);
#19169=AXIS2_PLACEMENT_3D('',#44969,#22002,#22003);
#19170=AXIS2_PLACEMENT_3D('',#44972,#22005,#22006);
#19171=AXIS2_PLACEMENT_3D('',#44973,#22007,#22008);
#19172=AXIS2_PLACEMENT_3D('',#44974,#22009,#22010);
#19173=AXIS2_PLACEMENT_3D('',#44976,#22011,#22012);
#19174=AXIS2_PLACEMENT_3D('',#44979,#22014,#22015);
#19175=AXIS2_PLACEMENT_3D('',#44980,#22016,#22017);
#19176=AXIS2_PLACEMENT_3D('',#44981,#22018,#22019);
#19177=AXIS2_PLACEMENT_3D('',#44983,#22020,#22021);
#19178=AXIS2_PLACEMENT_3D('',#44986,#22023,#22024);
#19179=AXIS2_PLACEMENT_3D('',#44987,#22025,#22026);
#19180=AXIS2_PLACEMENT_3D('',#44988,#22027,#22028);
#19181=AXIS2_PLACEMENT_3D('',#44990,#22029,#22030);
#19182=AXIS2_PLACEMENT_3D('',#44993,#22032,#22033);
#19183=AXIS2_PLACEMENT_3D('',#44994,#22034,#22035);
#19184=AXIS2_PLACEMENT_3D('',#44995,#22036,#22037);
#19185=AXIS2_PLACEMENT_3D('',#44997,#22038,#22039);
#19186=AXIS2_PLACEMENT_3D('',#45000,#22041,#22042);
#19187=AXIS2_PLACEMENT_3D('',#45001,#22043,#22044);
#19188=AXIS2_PLACEMENT_3D('',#45002,#22045,#22046);
#19189=AXIS2_PLACEMENT_3D('',#45004,#22047,#22048);
#19190=AXIS2_PLACEMENT_3D('',#45007,#22050,#22051);
#19191=AXIS2_PLACEMENT_3D('',#45008,#22052,#22053);
#19192=AXIS2_PLACEMENT_3D('',#45010,#22054,#22055);
#19193=AXIS2_PLACEMENT_3D('',#45011,#22056,#22057);
#19194=AXIS2_PLACEMENT_3D('',#45013,#22058,#22059);
#19195=AXIS2_PLACEMENT_3D('',#45014,#22060,#22061);
#19196=AXIS2_PLACEMENT_3D('',#45016,#22062,#22063);
#19197=AXIS2_PLACEMENT_3D('',#45018,#22065,#22066);
#19198=AXIS2_PLACEMENT_3D('',#45020,#22067,#22068);
#19199=AXIS2_PLACEMENT_3D('',#45023,#22070,#22071);
#19200=AXIS2_PLACEMENT_3D('',#45024,#22072,#22073);
#19201=AXIS2_PLACEMENT_3D('',#45026,#22074,#22075);
#19202=AXIS2_PLACEMENT_3D('',#45028,#22077,#22078);
#19203=AXIS2_PLACEMENT_3D('',#45030,#22079,#22080);
#19204=AXIS2_PLACEMENT_3D('',#45031,#22081,#22082);
#19205=AXIS2_PLACEMENT_3D('',#45033,#22083,#22084);
#19206=AXIS2_PLACEMENT_3D('',#45035,#22086,#22087);
#19207=AXIS2_PLACEMENT_3D('',#45037,#22088,#22089);
#19208=AXIS2_PLACEMENT_3D('',#45039,#22091,#22092);
#19209=AXIS2_PLACEMENT_3D('',#45041,#22093,#22094);
#19210=AXIS2_PLACEMENT_3D('',#45043,#22096,#22097);
#19211=AXIS2_PLACEMENT_3D('',#45045,#22098,#22099);
#19212=AXIS2_PLACEMENT_3D('',#45046,#22100,#22101);
#19213=AXIS2_PLACEMENT_3D('',#45048,#22102,#22103);
#19214=AXIS2_PLACEMENT_3D('',#45050,#22105,#22106);
#19215=AXIS2_PLACEMENT_3D('',#45052,#22108,#22109);
#19216=AXIS2_PLACEMENT_3D('',#45054,#22110,#22111);
#19217=AXIS2_PLACEMENT_3D('',#45056,#22113,#22114);
#19218=AXIS2_PLACEMENT_3D('',#45058,#22115,#22116);
#19219=AXIS2_PLACEMENT_3D('',#45059,#22117,#22118);
#19220=AXIS2_PLACEMENT_3D('',#45062,#22120,#22121);
#19221=AXIS2_PLACEMENT_3D('',#45063,#22122,#22123);
#19222=AXIS2_PLACEMENT_3D('',#45066,#22125,#22126);
#19223=AXIS2_PLACEMENT_3D('',#45067,#22127,#22128);
#19224=AXIS2_PLACEMENT_3D('',#45070,#22130,#22131);
#19225=AXIS2_PLACEMENT_3D('',#45071,#22132,#22133);
#19226=AXIS2_PLACEMENT_3D('',#45072,#22134,#22135);
#19227=AXIS2_PLACEMENT_3D('',#45169,#22136,#22137);
#19228=AXIS2_PLACEMENT_3D('',#47060,#22144,#22145);
#19229=AXIS2_PLACEMENT_3D('',#47063,#22148,#22149);
#19230=AXIS2_PLACEMENT_3D('',#47064,#22150,#22151);
#19231=AXIS2_PLACEMENT_3D('',#47065,#22152,#22153);
#19232=AXIS2_PLACEMENT_3D('',#47376,#22154,#22155);
#19233=AXIS2_PLACEMENT_3D('',#47427,#22156,#22157);
#19234=AXIS2_PLACEMENT_3D('',#47480,#22158,#22159);
#19235=AXIS2_PLACEMENT_3D('',#47488,#22160,#22161);
#19236=AXIS2_PLACEMENT_3D('',#47494,#22162,#22163);
#19237=AXIS2_PLACEMENT_3D('',#47495,#22164,#22165);
#19238=AXIS2_PLACEMENT_3D('',#47514,#22166,#22167);
#19239=AXIS2_PLACEMENT_3D('',#47528,#22168,#22169);
#19240=AXIS2_PLACEMENT_3D('',#47542,#22170,#22171);
#19241=AXIS2_PLACEMENT_3D('',#47556,#22172,#22173);
#19242=AXIS2_PLACEMENT_3D('',#47570,#22174,#22175);
#19243=AXIS2_PLACEMENT_3D('',#47584,#22176,#22177);
#19244=AXIS2_PLACEMENT_3D('',#47598,#22178,#22179);
#19245=AXIS2_PLACEMENT_3D('',#47612,#22180,#22181);
#19246=AXIS2_PLACEMENT_3D('',#47626,#22182,#22183);
#19247=AXIS2_PLACEMENT_3D('',#47640,#22184,#22185);
#19248=AXIS2_PLACEMENT_3D('',#47654,#22186,#22187);
#19249=AXIS2_PLACEMENT_3D('',#47668,#22188,#22189);
#19250=AXIS2_PLACEMENT_3D('',#47682,#22190,#22191);
#19251=AXIS2_PLACEMENT_3D('',#47685,#22193,#22194);
#19252=AXIS2_PLACEMENT_3D('',#47687,#22195,#22196);
#19253=AXIS2_PLACEMENT_3D('',#47701,#22197,#22198);
#19254=AXIS2_PLACEMENT_3D('',#47715,#22199,#22200);
#19255=AXIS2_PLACEMENT_3D('',#47729,#22201,#22202);
#19256=AXIS2_PLACEMENT_3D('',#47743,#22203,#22204);
#19257=AXIS2_PLACEMENT_3D('',#47757,#22205,#22206);
#19258=AXIS2_PLACEMENT_3D('',#47771,#22207,#22208);
#19259=AXIS2_PLACEMENT_3D('',#47785,#22209,#22210);
#19260=AXIS2_PLACEMENT_3D('',#47799,#22211,#22212);
#19261=AXIS2_PLACEMENT_3D('',#47813,#22213,#22214);
#19262=AXIS2_PLACEMENT_3D('',#47827,#22215,#22216);
#19263=AXIS2_PLACEMENT_3D('',#47841,#22217,#22218);
#19264=AXIS2_PLACEMENT_3D('',#47855,#22219,#22220);
#19265=AXIS2_PLACEMENT_3D('',#47869,#22221,#22222);
#19266=AXIS2_PLACEMENT_3D('',#47883,#22223,#22224);
#19267=AXIS2_PLACEMENT_3D('',#47890,#22225,#22226);
#19268=AXIS2_PLACEMENT_3D('',#47901,#22227,#22228);
#19269=AXIS2_PLACEMENT_3D('',#47902,#22229,#22230);
#19270=AXIS2_PLACEMENT_3D('',#47913,#22231,#22232);
#19271=AXIS2_PLACEMENT_3D('',#47914,#22233,#22234);
#19272=AXIS2_PLACEMENT_3D('',#47925,#22235,#22236);
#19273=AXIS2_PLACEMENT_3D('',#47926,#22237,#22238);
#19274=AXIS2_PLACEMENT_3D('',#47937,#22239,#22240);
#19275=AXIS2_PLACEMENT_3D('',#47938,#22241,#22242);
#19276=AXIS2_PLACEMENT_3D('',#47949,#22243,#22244);
#19277=AXIS2_PLACEMENT_3D('',#47950,#22245,#22246);
#19278=AXIS2_PLACEMENT_3D('',#47961,#22247,#22248);
#19279=AXIS2_PLACEMENT_3D('',#47962,#22249,#22250);
#19280=AXIS2_PLACEMENT_3D('',#47973,#22251,#22252);
#19281=AXIS2_PLACEMENT_3D('',#47974,#22253,#22254);
#19282=AXIS2_PLACEMENT_3D('',#47985,#22255,#22256);
#19283=AXIS2_PLACEMENT_3D('',#47986,#22257,#22258);
#19284=AXIS2_PLACEMENT_3D('',#47997,#22259,#22260);
#19285=AXIS2_PLACEMENT_3D('',#47998,#22261,#22262);
#19286=AXIS2_PLACEMENT_3D('',#48009,#22263,#22264);
#19287=AXIS2_PLACEMENT_3D('',#48010,#22265,#22266);
#19288=AXIS2_PLACEMENT_3D('',#48021,#22267,#22268);
#19289=AXIS2_PLACEMENT_3D('',#48022,#22269,#22270);
#19290=AXIS2_PLACEMENT_3D('',#48033,#22271,#22272);
#19291=AXIS2_PLACEMENT_3D('',#48034,#22273,#22274);
#19292=AXIS2_PLACEMENT_3D('',#48045,#22275,#22276);
#19293=AXIS2_PLACEMENT_3D('',#48046,#22277,#22278);
#19294=AXIS2_PLACEMENT_3D('',#48048,#22279,#22280);
#19295=AXIS2_PLACEMENT_3D('',#48052,#22282,#22283);
#19296=AXIS2_PLACEMENT_3D('',#48053,#22284,#22285);
#19297=AXIS2_PLACEMENT_3D('',#48054,#22286,#22287);
#19298=AXIS2_PLACEMENT_3D('',#48057,#22288,#22289);
#19299=AXIS2_PLACEMENT_3D('',#48058,#22290,#22291);
#19300=AXIS2_PLACEMENT_3D('',#48060,#22293,#22294);
#19301=AXIS2_PLACEMENT_3D('',#48062,#22295,#22296);
#19302=AXIS2_PLACEMENT_3D('',#48063,#22297,#22298);
#19303=AXIS2_PLACEMENT_3D('',#48066,#22300,#22301);
#19304=AXIS2_PLACEMENT_3D('',#48067,#22302,#22303);
#19305=AXIS2_PLACEMENT_3D('',#48069,#22304,#22305);
#19306=AXIS2_PLACEMENT_3D('',#48245,#22306,#22307);
#19307=AXIS2_PLACEMENT_3D('',#48256,#22308,#22309);
#19308=AXIS2_PLACEMENT_3D('',#48533,#22310,#22311);
#19309=AXIS2_PLACEMENT_3D('',#48535,#22312,#22313);
#19310=AXIS2_PLACEMENT_3D('',#48715,#22314,#22315);
#19311=AXIS2_PLACEMENT_3D('',#48726,#22316,#22317);
#19312=AXIS2_PLACEMENT_3D('',#49003,#22318,#22319);
#19313=AXIS2_PLACEMENT_3D('',#49005,#22320,#22321);
#19314=AXIS2_PLACEMENT_3D('',#49185,#22322,#22323);
#19315=AXIS2_PLACEMENT_3D('',#49196,#22324,#22325);
#19316=AXIS2_PLACEMENT_3D('',#49473,#22326,#22327);
#19317=AXIS2_PLACEMENT_3D('',#49475,#22328,#22329);
#19318=AXIS2_PLACEMENT_3D('',#49655,#22330,#22331);
#19319=AXIS2_PLACEMENT_3D('',#49668,#22332,#22333);
#19320=AXIS2_PLACEMENT_3D('',#49945,#22334,#22335);
#19321=AXIS2_PLACEMENT_3D('',#49947,#22336,#22337);
#19322=AXIS2_PLACEMENT_3D('',#50127,#22338,#22339);
#19323=AXIS2_PLACEMENT_3D('',#50140,#22340,#22341);
#19324=AXIS2_PLACEMENT_3D('',#50417,#22342,#22343);
#19325=AXIS2_PLACEMENT_3D('',#50419,#22344,#22345);
#19326=AXIS2_PLACEMENT_3D('',#50599,#22346,#22347);
#19327=AXIS2_PLACEMENT_3D('',#50610,#22348,#22349);
#19328=AXIS2_PLACEMENT_3D('',#50887,#22350,#22351);
#19329=AXIS2_PLACEMENT_3D('',#50889,#22352,#22353);
#19330=AXIS2_PLACEMENT_3D('',#51039,#22354,#22355);
#19331=AXIS2_PLACEMENT_3D('',#51045,#22356,#22357);
#19332=AXIS2_PLACEMENT_3D('',#51307,#22358,#22359);
#19333=AXIS2_PLACEMENT_3D('',#51560,#22360,#22361);
#19334=AXIS2_PLACEMENT_3D('',#51573,#22362,#22363);
#19335=AXIS2_PLACEMENT_3D('',#52132,#22364,#22365);
#19336=AXIS2_PLACEMENT_3D('',#52133,#22366,#22367);
#19337=AXIS2_PLACEMENT_3D('',#52382,#22368,#22369);
#19338=AXIS2_PLACEMENT_3D('',#52395,#22370,#22371);
#19339=AXIS2_PLACEMENT_3D('',#52984,#22372,#22373);
#19340=AXIS2_PLACEMENT_3D('',#52985,#22374,#22375);
#19341=AXIS2_PLACEMENT_3D('',#53239,#22376,#22377);
#19342=AXIS2_PLACEMENT_3D('',#53252,#22378,#22379);
#19343=AXIS2_PLACEMENT_3D('',#53806,#22380,#22381);
#19344=AXIS2_PLACEMENT_3D('',#53807,#22382,#22383);
#19345=AXIS2_PLACEMENT_3D('',#54056,#22384,#22385);
#19346=AXIS2_PLACEMENT_3D('',#54069,#22386,#22387);
#19347=AXIS2_PLACEMENT_3D('',#54658,#22388,#22389);
#19348=AXIS2_PLACEMENT_3D('',#54659,#22390,#22391);
#19349=AXIS2_PLACEMENT_3D('',#54908,#22392,#22393);
#19350=AXIS2_PLACEMENT_3D('',#54921,#22394,#22395);
#19351=AXIS2_PLACEMENT_3D('',#55475,#22396,#22397);
#19352=AXIS2_PLACEMENT_3D('',#55476,#22398,#22399);
#19353=AXIS2_PLACEMENT_3D('',#55725,#22400,#22401);
#19354=AXIS2_PLACEMENT_3D('',#55743,#22402,#22403);
#19355=AXIS2_PLACEMENT_3D('',#56253,#22404,#22405);
#19356=AXIS2_PLACEMENT_3D('',#56534,#22406,#22407);
#19357=AXIS2_PLACEMENT_3D('',#56535,#22408,#22409);
#19358=AXIS2_PLACEMENT_3D('',#56537,#22410,#22411);
#19359=AXIS2_PLACEMENT_3D('',#56827,#22412,#22413);
#19360=AXIS2_PLACEMENT_3D('',#56833,#22414,#22415);
#19361=AXIS2_PLACEMENT_3D('',#57369,#22416,#22417);
#19362=AXIS2_PLACEMENT_3D('',#57371,#22419,#22420);
#19363=AXIS2_PLACEMENT_3D('',#57372,#22421,#22422);
#19364=AXIS2_PLACEMENT_3D('',#57374,#22423,#22424);
#19365=AXIS2_PLACEMENT_3D('',#57376,#22426,#22427);
#19366=AXIS2_PLACEMENT_3D('',#57378,#22428,#22429);
#19367=AXIS2_PLACEMENT_3D('',#57380,#22431,#22432);
#19368=AXIS2_PLACEMENT_3D('',#57382,#22434,#22435);
#19369=AXIS2_PLACEMENT_3D('',#57383,#22436,#22437);
#19370=AXIS2_PLACEMENT_3D('',#57405,#22441,#22442);
#19371=AXIS2_PLACEMENT_3D('',#57449,#22445,#22446);
#19372=AXIS2_PLACEMENT_3D('',#57471,#22450,#22451);
#19373=AXIS2_PLACEMENT_3D('',#57515,#22454,#22455);
#19374=AXIS2_PLACEMENT_3D('',#57537,#22459,#22460);
#19375=AXIS2_PLACEMENT_3D('',#57581,#22463,#22464);
#19376=AXIS2_PLACEMENT_3D('',#57592,#22468,#22469);
#19377=AXIS2_PLACEMENT_3D('',#57611,#22472,#22473);
#19378=AXIS2_PLACEMENT_3D('',#57648,#22474,#22475);
#19379=AXIS2_PLACEMENT_3D('',#57657,#22476,#22477);
#19380=AXIS2_PLACEMENT_3D('',#57663,#22481,#22482);
#19381=AXIS2_PLACEMENT_3D('',#57667,#22485,#22486);
#19382=AXIS2_PLACEMENT_3D('',#57689,#22490,#22491);
#19383=AXIS2_PLACEMENT_3D('',#57768,#22494,#22495);
#19384=AXIS2_PLACEMENT_3D('',#57790,#22499,#22500);
#19385=AXIS2_PLACEMENT_3D('',#57863,#22503,#22504);
#19386=AXIS2_PLACEMENT_3D('',#57885,#22508,#22509);
#19387=AXIS2_PLACEMENT_3D('',#57923,#22512,#22513);
#19388=AXIS2_PLACEMENT_3D('',#57945,#22517,#22518);
#19389=AXIS2_PLACEMENT_3D('',#58010,#22521,#22522);
#19390=AXIS2_PLACEMENT_3D('',#58032,#22526,#22527);
#19391=AXIS2_PLACEMENT_3D('',#58105,#22530,#22531);
#19392=AXIS2_PLACEMENT_3D('',#58127,#22535,#22536);
#19393=AXIS2_PLACEMENT_3D('',#58200,#22539,#22540);
#19394=AXIS2_PLACEMENT_3D('',#58222,#22544,#22545);
#19395=AXIS2_PLACEMENT_3D('',#58908,#22548,#22549);
#19396=AXIS2_PLACEMENT_3D('',#58910,#22551,#22552);
#19397=AXIS2_PLACEMENT_3D('',#58912,#22554,#22555);
#19398=AXIS2_PLACEMENT_3D('',#58914,#22557,#22558);
#19399=AXIS2_PLACEMENT_3D('',#58916,#22560,#22561);
#19400=AXIS2_PLACEMENT_3D('',#58917,#22562,#22563);
#19401=AXIS2_PLACEMENT_3D('',#58918,#22564,#22565);
#19402=AXIS2_PLACEMENT_3D('',#58919,#22566,#22567);
#19403=AXIS2_PLACEMENT_3D('',#58920,#22568,#22569);
#19404=AXIS2_PLACEMENT_3D('',#58921,#22570,#22571);
#19405=AXIS2_PLACEMENT_3D('',#58922,#22572,#22573);
#19406=AXIS2_PLACEMENT_3D('',#58923,#22574,#22575);
#19407=AXIS2_PLACEMENT_3D('',#58924,#22576,#22577);
#19408=AXIS2_PLACEMENT_3D('',#58926,#22578,#22579);
#19409=AXIS2_PLACEMENT_3D('',#58927,#22580,#22581);
#19410=AXIS2_PLACEMENT_3D('',#58928,#22582,#22583);
#19411=AXIS2_PLACEMENT_3D('',#58929,#22584,#22585);
#19412=AXIS2_PLACEMENT_3D('',#58930,#22586,#22587);
#19413=AXIS2_PLACEMENT_3D('',#58931,#22588,#22589);
#19414=AXIS2_PLACEMENT_3D('',#58932,#22590,#22591);
#19415=AXIS2_PLACEMENT_3D('',#58933,#22592,#22593);
#19416=AXIS2_PLACEMENT_3D('',#58934,#22594,#22595);
#19417=AXIS2_PLACEMENT_3D('',#58935,#22596,#22597);
#19418=AXIS2_PLACEMENT_3D('',#58937,#22598,#22599);
#19419=AXIS2_PLACEMENT_3D('',#58939,#22601,#22602);
#19420=AXIS2_PLACEMENT_3D('',#58941,#22603,#22604);
#19421=AXIS2_PLACEMENT_3D('',#58944,#22606,#22607);
#19422=AXIS2_PLACEMENT_3D('',#58945,#22608,#22609);
#19423=AXIS2_PLACEMENT_3D('',#58947,#22611,#22612);
#19424=AXIS2_PLACEMENT_3D('',#58949,#22614,#22615);
#19425=AXIS2_PLACEMENT_3D('',#58951,#22617,#22618);
#19426=AXIS2_PLACEMENT_3D('',#58953,#22620,#22621);
#19427=AXIS2_PLACEMENT_3D('',#58955,#22623,#22624);
#19428=AXIS2_PLACEMENT_3D('',#58957,#22626,#22627);
#19429=AXIS2_PLACEMENT_3D('',#58959,#22629,#22630);
#19430=AXIS2_PLACEMENT_3D('',#58961,#22632,#22633);
#19431=AXIS2_PLACEMENT_3D('',#58963,#22635,#22636);
#19432=AXIS2_PLACEMENT_3D('',#58965,#22637,#22638);
#19433=AXIS2_PLACEMENT_3D('',#58966,#22639,#22640);
#19434=AXIS2_PLACEMENT_3D('',#58968,#22641,#22642);
#19435=AXIS2_PLACEMENT_3D('',#58970,#22644,#22645);
#19436=AXIS2_PLACEMENT_3D('',#58972,#22646,#22647);
#19437=AXIS2_PLACEMENT_3D('',#58974,#22649,#22650);
#19438=AXIS2_PLACEMENT_3D('',#58976,#22651,#22652);
#19439=AXIS2_PLACEMENT_3D('',#58978,#22654,#22655);
#19440=AXIS2_PLACEMENT_3D('',#58979,#22656,#22657);
#19441=AXIS2_PLACEMENT_3D('',#58980,#22658,#22659);
#19442=AXIS2_PLACEMENT_3D('',#58983,#22660,#22661);
#19443=AXIS2_PLACEMENT_3D('',#58984,#22662,#22663);
#19444=AXIS2_PLACEMENT_3D('',#58985,#22664,#22665);
#19445=AXIS2_PLACEMENT_3D('',#58989,#22667,#22668);
#19446=AXIS2_PLACEMENT_3D('',#58991,#22670,#22671);
#19447=AXIS2_PLACEMENT_3D('',#58992,#22672,#22673);
#19448=AXIS2_PLACEMENT_3D('',#58993,#22674,#22675);
#19449=AXIS2_PLACEMENT_3D('',#58996,#22676,#22677);
#19450=AXIS2_PLACEMENT_3D('',#58997,#22678,#22679);
#19451=AXIS2_PLACEMENT_3D('',#58998,#22680,#22681);
#19452=AXIS2_PLACEMENT_3D('',#59002,#22683,#22684);
#19453=AXIS2_PLACEMENT_3D('',#59004,#22686,#22687);
#19454=AXIS2_PLACEMENT_3D('',#59005,#22688,#22689);
#19455=AXIS2_PLACEMENT_3D('',#59006,#22690,#22691);
#19456=AXIS2_PLACEMENT_3D('',#59009,#22692,#22693);
#19457=AXIS2_PLACEMENT_3D('',#59010,#22694,#22695);
#19458=AXIS2_PLACEMENT_3D('',#59011,#22696,#22697);
#19459=AXIS2_PLACEMENT_3D('',#59015,#22699,#22700);
#19460=AXIS2_PLACEMENT_3D('',#59017,#22702,#22703);
#19461=AXIS2_PLACEMENT_3D('',#59018,#22704,#22705);
#19462=AXIS2_PLACEMENT_3D('',#59019,#22706,#22707);
#19463=AXIS2_PLACEMENT_3D('',#59022,#22708,#22709);
#19464=AXIS2_PLACEMENT_3D('',#59023,#22710,#22711);
#19465=AXIS2_PLACEMENT_3D('',#59024,#22712,#22713);
#19466=AXIS2_PLACEMENT_3D('',#59028,#22715,#22716);
#19467=AXIS2_PLACEMENT_3D('',#59030,#22718,#22719);
#19468=AXIS2_PLACEMENT_3D('',#59031,#22720,#22721);
#19469=AXIS2_PLACEMENT_3D('',#59032,#22722,#22723);
#19470=AXIS2_PLACEMENT_3D('',#59111,#22725,#22726);
#19471=AXIS2_PLACEMENT_3D('',#59190,#22728,#22729);
#19472=AXIS2_PLACEMENT_3D('',#59272,#22731,#22732);
#19473=AXIS2_PLACEMENT_3D('',#59351,#22734,#22735);
#19474=AXIS2_PLACEMENT_3D('',#59353,#22736,#22737);
#19475=AXIS2_PLACEMENT_3D('',#59357,#22740,#22741);
#19476=AXIS2_PLACEMENT_3D('',#59358,#22742,#22743);
#19477=AXIS2_PLACEMENT_3D('',#59360,#22744,#22745);
#19478=AXIS2_PLACEMENT_3D('',#59361,#22746,#22747);
#19479=AXIS2_PLACEMENT_3D('',#59363,#22748,#22749);
#19480=AXIS2_PLACEMENT_3D('',#59364,#22750,#22751);
#19481=AXIS2_PLACEMENT_3D('',#59366,#22752,#22753);
#19482=AXIS2_PLACEMENT_3D('',#59368,#22755,#22756);
#19483=AXIS2_PLACEMENT_3D('',#59370,#22757,#22758);
#19484=AXIS2_PLACEMENT_3D('',#59373,#22760,#22761);
#19485=AXIS2_PLACEMENT_3D('',#59374,#22762,#22763);
#19486=AXIS2_PLACEMENT_3D('',#59376,#22765,#22766);
#19487=AXIS2_PLACEMENT_3D('',#59378,#22767,#22768);
#19488=AXIS2_PLACEMENT_3D('',#59380,#22770,#22771);
#19489=AXIS2_PLACEMENT_3D('',#59382,#22772,#22773);
#19490=AXIS2_PLACEMENT_3D('',#59383,#22774,#22775);
#19491=AXIS2_PLACEMENT_3D('',#59386,#22777,#22778);
#19492=AXIS2_PLACEMENT_3D('',#59387,#22779,#22780);
#19493=AXIS2_PLACEMENT_3D('',#59391,#22783,#22784);
#19494=AXIS2_PLACEMENT_3D('',#59392,#22785,#22786);
#19495=AXIS2_PLACEMENT_3D('',#59395,#22788,#22789);
#19496=AXIS2_PLACEMENT_3D('',#59396,#22790,#22791);
#19497=AXIS2_PLACEMENT_3D('',#59397,#22792,#22793);
#19498=AXIS2_PLACEMENT_3D('',#59398,#22794,#22795);
#19499=AXIS2_PLACEMENT_3D('',#59400,#22796,#22797);
#19500=AXIS2_PLACEMENT_3D('',#59403,#22799,#22800);
#19501=AXIS2_PLACEMENT_3D('',#59404,#22801,#22802);
#19502=AXIS2_PLACEMENT_3D('',#59407,#22804,#22805);
#19503=AXIS2_PLACEMENT_3D('',#59408,#22806,#22807);
#19504=AXIS2_PLACEMENT_3D('',#59710,#22958,#22959);
#19505=AXIS2_PLACEMENT_3D('',#59711,#22960,#22961);
#19506=AXIS2_PLACEMENT_3D('',#59713,#22962,#22963);
#19507=AXIS2_PLACEMENT_3D('',#59715,#22965,#22966);
#19508=AXIS2_PLACEMENT_3D('',#60017,#23117,#23118);
#19509=AXIS2_PLACEMENT_3D('',#60018,#23119,#23120);
#19510=AXIS2_PLACEMENT_3D('',#60021,#23122,#23123);
#19511=AXIS2_PLACEMENT_3D('',#60022,#23124,#23125);
#19512=AXIS2_PLACEMENT_3D('',#60025,#23127,#23128);
#19513=AXIS2_PLACEMENT_3D('',#60026,#23129,#23130);
#19514=AXIS2_PLACEMENT_3D('',#60028,#23132,#23133);
#19515=AXIS2_PLACEMENT_3D('',#60031,#23136,#23137);
#19516=AXIS2_PLACEMENT_3D('',#60033,#23139,#23140);
#19517=AXIS2_PLACEMENT_3D('',#60035,#23142,#23143);
#19518=AXIS2_PLACEMENT_3D('',#60037,#23145,#23146);
#19519=AXIS2_PLACEMENT_3D('',#60039,#23148,#23149);
#19520=AXIS2_PLACEMENT_3D('',#60041,#23151,#23152);
#19521=AXIS2_PLACEMENT_3D('',#60043,#23154,#23155);
#19522=AXIS2_PLACEMENT_3D('',#60045,#23157,#23158);
#19523=AXIS2_PLACEMENT_3D('',#60047,#23160,#23161);
#19524=AXIS2_PLACEMENT_3D('',#60049,#23163,#23164);
#19525=AXIS2_PLACEMENT_3D('',#60051,#23166,#23167);
#19526=AXIS2_PLACEMENT_3D('',#60053,#23169,#23170);
#19527=AXIS2_PLACEMENT_3D('',#60055,#23172,#23173);
#19528=AXIS2_PLACEMENT_3D('',#60057,#23175,#23176);
#19529=AXIS2_PLACEMENT_3D('',#60059,#23178,#23179);
#19530=AXIS2_PLACEMENT_3D('',#60061,#23181,#23182);
#19531=AXIS2_PLACEMENT_3D('',#60063,#23184,#23185);
#19532=AXIS2_PLACEMENT_3D('',#60065,#23187,#23188);
#19533=AXIS2_PLACEMENT_3D('',#60067,#23190,#23191);
#19534=AXIS2_PLACEMENT_3D('',#60069,#23193,#23194);
#19535=AXIS2_PLACEMENT_3D('',#60071,#23196,#23197);
#19536=AXIS2_PLACEMENT_3D('',#60073,#23199,#23200);
#19537=AXIS2_PLACEMENT_3D('',#60075,#23202,#23203);
#19538=AXIS2_PLACEMENT_3D('',#60077,#23205,#23206);
#19539=AXIS2_PLACEMENT_3D('',#60079,#23208,#23209);
#19540=AXIS2_PLACEMENT_3D('',#60081,#23211,#23212);
#19541=AXIS2_PLACEMENT_3D('',#60083,#23214,#23215);
#19542=AXIS2_PLACEMENT_3D('',#60085,#23217,#23218);
#19543=AXIS2_PLACEMENT_3D('',#60087,#23220,#23221);
#19544=AXIS2_PLACEMENT_3D('',#60089,#23223,#23224);
#19545=AXIS2_PLACEMENT_3D('',#60091,#23226,#23227);
#19546=AXIS2_PLACEMENT_3D('',#60093,#23229,#23230);
#19547=AXIS2_PLACEMENT_3D('',#60095,#23232,#23233);
#19548=AXIS2_PLACEMENT_3D('',#60097,#23235,#23236);
#19549=AXIS2_PLACEMENT_3D('',#60099,#23238,#23239);
#19550=AXIS2_PLACEMENT_3D('',#60101,#23241,#23242);
#19551=AXIS2_PLACEMENT_3D('',#60103,#23244,#23245);
#19552=AXIS2_PLACEMENT_3D('',#60105,#23247,#23248);
#19553=AXIS2_PLACEMENT_3D('',#60107,#23250,#23251);
#19554=AXIS2_PLACEMENT_3D('',#60109,#23253,#23254);
#19555=AXIS2_PLACEMENT_3D('',#60111,#23256,#23257);
#19556=AXIS2_PLACEMENT_3D('',#60113,#23259,#23260);
#19557=AXIS2_PLACEMENT_3D('',#60115,#23262,#23263);
#19558=AXIS2_PLACEMENT_3D('',#60117,#23265,#23266);
#19559=AXIS2_PLACEMENT_3D('',#60119,#23268,#23269);
#19560=AXIS2_PLACEMENT_3D('',#60121,#23271,#23272);
#19561=AXIS2_PLACEMENT_3D('',#60123,#23274,#23275);
#19562=AXIS2_PLACEMENT_3D('',#60125,#23277,#23278);
#19563=AXIS2_PLACEMENT_3D('',#60127,#23280,#23281);
#19564=AXIS2_PLACEMENT_3D('',#60129,#23283,#23284);
#19565=AXIS2_PLACEMENT_3D('',#60131,#23286,#23287);
#19566=AXIS2_PLACEMENT_3D('',#60133,#23289,#23290);
#19567=AXIS2_PLACEMENT_3D('',#60135,#23292,#23293);
#19568=AXIS2_PLACEMENT_3D('',#60137,#23295,#23296);
#19569=AXIS2_PLACEMENT_3D('',#60139,#23298,#23299);
#19570=AXIS2_PLACEMENT_3D('',#60141,#23301,#23302);
#19571=AXIS2_PLACEMENT_3D('',#60143,#23304,#23305);
#19572=AXIS2_PLACEMENT_3D('',#60145,#23307,#23308);
#19573=AXIS2_PLACEMENT_3D('',#60147,#23310,#23311);
#19574=AXIS2_PLACEMENT_3D('',#60149,#23313,#23314);
#19575=AXIS2_PLACEMENT_3D('',#60151,#23316,#23317);
#19576=AXIS2_PLACEMENT_3D('',#60153,#23319,#23320);
#19577=AXIS2_PLACEMENT_3D('',#60155,#23322,#23323);
#19578=AXIS2_PLACEMENT_3D('',#60157,#23325,#23326);
#19579=AXIS2_PLACEMENT_3D('',#60159,#23328,#23329);
#19580=AXIS2_PLACEMENT_3D('',#60161,#23331,#23332);
#19581=AXIS2_PLACEMENT_3D('',#60163,#23334,#23335);
#19582=AXIS2_PLACEMENT_3D('',#60165,#23337,#23338);
#19583=AXIS2_PLACEMENT_3D('',#60167,#23340,#23341);
#19584=AXIS2_PLACEMENT_3D('',#60169,#23343,#23344);
#19585=AXIS2_PLACEMENT_3D('',#60171,#23346,#23347);
#19586=AXIS2_PLACEMENT_3D('',#60173,#23349,#23350);
#19587=AXIS2_PLACEMENT_3D('',#60175,#23352,#23353);
#19588=AXIS2_PLACEMENT_3D('',#60177,#23355,#23356);
#19589=AXIS2_PLACEMENT_3D('',#60179,#23358,#23359);
#19590=AXIS2_PLACEMENT_3D('',#60181,#23361,#23362);
#19591=AXIS2_PLACEMENT_3D('',#60183,#23364,#23365);
#19592=AXIS2_PLACEMENT_3D('',#60185,#23367,#23368);
#19593=AXIS2_PLACEMENT_3D('',#60187,#23370,#23371);
#19594=AXIS2_PLACEMENT_3D('',#60189,#23373,#23374);
#19595=AXIS2_PLACEMENT_3D('',#60191,#23376,#23377);
#19596=AXIS2_PLACEMENT_3D('',#60193,#23379,#23380);
#19597=AXIS2_PLACEMENT_3D('',#60195,#23382,#23383);
#19598=AXIS2_PLACEMENT_3D('',#60197,#23385,#23386);
#19599=AXIS2_PLACEMENT_3D('',#60199,#23388,#23389);
#19600=AXIS2_PLACEMENT_3D('',#60201,#23391,#23392);
#19601=AXIS2_PLACEMENT_3D('',#60203,#23394,#23395);
#19602=AXIS2_PLACEMENT_3D('',#60205,#23397,#23398);
#19603=AXIS2_PLACEMENT_3D('',#60207,#23400,#23401);
#19604=AXIS2_PLACEMENT_3D('',#60209,#23403,#23404);
#19605=AXIS2_PLACEMENT_3D('',#60211,#23406,#23407);
#19606=AXIS2_PLACEMENT_3D('',#60213,#23409,#23410);
#19607=AXIS2_PLACEMENT_3D('',#60215,#23412,#23413);
#19608=AXIS2_PLACEMENT_3D('',#60217,#23415,#23416);
#19609=AXIS2_PLACEMENT_3D('',#60219,#23418,#23419);
#19610=AXIS2_PLACEMENT_3D('',#60221,#23421,#23422);
#19611=AXIS2_PLACEMENT_3D('',#60223,#23424,#23425);
#19612=AXIS2_PLACEMENT_3D('',#60225,#23427,#23428);
#19613=AXIS2_PLACEMENT_3D('',#60227,#23430,#23431);
#19614=AXIS2_PLACEMENT_3D('',#60229,#23433,#23434);
#19615=AXIS2_PLACEMENT_3D('',#60231,#23436,#23437);
#19616=AXIS2_PLACEMENT_3D('',#60233,#23439,#23440);
#19617=AXIS2_PLACEMENT_3D('',#60235,#23442,#23443);
#19618=AXIS2_PLACEMENT_3D('',#60237,#23445,#23446);
#19619=AXIS2_PLACEMENT_3D('',#60239,#23448,#23449);
#19620=AXIS2_PLACEMENT_3D('',#60241,#23451,#23452);
#19621=AXIS2_PLACEMENT_3D('',#60243,#23454,#23455);
#19622=AXIS2_PLACEMENT_3D('',#60245,#23457,#23458);
#19623=AXIS2_PLACEMENT_3D('',#60247,#23460,#23461);
#19624=AXIS2_PLACEMENT_3D('',#60249,#23463,#23464);
#19625=AXIS2_PLACEMENT_3D('',#60251,#23466,#23467);
#19626=AXIS2_PLACEMENT_3D('',#60253,#23469,#23470);
#19627=AXIS2_PLACEMENT_3D('',#60255,#23472,#23473);
#19628=AXIS2_PLACEMENT_3D('',#60257,#23475,#23476);
#19629=AXIS2_PLACEMENT_3D('',#60259,#23478,#23479);
#19630=AXIS2_PLACEMENT_3D('',#60261,#23481,#23482);
#19631=AXIS2_PLACEMENT_3D('',#60263,#23484,#23485);
#19632=AXIS2_PLACEMENT_3D('',#60265,#23487,#23488);
#19633=AXIS2_PLACEMENT_3D('',#60267,#23490,#23491);
#19634=AXIS2_PLACEMENT_3D('',#60269,#23493,#23494);
#19635=AXIS2_PLACEMENT_3D('',#60271,#23496,#23497);
#19636=AXIS2_PLACEMENT_3D('',#60273,#23499,#23500);
#19637=AXIS2_PLACEMENT_3D('',#60275,#23502,#23503);
#19638=AXIS2_PLACEMENT_3D('',#60277,#23505,#23506);
#19639=AXIS2_PLACEMENT_3D('',#60279,#23508,#23509);
#19640=AXIS2_PLACEMENT_3D('',#60281,#23511,#23512);
#19641=AXIS2_PLACEMENT_3D('',#60283,#23514,#23515);
#19642=AXIS2_PLACEMENT_3D('',#60285,#23517,#23518);
#19643=AXIS2_PLACEMENT_3D('',#60287,#23520,#23521);
#19644=AXIS2_PLACEMENT_3D('',#60289,#23523,#23524);
#19645=AXIS2_PLACEMENT_3D('',#60291,#23526,#23527);
#19646=AXIS2_PLACEMENT_3D('',#60293,#23529,#23530);
#19647=AXIS2_PLACEMENT_3D('',#60295,#23532,#23533);
#19648=AXIS2_PLACEMENT_3D('',#60297,#23535,#23536);
#19649=AXIS2_PLACEMENT_3D('',#60299,#23538,#23539);
#19650=AXIS2_PLACEMENT_3D('',#60301,#23541,#23542);
#19651=AXIS2_PLACEMENT_3D('',#60303,#23544,#23545);
#19652=AXIS2_PLACEMENT_3D('',#60305,#23547,#23548);
#19653=AXIS2_PLACEMENT_3D('',#60307,#23550,#23551);
#19654=AXIS2_PLACEMENT_3D('',#60309,#23553,#23554);
#19655=AXIS2_PLACEMENT_3D('',#60311,#23556,#23557);
#19656=AXIS2_PLACEMENT_3D('',#60313,#23559,#23560);
#19657=AXIS2_PLACEMENT_3D('',#60315,#23562,#23563);
#19658=AXIS2_PLACEMENT_3D('',#60317,#23565,#23566);
#19659=AXIS2_PLACEMENT_3D('',#60319,#23568,#23569);
#19660=AXIS2_PLACEMENT_3D('',#60321,#23571,#23572);
#19661=AXIS2_PLACEMENT_3D('',#60323,#23574,#23575);
#19662=AXIS2_PLACEMENT_3D('',#60325,#23577,#23578);
#19663=AXIS2_PLACEMENT_3D('',#60327,#23580,#23581);
#19664=AXIS2_PLACEMENT_3D('',#60328,#23582,#23583);
#19665=AXIS2_PLACEMENT_3D('',#60329,#23584,#23585);
#19666=AXIS2_PLACEMENT_3D('',#60330,#23586,#23587);
#19667=AXIS2_PLACEMENT_3D('',#60331,#23588,#23589);
#19668=AXIS2_PLACEMENT_3D('',#60332,#23590,#23591);
#19669=AXIS2_PLACEMENT_3D('',#60333,#23592,#23593);
#19670=AXIS2_PLACEMENT_3D('',#60334,#23594,#23595);
#19671=AXIS2_PLACEMENT_3D('',#60335,#23596,#23597);
#19672=AXIS2_PLACEMENT_3D('',#60336,#23598,#23599);
#19673=AXIS2_PLACEMENT_3D('',#60337,#23600,#23601);
#19674=AXIS2_PLACEMENT_3D('',#60338,#23602,#23603);
#19675=AXIS2_PLACEMENT_3D('',#60339,#23604,#23605);
#19676=AXIS2_PLACEMENT_3D('',#60340,#23606,#23607);
#19677=AXIS2_PLACEMENT_3D('',#60341,#23608,#23609);
#19678=DIRECTION('axis',(0.,0.,1.));
#19679=DIRECTION('refdir',(1.,0.,0.));
#19680=DIRECTION('axis',(0.,0.,1.));
#19681=DIRECTION('refdir',(1.,0.,0.));
#19682=DIRECTION('center_axis',(1.,0.,0.));
#19683=DIRECTION('ref_axis',(0.,1.,0.));
#19684=DIRECTION('',(-1.,0.,0.));
#19685=DIRECTION('center_axis',(1.,0.,0.));
#19686=DIRECTION('ref_axis',(0.,1.,0.));
#19687=DIRECTION('center_axis',(1.,0.,0.));
#19688=DIRECTION('ref_axis',(0.,1.,0.));
#19689=DIRECTION('',(-1.,0.,0.));
#19690=DIRECTION('center_axis',(1.,0.,0.));
#19691=DIRECTION('ref_axis',(0.,1.,0.));
#19692=DIRECTION('',(-1.,0.,0.));
#19693=DIRECTION('center_axis',(1.,0.,0.));
#19694=DIRECTION('ref_axis',(0.,1.,0.));
#19695=DIRECTION('',(-1.,0.,0.));
#19696=DIRECTION('center_axis',(1.,0.,0.));
#19697=DIRECTION('ref_axis',(0.,1.,0.));
#19698=DIRECTION('',(-1.,0.,0.));
#19699=DIRECTION('center_axis',(1.,0.,0.));
#19700=DIRECTION('ref_axis',(0.,1.,0.));
#19701=DIRECTION('',(-1.,0.,0.));
#19702=DIRECTION('center_axis',(1.,0.,0.));
#19703=DIRECTION('ref_axis',(0.,1.,0.));
#19704=DIRECTION('',(-1.,0.,0.));
#19705=DIRECTION('center_axis',(1.,0.,0.));
#19706=DIRECTION('ref_axis',(0.,1.,0.));
#19707=DIRECTION('',(-1.,0.,0.));
#19708=DIRECTION('center_axis',(1.,0.,0.));
#19709=DIRECTION('ref_axis',(0.,1.,0.));
#19710=DIRECTION('',(-1.,0.,0.));
#19711=DIRECTION('center_axis',(1.,0.,0.));
#19712=DIRECTION('ref_axis',(0.,1.,0.));
#19713=DIRECTION('',(-1.,0.,0.));
#19714=DIRECTION('center_axis',(1.,0.,0.));
#19715=DIRECTION('ref_axis',(0.,1.,0.));
#19716=DIRECTION('',(-1.,0.,0.));
#19717=DIRECTION('center_axis',(1.,0.,0.));
#19718=DIRECTION('ref_axis',(0.,1.,0.));
#19719=DIRECTION('',(-1.,0.,0.));
#19720=DIRECTION('center_axis',(1.,0.,0.));
#19721=DIRECTION('ref_axis',(0.,1.,0.));
#19722=DIRECTION('',(-1.,0.,0.));
#19723=DIRECTION('center_axis',(1.,0.,0.));
#19724=DIRECTION('ref_axis',(0.,1.,0.));
#19725=DIRECTION('',(-1.,0.,0.));
#19726=DIRECTION('center_axis',(1.,0.,0.));
#19727=DIRECTION('ref_axis',(0.,1.,0.));
#19728=DIRECTION('',(-1.,0.,0.));
#19729=DIRECTION('center_axis',(1.,0.,0.));
#19730=DIRECTION('ref_axis',(0.,1.,0.));
#19731=DIRECTION('',(-1.,0.,0.));
#19732=DIRECTION('center_axis',(1.,0.,0.));
#19733=DIRECTION('ref_axis',(0.,0.,-1.));
#19734=DIRECTION('center_axis',(1.,0.,0.));
#19735=DIRECTION('ref_axis',(0.,0.,-1.));
#19736=DIRECTION('center_axis',(1.,0.,0.));
#19737=DIRECTION('ref_axis',(0.,0.,-1.));
#19738=DIRECTION('center_axis',(1.,0.,0.));
#19739=DIRECTION('ref_axis',(0.,0.,-1.));
#19740=DIRECTION('center_axis',(1.,0.,0.));
#19741=DIRECTION('ref_axis',(0.,0.,-1.));
#19742=DIRECTION('center_axis',(1.,0.,0.));
#19743=DIRECTION('ref_axis',(0.,0.,-1.));
#19744=DIRECTION('center_axis',(1.,0.,0.));
#19745=DIRECTION('ref_axis',(0.,0.,-1.));
#19746=DIRECTION('center_axis',(1.,0.,0.));
#19747=DIRECTION('ref_axis',(0.,0.,-1.));
#19748=DIRECTION('center_axis',(1.,0.,0.));
#19749=DIRECTION('ref_axis',(0.,0.,-1.));
#19750=DIRECTION('center_axis',(1.,0.,0.));
#19751=DIRECTION('ref_axis',(0.,0.,-1.));
#19752=DIRECTION('center_axis',(1.,0.,0.));
#19753=DIRECTION('ref_axis',(0.,0.,-1.));
#19754=DIRECTION('center_axis',(1.,0.,0.));
#19755=DIRECTION('ref_axis',(0.,0.,-1.));
#19756=DIRECTION('center_axis',(1.,0.,0.));
#19757=DIRECTION('ref_axis',(0.,0.,-1.));
#19758=DIRECTION('center_axis',(1.,0.,0.));
#19759=DIRECTION('ref_axis',(0.,0.,-1.));
#19760=DIRECTION('center_axis',(1.,0.,0.));
#19761=DIRECTION('ref_axis',(0.,0.,-1.));
#19762=DIRECTION('center_axis',(1.,0.,0.));
#19763=DIRECTION('ref_axis',(0.,0.,-1.));
#19764=DIRECTION('center_axis',(1.,0.,0.));
#19765=DIRECTION('ref_axis',(0.,0.,-1.));
#19766=DIRECTION('center_axis',(1.,0.,0.));
#19767=DIRECTION('ref_axis',(0.,0.,-1.));
#19768=DIRECTION('center_axis',(1.,0.,0.));
#19769=DIRECTION('ref_axis',(0.,0.,-1.));
#19770=DIRECTION('center_axis',(1.,0.,0.));
#19771=DIRECTION('ref_axis',(0.,0.,-1.));
#19772=DIRECTION('center_axis',(1.,0.,0.));
#19773=DIRECTION('ref_axis',(0.,0.,-1.));
#19774=DIRECTION('center_axis',(1.,0.,0.));
#19775=DIRECTION('ref_axis',(0.,0.,-1.));
#19776=DIRECTION('center_axis',(1.,0.,0.));
#19777=DIRECTION('ref_axis',(0.,0.,-1.));
#19778=DIRECTION('center_axis',(1.,0.,0.));
#19779=DIRECTION('ref_axis',(0.,-0.201120720209613,-0.9795664632389));
#19780=DIRECTION('',(1.,0.,0.));
#19781=DIRECTION('center_axis',(1.,0.,0.));
#19782=DIRECTION('ref_axis',(0.,1.,1.0886778522233E-13));
#19783=DIRECTION('center_axis',(1.,0.,0.));
#19784=DIRECTION('ref_axis',(0.,1.,1.0886778522233E-13));
#19785=DIRECTION('',(1.,0.,0.));
#19786=DIRECTION('center_axis',(1.,0.,0.));
#19787=DIRECTION('ref_axis',(0.,1.,1.0886778522233E-13));
#19788=DIRECTION('',(1.,0.,0.));
#19789=DIRECTION('center_axis',(1.,0.,0.));
#19790=DIRECTION('ref_axis',(0.,1.,1.0886778522233E-13));
#19791=DIRECTION('',(1.,0.,0.));
#19792=DIRECTION('center_axis',(1.,0.,0.));
#19793=DIRECTION('ref_axis',(0.,1.,1.0886778522233E-13));
#19794=DIRECTION('',(1.,0.,0.));
#19795=DIRECTION('center_axis',(1.,0.,0.));
#19796=DIRECTION('ref_axis',(0.,1.,1.0886778522233E-13));
#19797=DIRECTION('',(1.,0.,0.));
#19798=DIRECTION('center_axis',(1.,0.,0.));
#19799=DIRECTION('ref_axis',(0.,1.,1.0886778522233E-13));
#19800=DIRECTION('',(1.,0.,0.));
#19801=DIRECTION('center_axis',(1.,0.,0.));
#19802=DIRECTION('ref_axis',(0.,1.,1.0886778522233E-13));
#19803=DIRECTION('',(1.,0.,0.));
#19804=DIRECTION('center_axis',(1.,0.,0.));
#19805=DIRECTION('ref_axis',(0.,1.,1.0886778522233E-13));
#19806=DIRECTION('',(1.,0.,0.));
#19807=DIRECTION('center_axis',(1.,0.,0.));
#19808=DIRECTION('ref_axis',(0.,1.,1.0886778522233E-13));
#19809=DIRECTION('',(1.,0.,0.));
#19810=DIRECTION('center_axis',(1.,0.,0.));
#19811=DIRECTION('ref_axis',(0.,1.,1.0886778522233E-13));
#19812=DIRECTION('',(1.,0.,0.));
#19813=DIRECTION('center_axis',(1.,0.,0.));
#19814=DIRECTION('ref_axis',(0.,1.,1.0886778522233E-13));
#19815=DIRECTION('',(1.,0.,0.));
#19816=DIRECTION('center_axis',(1.,0.,0.));
#19817=DIRECTION('ref_axis',(0.,1.,1.0886778522233E-13));
#19818=DIRECTION('',(1.,0.,0.));
#19819=DIRECTION('center_axis',(1.,0.,0.));
#19820=DIRECTION('ref_axis',(0.,1.,1.0886778522233E-13));
#19821=DIRECTION('',(1.,0.,0.));
#19822=DIRECTION('center_axis',(1.,0.,0.));
#19823=DIRECTION('ref_axis',(0.,1.,1.0886778522233E-13));
#19824=DIRECTION('',(1.,0.,0.));
#19825=DIRECTION('center_axis',(1.,0.,0.));
#19826=DIRECTION('ref_axis',(0.,1.,1.0886778522233E-13));
#19827=DIRECTION('',(1.,0.,0.));
#19828=DIRECTION('center_axis',(-1.,0.,-1.46491071877532E-15));
#19829=DIRECTION('ref_axis',(0.,-1.,-3.17896142702966E-17));
#19830=DIRECTION('center_axis',(-1.,0.,0.));
#19831=DIRECTION('ref_axis',(0.,-1.,0.));
#19832=DIRECTION('',(-0.492698814983593,0.870199906753479,-5.87527702781227E-16));
#19833=DIRECTION('center_axis',(1.,0.,0.));
#19834=DIRECTION('ref_axis',(0.,-1.,-6.12323399573676E-17));
#19835=DIRECTION('center_axis',(1.,0.,0.));
#19836=DIRECTION('ref_axis',(0.,-1.,-6.12323399573676E-17));
#19837=DIRECTION('center_axis',(-1.,0.,0.));
#19838=DIRECTION('ref_axis',(0.,1.,0.));
#19839=DIRECTION('',(-0.857492925712545,-0.514495755427525,-6.30075580059218E-17));
#19840=DIRECTION('center_axis',(1.,0.,0.));
#19841=DIRECTION('ref_axis',(0.,0.,-1.));
#19842=DIRECTION('center_axis',(1.,0.,0.));
#19843=DIRECTION('ref_axis',(0.,0.,-1.));
#19844=DIRECTION('center_axis',(1.,0.,0.));
#19845=DIRECTION('ref_axis',(0.,0.,-1.));
#19846=DIRECTION('center_axis',(0.,0.866025403784439,0.499999999999999));
#19847=DIRECTION('ref_axis',(0.,-0.499999999999999,0.866025403784439));
#19848=DIRECTION('',(0.463876645871912,-0.442949900500785,0.767211732874941));
#19849=DIRECTION('',(1.,0.,0.));
#19850=DIRECTION('',(0.,-0.499999999999999,0.866025403784439));
#19851=DIRECTION('',(-1.,0.,0.));
#19852=DIRECTION('',(-0.463876645871911,-0.442949900500785,0.767211732874941));
#19853=DIRECTION('center_axis',(0.,0.475999928342023,0.879445318492508));
#19854=DIRECTION('ref_axis',(0.,-0.879445318492508,0.475999928342023));
#19855=DIRECTION('',(0.,0.879445318492508,-0.475999928342023));
#19856=DIRECTION('',(1.,0.,0.));
#19857=DIRECTION('',(0.,-0.879445318492508,0.475999928342023));
#19858=DIRECTION('center_axis',(-0.707106781186547,0.336582777174955,0.621861748388816));
#19859=DIRECTION('ref_axis',(0.660393123266679,0.,0.750920050832364));
#19860=DIRECTION('',(0.648510052987376,0.659223811296842,0.380603044908442));
#19861=DIRECTION('',(0.,-0.879445318492508,0.475999928342023));
#19862=DIRECTION('',(0.691947206789735,0.510494399095566,0.510494399095564));
#19863=DIRECTION('center_axis',(-0.707106781186547,0.706839460333999,-0.01944163868458));
#19864=DIRECTION('ref_axis',(-0.0274842426448097,0.,0.999622236850622));
#19865=DIRECTION('',(0.,-0.0274946291024904,-0.99962195122482));
#19866=DIRECTION('',(0.691947206789734,0.697348317654214,0.18685391855865));
#19867=DIRECTION('',(0.,0.0274946291024904,0.99962195122482));
#19868=DIRECTION('center_axis',(0.,0.500000000000001,0.866025403784438));
#19869=DIRECTION('ref_axis',(1.,0.,0.));
#19870=DIRECTION('',(0.463876645871911,-0.76721173287494,0.442949900500787));
#19871=DIRECTION('',(1.,0.,0.));
#19872=DIRECTION('',(0.,-0.866025403784438,0.500000000000001));
#19873=DIRECTION('',(-1.,0.,0.));
#19874=DIRECTION('',(-0.463876645871911,-0.76721173287494,0.442949900500787));
#19875=DIRECTION('center_axis',(0.,-0.0274946291024896,0.99962195122482));
#19876=DIRECTION('ref_axis',(0.,-0.99962195122482,-0.0274946291024896));
#19877=DIRECTION('',(0.,0.99962195122482,0.0274946291024896));
#19878=DIRECTION('',(1.,0.,0.));
#19879=DIRECTION('',(0.,-0.99962195122482,-0.0274946291024896));
#19880=DIRECTION('center_axis',(-0.707106781186548,-0.0194416386845794,
0.706839460333999));
#19881=DIRECTION('ref_axis',(0.706973082855489,0.,0.707240454242973));
#19882=DIRECTION('',(0.648510052987376,0.380603044908442,0.659223811296841));
#19883=DIRECTION('',(0.,-0.99962195122482,-0.0274946291024896));
#19884=DIRECTION('',(0.691947206789734,0.186853918558649,0.697348317654214));
#19885=DIRECTION('center_axis',(-0.707106781186547,0.621861748388816,0.336582777174955));
#19886=DIRECTION('ref_axis',(0.429793326728032,0.,0.902927292920117));
#19887=DIRECTION('',(0.,0.475999928342023,-0.879445318492508));
#19888=DIRECTION('',(0.,-0.475999928342023,0.879445318492508));
#19889=DIRECTION('center_axis',(0.,2.60630817828214E-15,1.));
#19890=DIRECTION('ref_axis',(1.,0.,0.));
#19891=DIRECTION('',(0.463876645871913,-0.885899801001572,2.30892789648892E-15));
#19892=DIRECTION('',(1.,0.,0.));
#19893=DIRECTION('',(0.,-1.,2.60630817828214E-15));
#19894=DIRECTION('',(-1.,0.,0.));
#19895=DIRECTION('',(-0.463876645871909,-0.885899801001573,2.30892789648892E-15));
#19896=DIRECTION('center_axis',(0.,-0.523622022882797,0.851950689390019));
#19897=DIRECTION('ref_axis',(0.,-0.851950689390018,-0.523622022882797));
#19898=DIRECTION('',(0.,0.851950689390018,0.523622022882797));
#19899=DIRECTION('',(1.,0.,0.));
#19900=DIRECTION('',(0.,-0.851950689390018,-0.523622022882797));
#19901=DIRECTION('center_axis',(-0.707106781186547,-0.370256683159044,0.602420109704237));
#19902=DIRECTION('ref_axis',(0.648510052987376,0.,0.761206089816884));
#19903=DIRECTION('',(0.648510052987376,3.84997679969453E-16,0.761206089816884));
#19904=DIRECTION('',(0.,-0.851950689390018,-0.523622022882797));
#19905=DIRECTION('',(0.691947206789735,-0.186853918558647,0.697348317654214));
#19906=DIRECTION('center_axis',(-0.707106781186548,0.370256683159043,0.602420109704236));
#19907=DIRECTION('ref_axis',(0.648510052987375,0.,0.761206089816885));
#19908=DIRECTION('',(0.,0.851950689390018,-0.523622022882797));
#19909=DIRECTION('',(0.,-0.851950689390018,0.523622022882797));
#19910=DIRECTION('center_axis',(0.,-0.5,0.866025403784439));
#19911=DIRECTION('ref_axis',(1.,0.,0.));
#19912=DIRECTION('',(0.463876645871911,-0.767211732874941,-0.442949900500786));
#19913=DIRECTION('',(1.,0.,0.));
#19914=DIRECTION('',(0.,-0.866025403784439,-0.5));
#19915=DIRECTION('',(-1.,0.,0.));
#19916=DIRECTION('',(-0.463876645871911,-0.767211732874941,-0.442949900500786));
#19917=DIRECTION('center_axis',(0.,-0.879445318492508,0.475999928342023));
#19918=DIRECTION('ref_axis',(0.,-0.475999928342023,-0.879445318492508));
#19919=DIRECTION('',(0.,0.475999928342023,0.879445318492508));
#19920=DIRECTION('',(1.,0.,0.));
#19921=DIRECTION('',(0.,-0.475999928342023,-0.879445318492508));
#19922=DIRECTION('center_axis',(-0.707106781186547,-0.621861748388816,0.336582777174955));
#19923=DIRECTION('ref_axis',(0.429793326728033,0.,0.902927292920117));
#19924=DIRECTION('',(0.648510052987375,-0.380603044908443,0.659223811296841));
#19925=DIRECTION('',(0.,-0.475999928342023,-0.879445318492508));
#19926=DIRECTION('',(0.691947206789734,-0.510494399095567,0.510494399095564));
#19927=DIRECTION('center_axis',(-0.707106781186547,0.01944163868458,0.706839460333999));
#19928=DIRECTION('ref_axis',(0.706973082855489,0.,0.707240454242973));
#19929=DIRECTION('',(0.,0.99962195122482,-0.0274946291024905));
#19930=DIRECTION('',(0.,-0.99962195122482,0.0274946291024905));
#19931=DIRECTION('center_axis',(0.,-0.866025403784438,0.500000000000001));
#19932=DIRECTION('ref_axis',(1.,0.,0.));
#19933=DIRECTION('',(0.463876645871912,-0.442949900500786,-0.76721173287494));
#19934=DIRECTION('',(1.,0.,0.));
#19935=DIRECTION('',(0.,-0.500000000000001,-0.866025403784438));
#19936=DIRECTION('',(-1.,0.,0.));
#19937=DIRECTION('',(-0.463876645871911,-0.442949900500787,-0.76721173287494));
#19938=DIRECTION('center_axis',(0.,-0.99962195122482,-0.0274946291024905));
#19939=DIRECTION('ref_axis',(0.,0.0274946291024905,-0.99962195122482));
#19940=DIRECTION('',(0.,-0.0274946291024905,0.99962195122482));
#19941=DIRECTION('',(1.,0.,0.));
#19942=DIRECTION('',(0.,0.0274946291024905,-0.99962195122482));
#19943=DIRECTION('center_axis',(-0.707106781186547,-0.706839460333999,-0.01944163868458));
#19944=DIRECTION('ref_axis',(-0.0274842426448098,0.,0.999622236850622));
#19945=DIRECTION('',(0.648510052987376,-0.659223811296841,0.380603044908442));
#19946=DIRECTION('',(0.,0.0274946291024905,-0.99962195122482));
#19947=DIRECTION('',(0.691947206789735,-0.697348317654213,0.18685391855865));
#19948=DIRECTION('center_axis',(-0.707106781186547,-0.336582777174955,0.621861748388816));
#19949=DIRECTION('ref_axis',(0.660393123266679,0.,0.750920050832364));
#19950=DIRECTION('',(0.,0.879445318492508,0.475999928342023));
#19951=DIRECTION('',(0.,-0.879445318492508,-0.475999928342023));
#19952=DIRECTION('center_axis',(0.,1.,-2.60630817828214E-15));
#19953=DIRECTION('ref_axis',(0.,2.60630817828214E-15,1.));
#19954=DIRECTION('',(0.463876645871912,2.30892789648892E-15,0.885899801001572));
#19955=DIRECTION('',(1.,0.,0.));
#19956=DIRECTION('',(0.,2.60630817828214E-15,1.));
#19957=DIRECTION('',(-1.,0.,0.));
#19958=DIRECTION('',(-0.46387664587191,2.30892789648892E-15,0.885899801001573));
#19959=DIRECTION('center_axis',(0.,0.851950689390018,0.523622022882797));
#19960=DIRECTION('ref_axis',(0.,-0.523622022882797,0.851950689390018));
#19961=DIRECTION('',(0.,0.523622022882797,-0.851950689390018));
#19962=DIRECTION('',(1.,0.,0.));
#19963=DIRECTION('',(0.,-0.523622022882797,0.851950689390018));
#19964=DIRECTION('center_axis',(-0.707106781186548,0.602420109704236,0.370256683159043));
#19965=DIRECTION('ref_axis',(0.463876645871911,0.,0.885899801001573));
#19966=DIRECTION('',(0.648510052987376,0.761206089816885,1.19998465421244E-15));
#19967=DIRECTION('',(0.,-0.523622022882797,0.851950689390018));
#19968=DIRECTION('center_axis',(-0.707106781186547,0.602420109704236,-0.370256683159044));
#19969=DIRECTION('ref_axis',(-0.463876645871911,0.,0.885899801001572));
#19970=DIRECTION('',(0.,-0.523622022882797,-0.851950689390018));
#19971=DIRECTION('',(-0.691947206789734,-0.697348317654214,0.186853918558648));
#19972=DIRECTION('',(0.,0.523622022882797,0.851950689390018));
#19973=DIRECTION('center_axis',(0.,0.866025403784438,-0.500000000000001));
#19974=DIRECTION('ref_axis',(-1.,0.,0.));
#19975=DIRECTION('',(0.463876645871911,0.442949900500787,0.76721173287494));
#19976=DIRECTION('',(1.,0.,0.));
#19977=DIRECTION('',(0.,0.500000000000001,0.866025403784438));
#19978=DIRECTION('',(-1.,0.,0.));
#19979=DIRECTION('',(-0.46387664587191,0.442949900500787,0.76721173287494));
#19980=DIRECTION('center_axis',(0.,0.99962195122482,0.0274946291024892));
#19981=DIRECTION('ref_axis',(0.,-0.0274946291024892,0.99962195122482));
#19982=DIRECTION('',(0.,0.0274946291024892,-0.99962195122482));
#19983=DIRECTION('',(1.,0.,0.));
#19984=DIRECTION('',(0.,-0.0274946291024892,0.99962195122482));
#19985=DIRECTION('center_axis',(-0.707106781186548,0.706839460333999,0.0194416386845791));
#19986=DIRECTION('ref_axis',(0.0274842426448084,0.,0.999622236850622));
#19987=DIRECTION('',(0.648510052987375,0.659223811296841,-0.380603044908443));
#19988=DIRECTION('',(0.,-0.0274946291024892,0.99962195122482));
#19989=DIRECTION('center_axis',(0.,0.5,-0.866025403784439));
#19990=DIRECTION('ref_axis',(-1.,0.,0.));
#19991=DIRECTION('',(0.463876645871911,0.76721173287494,0.442949900500786));
#19992=DIRECTION('',(1.,0.,0.));
#19993=DIRECTION('',(0.,0.866025403784439,0.5));
#19994=DIRECTION('',(-1.,0.,0.));
#19995=DIRECTION('',(-0.46387664587191,0.767211732874941,0.442949900500786));
#19996=DIRECTION('center_axis',(0.,0.879445318492508,-0.475999928342023));
#19997=DIRECTION('ref_axis',(0.,0.475999928342023,0.879445318492508));
#19998=DIRECTION('',(0.,-0.475999928342023,-0.879445318492508));
#19999=DIRECTION('',(1.,0.,0.));
#20000=DIRECTION('',(0.,0.475999928342023,0.879445318492508));
#20001=DIRECTION('center_axis',(-0.707106781186547,0.621861748388816,-0.336582777174955));
#20002=DIRECTION('ref_axis',(-0.429793326728032,0.,0.902927292920117));
#20003=DIRECTION('',(0.648510052987376,0.380603044908442,-0.659223811296841));
#20004=DIRECTION('',(0.,0.475999928342023,0.879445318492508));
#20005=DIRECTION('',(0.691947206789734,0.510494399095564,-0.510494399095566));
#20006=DIRECTION('center_axis',(-0.707106781186548,-0.0194416386845788,
-0.706839460333999));
#20007=DIRECTION('ref_axis',(-0.706973082855489,0.,0.707240454242973));
#20008=DIRECTION('',(0.,-0.99962195122482,0.0274946291024888));
#20009=DIRECTION('',(0.691947206789735,0.186853918558646,-0.697348317654214));
#20010=DIRECTION('',(0.,0.99962195122482,-0.0274946291024888));
#20011=DIRECTION('center_axis',(0.,-2.60630817828214E-15,-1.));
#20012=DIRECTION('ref_axis',(-1.,0.,0.));
#20013=DIRECTION('',(0.463876645871913,0.885899801001571,-2.30892789648892E-15));
#20014=DIRECTION('',(1.,0.,0.));
#20015=DIRECTION('',(0.,1.,-2.60630817828214E-15));
#20016=DIRECTION('',(-1.,0.,0.));
#20017=DIRECTION('',(-0.46387664587191,0.885899801001573,-2.30892789648892E-15));
#20018=DIRECTION('center_axis',(0.,0.523622022882797,-0.851950689390019));
#20019=DIRECTION('ref_axis',(0.,0.851950689390018,0.523622022882797));
#20020=DIRECTION('',(0.,-0.851950689390018,-0.523622022882797));
#20021=DIRECTION('',(1.,0.,0.));
#20022=DIRECTION('',(0.,0.851950689390018,0.523622022882797));
#20023=DIRECTION('center_axis',(-0.707106781186547,0.370256683159044,-0.602420109704237));
#20024=DIRECTION('ref_axis',(-0.648510052987376,0.,0.761206089816884));
#20025=DIRECTION('',(0.648510052987376,-2.3549776941208E-15,-0.761206089816885));
#20026=DIRECTION('',(0.,0.851950689390018,0.523622022882797));
#20027=DIRECTION('center_axis',(-0.707106781186548,-0.370256683159044,-0.602420109704236));
#20028=DIRECTION('ref_axis',(-0.648510052987375,0.,0.761206089816885));
#20029=DIRECTION('',(0.,-0.851950689390018,0.523622022882798));
#20030=DIRECTION('',(0.691947206789734,-0.186853918558651,-0.697348317654214));
#20031=DIRECTION('',(0.,0.851950689390018,-0.523622022882798));
#20032=DIRECTION('center_axis',(0.,-0.500000000000001,-0.866025403784438));
#20033=DIRECTION('ref_axis',(-1.,0.,0.));
#20034=DIRECTION('',(0.463876645871911,0.76721173287494,-0.442949900500787));
#20035=DIRECTION('',(1.,0.,0.));
#20036=DIRECTION('',(0.,0.866025403784438,-0.500000000000001));
#20037=DIRECTION('',(-1.,0.,0.));
#20038=DIRECTION('',(-0.46387664587191,0.767211732874941,-0.442949900500787));
#20039=DIRECTION('center_axis',(0.,0.0274946291024892,-0.99962195122482));
#20040=DIRECTION('ref_axis',(0.,0.99962195122482,0.0274946291024892));
#20041=DIRECTION('',(0.,-0.99962195122482,-0.0274946291024892));
#20042=DIRECTION('',(1.,0.,0.));
#20043=DIRECTION('',(0.,0.99962195122482,0.0274946291024892));
#20044=DIRECTION('center_axis',(-0.707106781186548,0.0194416386845791,-0.706839460333999));
#20045=DIRECTION('ref_axis',(-0.706973082855489,0.,0.707240454242973));
#20046=DIRECTION('',(0.648510052987375,-0.380603044908443,-0.659223811296841));
#20047=DIRECTION('',(0.,0.99962195122482,0.0274946291024892));
#20048=DIRECTION('center_axis',(-0.707106781186548,-0.621861748388815,-0.336582777174955));
#20049=DIRECTION('ref_axis',(-0.429793326728032,0.,0.902927292920117));
#20050=DIRECTION('',(0.,-0.475999928342023,0.879445318492508));
#20051=DIRECTION('',(0.691947206789734,-0.510494399095568,-0.510494399095563));
#20052=DIRECTION('',(0.,0.475999928342023,-0.879445318492508));
#20053=DIRECTION('center_axis',(0.,-0.866025403784438,-0.5));
#20054=DIRECTION('ref_axis',(-1.,0.,0.));
#20055=DIRECTION('',(0.463876645871911,0.442949900500787,-0.76721173287494));
#20056=DIRECTION('',(1.,0.,0.));
#20057=DIRECTION('',(0.,0.5,-0.866025403784438));
#20058=DIRECTION('',(-1.,0.,0.));
#20059=DIRECTION('',(-0.463876645871912,0.442949900500786,-0.76721173287494));
#20060=DIRECTION('center_axis',(0.,-0.475999928342023,-0.879445318492508));
#20061=DIRECTION('ref_axis',(0.,0.879445318492508,-0.475999928342023));
#20062=DIRECTION('',(0.,-0.879445318492508,0.475999928342023));
#20063=DIRECTION('',(1.,0.,0.));
#20064=DIRECTION('',(0.,0.879445318492508,-0.475999928342023));
#20065=DIRECTION('center_axis',(-0.707106781186547,-0.336582777174955,-0.621861748388816));
#20066=DIRECTION('ref_axis',(-0.660393123266679,0.,0.750920050832364));
#20067=DIRECTION('',(0.648510052987376,-0.659223811296841,-0.380603044908442));
#20068=DIRECTION('',(0.,0.879445318492508,-0.475999928342023));
#20069=DIRECTION('center_axis',(-0.707106781186547,-0.706839460333999,0.0194416386845794));
#20070=DIRECTION('ref_axis',(0.027484242644809,0.,0.999622236850622));
#20071=DIRECTION('',(0.,0.0274946291024896,0.99962195122482));
#20072=DIRECTION('',(0.691947206789735,-0.697348317654213,-0.18685391855865));
#20073=DIRECTION('',(0.,-0.0274946291024896,-0.99962195122482));
#20074=DIRECTION('center_axis',(0.,-1.,0.));
#20075=DIRECTION('ref_axis',(0.,0.,-1.));
#20076=DIRECTION('',(0.463876645871911,0.,-0.885899801001572));
#20077=DIRECTION('',(1.,0.,0.));
#20078=DIRECTION('',(0.,0.,-1.));
#20079=DIRECTION('',(-1.,0.,0.));
#20080=DIRECTION('',(-0.463876645871911,0.,-0.885899801001572));
#20081=DIRECTION('center_axis',(0.,-0.851950689390019,-0.523622022882797));
#20082=DIRECTION('ref_axis',(0.,0.523622022882797,-0.851950689390018));
#20083=DIRECTION('',(0.,-0.523622022882797,0.851950689390018));
#20084=DIRECTION('',(1.,0.,0.));
#20085=DIRECTION('',(0.,0.523622022882797,-0.851950689390018));
#20086=DIRECTION('center_axis',(-0.707106781186547,-0.602420109704237,-0.370256683159044));
#20087=DIRECTION('ref_axis',(-0.463876645871911,0.,0.885899801001572));
#20088=DIRECTION('',(0.648510052987376,-0.761206089816884,-4.29989294273536E-16));
#20089=DIRECTION('',(0.,0.523622022882797,-0.851950689390018));
#20090=DIRECTION('center_axis',(-0.707106781186547,-0.602420109704237,0.370256683159044));
#20091=DIRECTION('ref_axis',(0.463876645871911,0.,0.885899801001572));
#20092=DIRECTION('',(0.,0.523622022882797,0.851950689390018));
#20093=DIRECTION('',(0.,-0.523622022882797,-0.851950689390018));
#20094=DIRECTION('center_axis',(-1.,0.,0.));
#20095=DIRECTION('ref_axis',(0.,1.,0.));
#20096=DIRECTION('center_axis',(-1.,0.,0.));
#20097=DIRECTION('ref_axis',(0.,1.,0.));
#20098=DIRECTION('center_axis',(1.,0.,0.));
#20099=DIRECTION('ref_axis',(0.,1.,0.));
#20100=DIRECTION('center_axis',(1.,0.,0.));
#20101=DIRECTION('ref_axis',(0.,1.,0.));
#20102=DIRECTION('center_axis',(1.,0.,0.));
#20103=DIRECTION('ref_axis',(0.,0.,-1.));
#20104=DIRECTION('center_axis',(-1.,0.,0.));
#20105=DIRECTION('ref_axis',(0.,0.866025403784439,0.5));
#20106=DIRECTION('center_axis',(-1.,0.,0.));
#20107=DIRECTION('ref_axis',(0.,0.866025403784439,0.5));
#20108=DIRECTION('center_axis',(1.,0.,0.));
#20109=DIRECTION('ref_axis',(0.,0.866025403784439,0.5));
#20110=DIRECTION('center_axis',(1.,0.,0.));
#20111=DIRECTION('ref_axis',(0.,0.866025403784439,0.5));
#20112=DIRECTION('center_axis',(1.,0.,0.));
#20113=DIRECTION('ref_axis',(0.,0.5,-0.866025403784439));
#20114=DIRECTION('center_axis',(-1.,0.,0.));
#20115=DIRECTION('ref_axis',(0.,0.5,0.866025403784438));
#20116=DIRECTION('center_axis',(-1.,0.,0.));
#20117=DIRECTION('ref_axis',(0.,0.5,0.866025403784439));
#20118=DIRECTION('center_axis',(1.,0.,0.));
#20119=DIRECTION('ref_axis',(0.,0.5,0.866025403784439));
#20120=DIRECTION('center_axis',(1.,0.,0.));
#20121=DIRECTION('ref_axis',(0.,0.5,0.866025403784439));
#20122=DIRECTION('center_axis',(1.,0.,0.));
#20123=DIRECTION('ref_axis',(0.,0.866025403784439,-0.5));
#20124=DIRECTION('center_axis',(-1.,0.,0.));
#20125=DIRECTION('ref_axis',(0.,6.12323399573677E-17,1.));
#20126=DIRECTION('center_axis',(-1.,0.,0.));
#20127=DIRECTION('ref_axis',(0.,6.12323399573677E-17,1.));
#20128=DIRECTION('center_axis',(1.,0.,0.));
#20129=DIRECTION('ref_axis',(0.,6.12323399573677E-17,1.));
#20130=DIRECTION('center_axis',(1.,0.,0.));
#20131=DIRECTION('ref_axis',(0.,6.12323399573677E-17,1.));
#20132=DIRECTION('center_axis',(1.,0.,0.));
#20133=DIRECTION('ref_axis',(0.,1.,-6.12323399573677E-17));
#20134=DIRECTION('center_axis',(-1.,0.,0.));
#20135=DIRECTION('ref_axis',(0.,-0.5,0.866025403784439));
#20136=DIRECTION('center_axis',(-1.,0.,0.));
#20137=DIRECTION('ref_axis',(0.,-0.5,0.866025403784439));
#20138=DIRECTION('center_axis',(1.,0.,0.));
#20139=DIRECTION('ref_axis',(0.,-0.5,0.866025403784439));
#20140=DIRECTION('center_axis',(1.,0.,0.));
#20141=DIRECTION('ref_axis',(0.,-0.5,0.866025403784439));
#20142=DIRECTION('center_axis',(1.,0.,0.));
#20143=DIRECTION('ref_axis',(0.,0.866025403784439,0.5));
#20144=DIRECTION('center_axis',(-1.,0.,0.));
#20145=DIRECTION('ref_axis',(0.,-0.866025403784438,0.5));
#20146=DIRECTION('center_axis',(-1.,0.,0.));
#20147=DIRECTION('ref_axis',(0.,-0.866025403784439,0.5));
#20148=DIRECTION('center_axis',(1.,0.,0.));
#20149=DIRECTION('ref_axis',(0.,-0.866025403784439,0.5));
#20150=DIRECTION('center_axis',(1.,0.,0.));
#20151=DIRECTION('ref_axis',(0.,-0.866025403784438,0.5));
#20152=DIRECTION('center_axis',(1.,0.,0.));
#20153=DIRECTION('ref_axis',(0.,0.5,0.866025403784438));
#20154=DIRECTION('center_axis',(-1.,0.,0.));
#20155=DIRECTION('ref_axis',(0.,-1.,1.22464679914735E-16));
#20156=DIRECTION('center_axis',(-1.,0.,0.));
#20157=DIRECTION('ref_axis',(0.,-1.,1.22464679914735E-16));
#20158=DIRECTION('center_axis',(1.,0.,0.));
#20159=DIRECTION('ref_axis',(0.,-1.,1.22464679914735E-16));
#20160=DIRECTION('center_axis',(1.,0.,0.));
#20161=DIRECTION('ref_axis',(0.,-1.,1.22464679914735E-16));
#20162=DIRECTION('center_axis',(1.,0.,0.));
#20163=DIRECTION('ref_axis',(0.,1.22464679914735E-16,1.));
#20164=DIRECTION('center_axis',(-1.,0.,0.));
#20165=DIRECTION('ref_axis',(0.,-0.866025403784439,-0.5));
#20166=DIRECTION('center_axis',(-1.,0.,0.));
#20167=DIRECTION('ref_axis',(0.,-0.866025403784439,-0.5));
#20168=DIRECTION('center_axis',(1.,0.,0.));
#20169=DIRECTION('ref_axis',(0.,-0.866025403784439,-0.5));
#20170=DIRECTION('center_axis',(1.,0.,0.));
#20171=DIRECTION('ref_axis',(0.,-0.866025403784439,-0.5));
#20172=DIRECTION('center_axis',(1.,0.,0.));
#20173=DIRECTION('ref_axis',(0.,-0.5,0.866025403784439));
#20174=DIRECTION('center_axis',(-1.,0.,0.));
#20175=DIRECTION('ref_axis',(0.,-0.500000000000001,-0.866025403784438));
#20176=DIRECTION('center_axis',(-1.,0.,0.));
#20177=DIRECTION('ref_axis',(0.,-0.5,-0.866025403784438));
#20178=DIRECTION('center_axis',(1.,0.,0.));
#20179=DIRECTION('ref_axis',(0.,-0.5,-0.866025403784438));
#20180=DIRECTION('center_axis',(1.,0.,0.));
#20181=DIRECTION('ref_axis',(0.,-0.5,-0.866025403784438));
#20182=DIRECTION('center_axis',(1.,0.,0.));
#20183=DIRECTION('ref_axis',(0.,-0.866025403784438,0.5));
#20184=DIRECTION('center_axis',(-1.,0.,0.));
#20185=DIRECTION('ref_axis',(0.,-1.83697019872103E-16,-1.));
#20186=DIRECTION('center_axis',(-1.,0.,0.));
#20187=DIRECTION('ref_axis',(0.,-1.83697019872103E-16,-1.));
#20188=DIRECTION('center_axis',(1.,0.,0.));
#20189=DIRECTION('ref_axis',(0.,-1.83697019872103E-16,-1.));
#20190=DIRECTION('center_axis',(1.,0.,0.));
#20191=DIRECTION('ref_axis',(0.,-1.83697019872103E-16,-1.));
#20192=DIRECTION('center_axis',(1.,0.,0.));
#20193=DIRECTION('ref_axis',(0.,-1.,1.83697019872103E-16));
#20194=DIRECTION('center_axis',(-1.,0.,0.));
#20195=DIRECTION('ref_axis',(0.,0.499999999999999,-0.866025403784439));
#20196=DIRECTION('center_axis',(-1.,0.,0.));
#20197=DIRECTION('ref_axis',(0.,0.499999999999999,-0.866025403784439));
#20198=DIRECTION('center_axis',(1.,0.,0.));
#20199=DIRECTION('ref_axis',(0.,0.499999999999999,-0.866025403784439));
#20200=DIRECTION('center_axis',(1.,0.,0.));
#20201=DIRECTION('ref_axis',(0.,0.499999999999999,-0.866025403784439));
#20202=DIRECTION('center_axis',(1.,0.,0.));
#20203=DIRECTION('ref_axis',(0.,-0.866025403784439,-0.499999999999999));
#20204=DIRECTION('center_axis',(-1.,0.,0.));
#20205=DIRECTION('ref_axis',(0.,0.866025403784438,-0.500000000000001));
#20206=DIRECTION('center_axis',(-1.,0.,0.));
#20207=DIRECTION('ref_axis',(0.,0.866025403784438,-0.5));
#20208=DIRECTION('center_axis',(1.,0.,0.));
#20209=DIRECTION('ref_axis',(0.,0.866025403784438,-0.5));
#20210=DIRECTION('center_axis',(1.,0.,0.));
#20211=DIRECTION('ref_axis',(0.,0.866025403784438,-0.5));
#20212=DIRECTION('center_axis',(1.,0.,0.));
#20213=DIRECTION('ref_axis',(0.,-0.5,-0.866025403784438));
#20214=DIRECTION('center_axis',(1.,0.,0.));
#20215=DIRECTION('ref_axis',(0.,1.,0.));
#20216=DIRECTION('center_axis',(-1.,0.,0.));
#20217=DIRECTION('ref_axis',(0.,1.,0.));
#20218=DIRECTION('',(-0.707106781186546,0.707106781186549,8.65956056235495E-17));
#20219=DIRECTION('center_axis',(1.,0.,0.));
#20220=DIRECTION('ref_axis',(0.,1.,0.));
#20221=DIRECTION('center_axis',(1.,0.,0.));
#20222=DIRECTION('ref_axis',(0.,0.,-1.));
#20223=DIRECTION('center_axis',(1.,0.,0.));
#20224=DIRECTION('ref_axis',(0.,0.,-1.));
#20225=DIRECTION('center_axis',(1.,0.,0.));
#20226=DIRECTION('ref_axis',(0.,1.,0.));
#20227=DIRECTION('center_axis',(-1.,0.,0.));
#20228=DIRECTION('ref_axis',(0.,1.,0.));
#20229=DIRECTION('',(-1.,0.,0.));
#20230=DIRECTION('center_axis',(-1.,0.,0.));
#20231=DIRECTION('ref_axis',(0.,1.,0.));
#20232=DIRECTION('center_axis',(1.,0.,0.));
#20233=DIRECTION('ref_axis',(0.,1.,0.));
#20234=DIRECTION('',(0.707106781186546,0.707106781186549,-8.65956056235495E-17));
#20235=DIRECTION('center_axis',(-1.,0.,0.));
#20236=DIRECTION('ref_axis',(0.,1.,0.));
#20237=DIRECTION('center_axis',(-1.,0.,0.));
#20238=DIRECTION('ref_axis',(0.,0.,1.));
#20239=DIRECTION('center_axis',(1.,0.,0.));
#20240=DIRECTION('ref_axis',(0.,0.,-1.));
#20241=DIRECTION('center_axis',(1.,0.,0.));
#20242=DIRECTION('ref_axis',(0.,1.,0.));
#20243=DIRECTION('',(-1.,0.,0.));
#20244=DIRECTION('center_axis',(1.,0.,0.));
#20245=DIRECTION('ref_axis',(0.,0.,-1.));
#20246=DIRECTION('center_axis',(0.,0.999997730284958,0.00213059262460322));
#20247=DIRECTION('ref_axis',(0.,-0.00213059262460322,0.999997730284958));
#20248=DIRECTION('',(1.,0.,0.));
#20249=DIRECTION('',(-1.,0.,0.));
#20250=DIRECTION('center_axis',(1.,0.,0.));
#20251=DIRECTION('ref_axis',(0.,0.,-1.));
#20252=DIRECTION('center_axis',(1.,0.,0.));
#20253=DIRECTION('ref_axis',(0.,0.,-1.));
#20254=DIRECTION('center_axis',(-1.,0.,0.));
#20255=DIRECTION('ref_axis',(0.,0.,-1.));
#20256=DIRECTION('center_axis',(-1.,0.,0.));
#20257=DIRECTION('ref_axis',(0.,1.,0.));
#20258=DIRECTION('center_axis',(1.,0.,0.));
#20259=DIRECTION('ref_axis',(0.,0.,-1.));
#20260=DIRECTION('center_axis',(1.,0.,0.));
#20261=DIRECTION('ref_axis',(0.,0.,-1.));
#20262=DIRECTION('center_axis',(1.,0.,0.));
#20263=DIRECTION('ref_axis',(0.,1.,0.));
#20264=DIRECTION('center_axis',(1.,0.,0.));
#20265=DIRECTION('ref_axis',(0.,0.,-1.));
#20266=DIRECTION('center_axis',(1.,0.,0.));
#20267=DIRECTION('ref_axis',(0.,1.,0.));
#20268=DIRECTION('center_axis',(1.,0.,0.));
#20269=DIRECTION('ref_axis',(0.,0.,-1.));
#20270=DIRECTION('',(-1.,0.,0.));
#20271=DIRECTION('center_axis',(0.,0.501844012480496,0.864958141841255));
#20272=DIRECTION('ref_axis',(1.,0.,0.));
#20273=DIRECTION('',(1.,0.,0.));
#20274=DIRECTION('center_axis',(1.,0.,0.));
#20275=DIRECTION('ref_axis',(0.,0.5,-0.866025403784439));
#20276=DIRECTION('center_axis',(-1.,0.,0.));
#20277=DIRECTION('ref_axis',(0.,0.5,-0.866025403784439));
#20278=DIRECTION('center_axis',(1.,0.,0.));
#20279=DIRECTION('ref_axis',(0.,0.5,-0.866025403784439));
#20280=DIRECTION('center_axis',(0.,0.864958141841257,0.501844012480492));
#20281=DIRECTION('ref_axis',(1.,0.,0.));
#20282=DIRECTION('',(1.,0.,0.));
#20283=DIRECTION('',(-1.,0.,0.));
#20284=DIRECTION('center_axis',(-1.,0.,0.));
#20285=DIRECTION('ref_axis',(0.,1.,0.));
#20286=DIRECTION('center_axis',(1.,0.,0.));
#20287=DIRECTION('ref_axis',(0.,0.,-1.));
#20288=DIRECTION('center_axis',(1.,0.,0.));
#20289=DIRECTION('ref_axis',(0.,0.,-1.));
#20290=DIRECTION('center_axis',(1.,0.,0.));
#20291=DIRECTION('ref_axis',(0.,1.,0.));
#20292=DIRECTION('center_axis',(1.,0.,0.));
#20293=DIRECTION('ref_axis',(0.,0.,-1.));
#20294=DIRECTION('center_axis',(1.,0.,0.));
#20295=DIRECTION('ref_axis',(0.,1.,0.));
#20296=DIRECTION('center_axis',(1.,0.,0.));
#20297=DIRECTION('ref_axis',(0.,0.,-1.));
#20298=DIRECTION('',(-1.,0.,0.));
#20299=DIRECTION('center_axis',(0.,0.00213059262460321,0.999997730284958));
#20300=DIRECTION('ref_axis',(1.,0.,0.));
#20301=DIRECTION('',(1.,0.,0.));
#20302=DIRECTION('center_axis',(1.,0.,0.));
#20303=DIRECTION('ref_axis',(0.,0.866025403784439,-0.5));
#20304=DIRECTION('center_axis',(-1.,0.,0.));
#20305=DIRECTION('ref_axis',(0.,0.866025403784439,-0.5));
#20306=DIRECTION('center_axis',(1.,0.,0.));
#20307=DIRECTION('ref_axis',(0.,0.866025403784439,-0.5));
#20308=DIRECTION('center_axis',(0.,0.49815371780446,0.867088734465853));
#20309=DIRECTION('ref_axis',(1.,0.,0.));
#20310=DIRECTION('',(1.,0.,0.));
#20311=DIRECTION('',(-1.,0.,0.));
#20312=DIRECTION('center_axis',(-1.,0.,0.));
#20313=DIRECTION('ref_axis',(0.,1.,0.));
#20314=DIRECTION('center_axis',(1.,0.,0.));
#20315=DIRECTION('ref_axis',(0.,0.,-1.));
#20316=DIRECTION('center_axis',(1.,0.,0.));
#20317=DIRECTION('ref_axis',(0.,0.,-1.));
#20318=DIRECTION('center_axis',(1.,0.,0.));
#20319=DIRECTION('ref_axis',(0.,1.,0.));
#20320=DIRECTION('center_axis',(1.,0.,0.));
#20321=DIRECTION('ref_axis',(0.,0.,-1.));
#20322=DIRECTION('center_axis',(1.,0.,0.));
#20323=DIRECTION('ref_axis',(0.,1.,0.));
#20324=DIRECTION('center_axis',(1.,0.,0.));
#20325=DIRECTION('ref_axis',(0.,0.,-1.));
#20326=DIRECTION('',(-1.,0.,0.));
#20327=DIRECTION('center_axis',(0.,-0.498153717804456,0.867088734465855));
#20328=DIRECTION('ref_axis',(1.,0.,0.));
#20329=DIRECTION('',(1.,0.,0.));
#20330=DIRECTION('center_axis',(1.,0.,0.));
#20331=DIRECTION('ref_axis',(0.,1.,-6.12323399573676E-17));
#20332=DIRECTION('center_axis',(-1.,0.,0.));
#20333=DIRECTION('ref_axis',(0.,1.,-6.12323399573677E-17));
#20334=DIRECTION('center_axis',(1.,0.,0.));
#20335=DIRECTION('ref_axis',(0.,1.,-6.12323399573677E-17));
#20336=DIRECTION('center_axis',(0.,-0.00213059262459345,0.999997730284958));
#20337=DIRECTION('ref_axis',(1.,0.,0.));
#20338=DIRECTION('',(1.,0.,0.));
#20339=DIRECTION('',(-1.,0.,0.));
#20340=DIRECTION('center_axis',(-1.,0.,0.));
#20341=DIRECTION('ref_axis',(0.,1.,0.));
#20342=DIRECTION('center_axis',(1.,0.,0.));
#20343=DIRECTION('ref_axis',(0.,0.,-1.));
#20344=DIRECTION('center_axis',(1.,0.,0.));
#20345=DIRECTION('ref_axis',(0.,0.,-1.));
#20346=DIRECTION('center_axis',(1.,0.,0.));
#20347=DIRECTION('ref_axis',(0.,1.,0.));
#20348=DIRECTION('center_axis',(1.,0.,0.));
#20349=DIRECTION('ref_axis',(0.,0.,-1.));
#20350=DIRECTION('center_axis',(1.,0.,0.));
#20351=DIRECTION('ref_axis',(0.,1.,0.));
#20352=DIRECTION('center_axis',(1.,0.,0.));
#20353=DIRECTION('ref_axis',(0.,0.,-1.));
#20354=DIRECTION('',(-1.,0.,0.));
#20355=DIRECTION('center_axis',(0.,-0.864958141841252,0.5018440124805));
#20356=DIRECTION('ref_axis',(1.,0.,0.));
#20357=DIRECTION('',(1.,0.,0.));
#20358=DIRECTION('center_axis',(1.,0.,0.));
#20359=DIRECTION('ref_axis',(0.,0.866025403784439,0.5));
#20360=DIRECTION('center_axis',(-1.,0.,0.));
#20361=DIRECTION('ref_axis',(0.,0.866025403784439,0.5));
#20362=DIRECTION('center_axis',(1.,0.,0.));
#20363=DIRECTION('ref_axis',(0.,0.866025403784439,0.5));
#20364=DIRECTION('center_axis',(0.,-0.501844012480502,0.864958141841251));
#20365=DIRECTION('ref_axis',(1.,0.,0.));
#20366=DIRECTION('',(1.,0.,0.));
#20367=DIRECTION('',(-1.,0.,0.));
#20368=DIRECTION('center_axis',(-1.,0.,0.));
#20369=DIRECTION('ref_axis',(0.,1.,0.));
#20370=DIRECTION('center_axis',(1.,0.,0.));
#20371=DIRECTION('ref_axis',(0.,0.,-1.));
#20372=DIRECTION('center_axis',(1.,0.,0.));
#20373=DIRECTION('ref_axis',(0.,0.,-1.));
#20374=DIRECTION('center_axis',(1.,0.,0.));
#20375=DIRECTION('ref_axis',(0.,1.,0.));
#20376=DIRECTION('center_axis',(1.,0.,0.));
#20377=DIRECTION('ref_axis',(0.,0.,-1.));
#20378=DIRECTION('center_axis',(1.,0.,0.));
#20379=DIRECTION('ref_axis',(0.,1.,0.));
#20380=DIRECTION('center_axis',(1.,0.,0.));
#20381=DIRECTION('ref_axis',(0.,0.,-1.));
#20382=DIRECTION('',(-1.,0.,0.));
#20383=DIRECTION('center_axis',(0.,-0.999997730284958,0.00213059262460321));
#20384=DIRECTION('ref_axis',(0.,-0.00213059262460321,-0.999997730284958));
#20385=DIRECTION('',(1.,0.,0.));
#20386=DIRECTION('center_axis',(1.,0.,0.));
#20387=DIRECTION('ref_axis',(0.,0.5,0.866025403784438));
#20388=DIRECTION('center_axis',(-1.,0.,0.));
#20389=DIRECTION('ref_axis',(0.,0.5,0.866025403784438));
#20390=DIRECTION('center_axis',(1.,0.,0.));
#20391=DIRECTION('ref_axis',(0.,0.5,0.866025403784438));
#20392=DIRECTION('center_axis',(1.,0.,0.));
#20393=DIRECTION('ref_axis',(0.,0.,-1.));
#20394=DIRECTION('center_axis',(1.,0.,0.));
#20395=DIRECTION('ref_axis',(0.,0.,-1.));
#20396=DIRECTION('center_axis',(1.,0.,0.));
#20397=DIRECTION('ref_axis',(0.,1.22464679914735E-16,1.));
#20398=DIRECTION('center_axis',(1.,0.,0.));
#20399=DIRECTION('ref_axis',(0.,0.,-1.));
#20400=DIRECTION('center_axis',(1.,0.,0.));
#20401=DIRECTION('ref_axis',(0.,-0.5,0.866025403784439));
#20402=DIRECTION('center_axis',(1.,0.,0.));
#20403=DIRECTION('ref_axis',(0.,0.,-1.));
#20404=DIRECTION('center_axis',(1.,0.,0.));
#20405=DIRECTION('ref_axis',(0.,-0.866025403784438,0.500000000000001));
#20406=DIRECTION('center_axis',(1.,0.,0.));
#20407=DIRECTION('ref_axis',(0.,0.,-1.));
#20408=DIRECTION('center_axis',(1.,0.,0.));
#20409=DIRECTION('ref_axis',(0.,-1.,1.83697019872103E-16));
#20410=DIRECTION('center_axis',(1.,0.,0.));
#20411=DIRECTION('ref_axis',(0.,0.,-1.));
#20412=DIRECTION('center_axis',(1.,0.,0.));
#20413=DIRECTION('ref_axis',(0.,-0.866025403784439,-0.499999999999999));
#20414=DIRECTION('center_axis',(1.,0.,0.));
#20415=DIRECTION('ref_axis',(0.,0.,-1.));
#20416=DIRECTION('center_axis',(1.,0.,0.));
#20417=DIRECTION('ref_axis',(0.,-0.500000000000001,-0.866025403784438));
#20418=DIRECTION('center_axis',(1.,0.,0.));
#20419=DIRECTION('ref_axis',(0.,0.,-1.));
#20420=DIRECTION('center_axis',(1.,0.,0.));
#20421=DIRECTION('ref_axis',(0.,0.,-1.));
#20422=DIRECTION('center_axis',(-1.,0.,0.));
#20423=DIRECTION('ref_axis',(0.,-1.,-1.4619715404243E-10));
#20424=DIRECTION('center_axis',(1.,0.,0.));
#20425=DIRECTION('ref_axis',(0.,0.,-1.));
#20426=DIRECTION('center_axis',(0.,-0.867088734465855,0.498153717804456));
#20427=DIRECTION('ref_axis',(0.,-0.498153717804456,-0.867088734465855));
#20428=DIRECTION('',(-1.,0.,0.));
#20429=DIRECTION('',(1.,0.,0.));
#20430=DIRECTION('center_axis',(1.,0.,0.));
#20431=DIRECTION('ref_axis',(0.,0.5,-0.866025403784439));
#20432=DIRECTION('center_axis',(1.,0.,0.));
#20433=DIRECTION('ref_axis',(0.,0.5,-0.866025403784439));
#20434=DIRECTION('center_axis',(1.,0.,0.));
#20435=DIRECTION('ref_axis',(0.,0.,-1.));
#20436=DIRECTION('',(1.,0.,0.));
#20437=DIRECTION('center_axis',(1.,0.,0.));
#20438=DIRECTION('ref_axis',(0.,0.,-1.));
#20439=DIRECTION('center_axis',(0.,0.867088734465855,0.498153717804456));
#20440=DIRECTION('ref_axis',(0.,-0.498153717804456,0.867088734465855));
#20441=DIRECTION('',(-1.,0.,0.));
#20442=DIRECTION('center_axis',(1.,0.,0.));
#20443=DIRECTION('ref_axis',(0.,-1.,5.66553889764798E-16));
#20444=DIRECTION('center_axis',(1.,0.,0.));
#20445=DIRECTION('ref_axis',(0.,0.,-1.));
#20446=DIRECTION('center_axis',(1.,0.,0.));
#20447=DIRECTION('ref_axis',(0.,1.,0.));
#20448=DIRECTION('center_axis',(1.,0.,0.));
#20449=DIRECTION('ref_axis',(0.,0.,-1.));
#20450=DIRECTION('',(-1.,0.,0.));
#20451=DIRECTION('center_axis',(0.,-0.867088734465854,-0.498153717804458));
#20452=DIRECTION('ref_axis',(0.,0.498153717804458,-0.867088734465854));
#20453=DIRECTION('',(1.,0.,0.));
#20454=DIRECTION('center_axis',(1.,0.,0.));
#20455=DIRECTION('ref_axis',(0.,1.22464679914735E-16,1.));
#20456=DIRECTION('center_axis',(-1.,0.,0.));
#20457=DIRECTION('ref_axis',(0.,1.22464679914735E-16,1.));
#20458=DIRECTION('center_axis',(-1.,0.,0.));
#20459=DIRECTION('ref_axis',(0.,1.,0.));
#20460=DIRECTION('center_axis',(1.,0.,0.));
#20461=DIRECTION('ref_axis',(0.,0.,-1.));
#20462=DIRECTION('center_axis',(0.,-0.999997730284958,-0.00213059262459835));
#20463=DIRECTION('ref_axis',(0.,0.00213059262459835,-0.999997730284958));
#20464=DIRECTION('',(-1.,0.,0.));
#20465=DIRECTION('',(1.,0.,0.));
#20466=DIRECTION('center_axis',(1.,0.,0.));
#20467=DIRECTION('ref_axis',(0.,1.,0.));
#20468=DIRECTION('center_axis',(1.,0.,0.));
#20469=DIRECTION('ref_axis',(0.,0.,-1.));
#20470=DIRECTION('center_axis',(1.,0.,0.));
#20471=DIRECTION('ref_axis',(0.,1.,0.));
#20472=DIRECTION('center_axis',(1.,0.,0.));
#20473=DIRECTION('ref_axis',(0.,0.,-1.));
#20474=DIRECTION('',(-1.,0.,0.));
#20475=DIRECTION('center_axis',(0.,-0.501844012480502,-0.864958141841251));
#20476=DIRECTION('ref_axis',(-1.,0.,0.));
#20477=DIRECTION('',(1.,0.,0.));
#20478=DIRECTION('center_axis',(1.,0.,0.));
#20479=DIRECTION('ref_axis',(0.,-0.5,0.866025403784439));
#20480=DIRECTION('center_axis',(-1.,0.,0.));
#20481=DIRECTION('ref_axis',(0.,-0.5,0.866025403784439));
#20482=DIRECTION('center_axis',(-1.,0.,0.));
#20483=DIRECTION('ref_axis',(0.,1.,0.));
#20484=DIRECTION('center_axis',(1.,0.,0.));
#20485=DIRECTION('ref_axis',(0.,0.,-1.));
#20486=DIRECTION('center_axis',(0.,-0.864958141841251,-0.501844012480502));
#20487=DIRECTION('ref_axis',(-1.,0.,0.));
#20488=DIRECTION('',(-1.,0.,0.));
#20489=DIRECTION('',(1.,0.,0.));
#20490=DIRECTION('center_axis',(1.,0.,0.));
#20491=DIRECTION('ref_axis',(0.,1.,0.));
#20492=DIRECTION('center_axis',(1.,0.,0.));
#20493=DIRECTION('ref_axis',(0.,0.,-1.));
#20494=DIRECTION('center_axis',(1.,0.,0.));
#20495=DIRECTION('ref_axis',(0.,1.,0.));
#20496=DIRECTION('center_axis',(1.,0.,0.));
#20497=DIRECTION('ref_axis',(0.,0.,-1.));
#20498=DIRECTION('',(-1.,0.,0.));
#20499=DIRECTION('center_axis',(0.,-0.00213059262460321,-0.999997730284958));
#20500=DIRECTION('ref_axis',(-1.,0.,0.));
#20501=DIRECTION('',(1.,0.,0.));
#20502=DIRECTION('center_axis',(1.,0.,0.));
#20503=DIRECTION('ref_axis',(0.,-0.866025403784438,0.5));
#20504=DIRECTION('center_axis',(-1.,0.,0.));
#20505=DIRECTION('ref_axis',(0.,-0.866025403784438,0.5));
#20506=DIRECTION('center_axis',(-1.,0.,0.));
#20507=DIRECTION('ref_axis',(0.,1.,0.));
#20508=DIRECTION('center_axis',(1.,0.,0.));
#20509=DIRECTION('ref_axis',(0.,0.,-1.));
#20510=DIRECTION('center_axis',(0.,-0.498153717804456,-0.867088734465856));
#20511=DIRECTION('ref_axis',(-1.,0.,0.));
#20512=DIRECTION('',(-1.,0.,0.));
#20513=DIRECTION('',(1.,0.,0.));
#20514=DIRECTION('center_axis',(1.,0.,0.));
#20515=DIRECTION('ref_axis',(0.,1.,0.));
#20516=DIRECTION('center_axis',(1.,0.,0.));
#20517=DIRECTION('ref_axis',(0.,0.,-1.));
#20518=DIRECTION('center_axis',(1.,0.,0.));
#20519=DIRECTION('ref_axis',(0.,1.,0.));
#20520=DIRECTION('center_axis',(1.,0.,0.));
#20521=DIRECTION('ref_axis',(0.,0.,-1.));
#20522=DIRECTION('',(-1.,0.,0.));
#20523=DIRECTION('center_axis',(0.,0.498153717804458,-0.867088734465854));
#20524=DIRECTION('ref_axis',(-1.,0.,0.));
#20525=DIRECTION('',(1.,0.,0.));
#20526=DIRECTION('center_axis',(1.,0.,0.));
#20527=DIRECTION('ref_axis',(0.,-1.,1.83697019872103E-16));
#20528=DIRECTION('center_axis',(-1.,0.,0.));
#20529=DIRECTION('ref_axis',(0.,-1.,1.83697019872103E-16));
#20530=DIRECTION('center_axis',(-1.,0.,0.));
#20531=DIRECTION('ref_axis',(0.,1.,0.));
#20532=DIRECTION('center_axis',(1.,0.,0.));
#20533=DIRECTION('ref_axis',(0.,0.,-1.));
#20534=DIRECTION('center_axis',(0.,0.0021305926246276,-0.999997730284958));
#20535=DIRECTION('ref_axis',(-1.,0.,0.));
#20536=DIRECTION('',(-1.,0.,0.));
#20537=DIRECTION('',(1.,0.,0.));
#20538=DIRECTION('center_axis',(1.,0.,0.));
#20539=DIRECTION('ref_axis',(0.,1.,0.));
#20540=DIRECTION('center_axis',(1.,0.,0.));
#20541=DIRECTION('ref_axis',(0.,0.,-1.));
#20542=DIRECTION('center_axis',(1.,0.,0.));
#20543=DIRECTION('ref_axis',(0.,1.,0.));
#20544=DIRECTION('center_axis',(1.,0.,0.));
#20545=DIRECTION('ref_axis',(0.,0.,-1.));
#20546=DIRECTION('',(-1.,0.,0.));
#20547=DIRECTION('center_axis',(0.,0.864958141841252,-0.5018440124805));
#20548=DIRECTION('ref_axis',(-1.,0.,0.));
#20549=DIRECTION('',(1.,0.,0.));
#20550=DIRECTION('center_axis',(1.,0.,0.));
#20551=DIRECTION('ref_axis',(0.,-0.866025403784439,-0.499999999999999));
#20552=DIRECTION('center_axis',(-1.,0.,0.));
#20553=DIRECTION('ref_axis',(0.,-0.866025403784439,-0.499999999999999));
#20554=DIRECTION('center_axis',(-1.,0.,0.));
#20555=DIRECTION('ref_axis',(0.,1.,0.));
#20556=DIRECTION('center_axis',(1.,0.,0.));
#20557=DIRECTION('ref_axis',(0.,0.,-1.));
#20558=DIRECTION('center_axis',(0.,0.501844012480498,-0.864958141841254));
#20559=DIRECTION('ref_axis',(-1.,0.,0.));
#20560=DIRECTION('',(-1.,0.,0.));
#20561=DIRECTION('',(1.,0.,0.));
#20562=DIRECTION('center_axis',(1.,0.,0.));
#20563=DIRECTION('ref_axis',(0.,1.,0.));
#20564=DIRECTION('center_axis',(1.,0.,0.));
#20565=DIRECTION('ref_axis',(0.,0.,-1.));
#20566=DIRECTION('',(1.,0.,0.));
#20567=DIRECTION('center_axis',(1.,0.,0.));
#20568=DIRECTION('ref_axis',(0.,0.,-1.));
#20569=DIRECTION('center_axis',(1.,0.,0.));
#20570=DIRECTION('ref_axis',(0.,1.,0.));
#20571=DIRECTION('center_axis',(1.,0.,0.));
#20572=DIRECTION('ref_axis',(0.,0.,-1.));
#20573=DIRECTION('center_axis',(-1.,0.,0.));
#20574=DIRECTION('ref_axis',(0.,1.,0.));
#20575=DIRECTION('center_axis',(1.,0.,0.));
#20576=DIRECTION('ref_axis',(0.,1.,0.));
#20577=DIRECTION('center_axis',(1.,0.,0.));
#20578=DIRECTION('ref_axis',(0.,0.,-1.));
#20579=DIRECTION('center_axis',(1.,0.,0.));
#20580=DIRECTION('ref_axis',(0.,1.,0.));
#20581=DIRECTION('center_axis',(1.,0.,0.));
#20582=DIRECTION('ref_axis',(0.,0.,-1.));
#20583=DIRECTION('',(-1.,0.,0.));
#20584=DIRECTION('center_axis',(0.,0.999997730284958,-0.00213059262460321));
#20585=DIRECTION('ref_axis',(0.,0.00213059262460321,0.999997730284958));
#20586=DIRECTION('',(1.,0.,0.));
#20587=DIRECTION('center_axis',(1.,0.,0.));
#20588=DIRECTION('ref_axis',(0.,-0.5,-0.866025403784438));
#20589=DIRECTION('center_axis',(-1.,0.,0.));
#20590=DIRECTION('ref_axis',(0.,-0.5,-0.866025403784438));
#20591=DIRECTION('center_axis',(0.,0.867088734465856,-0.498153717804456));
#20592=DIRECTION('ref_axis',(0.,0.498153717804456,0.867088734465855));
#20593=DIRECTION('',(-1.,0.,0.));
#20594=DIRECTION('center_axis',(1.,0.,0.));
#20595=DIRECTION('ref_axis',(0.,1.,0.));
#20596=DIRECTION('center_axis',(1.,0.,0.));
#20597=DIRECTION('ref_axis',(0.,0.,-1.));
#20598=DIRECTION('center_axis',(1.,0.,0.));
#20599=DIRECTION('ref_axis',(0.,-0.5,-0.866025403784438));
#20600=DIRECTION('center_axis',(1.,0.,0.));
#20601=DIRECTION('ref_axis',(0.,-0.5,-0.866025403784438));
#20602=DIRECTION('center_axis',(1.,0.,0.));
#20603=DIRECTION('ref_axis',(0.,0.,-1.));
#20604=DIRECTION('center_axis',(-1.,0.,0.));
#20605=DIRECTION('ref_axis',(0.,1.,0.));
#20606=DIRECTION('center_axis',(-1.,0.,0.));
#20607=DIRECTION('ref_axis',(0.,1.,0.));
#20608=DIRECTION('center_axis',(1.,0.,0.));
#20609=DIRECTION('ref_axis',(0.,0.,-1.));
#20610=DIRECTION('center_axis',(1.,0.,0.));
#20611=DIRECTION('ref_axis',(0.,1.,0.));
#20612=DIRECTION('center_axis',(1.,0.,0.));
#20613=DIRECTION('ref_axis',(0.,1.,0.));
#20614=DIRECTION('center_axis',(-1.,0.,0.));
#20615=DIRECTION('ref_axis',(0.,1.,1.0886778522233E-13));
#20616=DIRECTION('center_axis',(1.,0.,0.));
#20617=DIRECTION('ref_axis',(0.,1.,1.0886778522233E-13));
#20618=DIRECTION('center_axis',(1.,0.,0.));
#20619=DIRECTION('ref_axis',(0.,-0.5,-0.866025403784438));
#20620=DIRECTION('center_axis',(1.,0.,0.));
#20621=DIRECTION('ref_axis',(0.,0.,-1.));
#20622=DIRECTION('center_axis',(1.,0.,0.));
#20623=DIRECTION('ref_axis',(0.,1.,0.));
#20624=DIRECTION('center_axis',(1.,0.,0.));
#20625=DIRECTION('ref_axis',(0.,-0.866025403784439,-0.499999999999999));
#20626=DIRECTION('center_axis',(1.,0.,0.));
#20627=DIRECTION('ref_axis',(0.,-0.866025403784439,-0.499999999999999));
#20628=DIRECTION('center_axis',(1.,0.,0.));
#20629=DIRECTION('ref_axis',(0.,-0.866025403784439,-0.499999999999999));
#20630=DIRECTION('center_axis',(1.,0.,0.));
#20631=DIRECTION('ref_axis',(0.,1.,0.));
#20632=DIRECTION('center_axis',(1.,0.,0.));
#20633=DIRECTION('ref_axis',(0.,1.,0.));
#20634=DIRECTION('center_axis',(1.,0.,0.));
#20635=DIRECTION('ref_axis',(0.,-1.,1.83697019872103E-16));
#20636=DIRECTION('center_axis',(1.,0.,0.));
#20637=DIRECTION('ref_axis',(0.,-1.,1.83697019872103E-16));
#20638=DIRECTION('center_axis',(1.,0.,0.));
#20639=DIRECTION('ref_axis',(0.,-1.,1.83697019872103E-16));
#20640=DIRECTION('center_axis',(1.,0.,0.));
#20641=DIRECTION('ref_axis',(0.,1.,0.));
#20642=DIRECTION('center_axis',(1.,0.,0.));
#20643=DIRECTION('ref_axis',(0.,1.,0.));
#20644=DIRECTION('center_axis',(1.,0.,0.));
#20645=DIRECTION('ref_axis',(0.,-0.866025403784438,0.5));
#20646=DIRECTION('center_axis',(1.,0.,0.));
#20647=DIRECTION('ref_axis',(0.,-0.866025403784438,0.5));
#20648=DIRECTION('center_axis',(1.,0.,0.));
#20649=DIRECTION('ref_axis',(0.,-0.866025403784438,0.5));
#20650=DIRECTION('center_axis',(1.,0.,0.));
#20651=DIRECTION('ref_axis',(0.,1.,0.));
#20652=DIRECTION('center_axis',(1.,0.,0.));
#20653=DIRECTION('ref_axis',(0.,1.,0.));
#20654=DIRECTION('center_axis',(1.,0.,0.));
#20655=DIRECTION('ref_axis',(0.,-0.5,0.866025403784439));
#20656=DIRECTION('center_axis',(1.,0.,0.));
#20657=DIRECTION('ref_axis',(0.,-0.5,0.866025403784439));
#20658=DIRECTION('center_axis',(1.,0.,0.));
#20659=DIRECTION('ref_axis',(0.,-0.5,0.866025403784439));
#20660=DIRECTION('center_axis',(1.,0.,0.));
#20661=DIRECTION('ref_axis',(0.,1.,0.));
#20662=DIRECTION('center_axis',(1.,0.,0.));
#20663=DIRECTION('ref_axis',(0.,1.,0.));
#20664=DIRECTION('center_axis',(1.,0.,0.));
#20665=DIRECTION('ref_axis',(0.,1.22464679914735E-16,1.));
#20666=DIRECTION('center_axis',(1.,0.,0.));
#20667=DIRECTION('ref_axis',(0.,1.22464679914735E-16,1.));
#20668=DIRECTION('center_axis',(1.,0.,0.));
#20669=DIRECTION('ref_axis',(0.,1.22464679914735E-16,1.));
#20670=DIRECTION('center_axis',(1.,0.,0.));
#20671=DIRECTION('ref_axis',(0.,1.,0.));
#20672=DIRECTION('center_axis',(1.,0.,0.));
#20673=DIRECTION('ref_axis',(0.,1.,0.));
#20674=DIRECTION('center_axis',(1.,0.,0.));
#20675=DIRECTION('ref_axis',(0.,0.5,0.866025403784438));
#20676=DIRECTION('center_axis',(1.,0.,0.));
#20677=DIRECTION('ref_axis',(0.,0.5,0.866025403784438));
#20678=DIRECTION('center_axis',(1.,0.,0.));
#20679=DIRECTION('ref_axis',(0.,0.5,0.866025403784438));
#20680=DIRECTION('center_axis',(1.,0.,0.));
#20681=DIRECTION('ref_axis',(0.,1.,0.));
#20682=DIRECTION('center_axis',(1.,0.,0.));
#20683=DIRECTION('ref_axis',(0.,1.,0.));
#20684=DIRECTION('center_axis',(1.,0.,0.));
#20685=DIRECTION('ref_axis',(0.,0.866025403784439,0.5));
#20686=DIRECTION('center_axis',(1.,0.,0.));
#20687=DIRECTION('ref_axis',(0.,0.866025403784439,0.5));
#20688=DIRECTION('center_axis',(1.,0.,0.));
#20689=DIRECTION('ref_axis',(0.,0.866025403784439,0.5));
#20690=DIRECTION('center_axis',(1.,0.,0.));
#20691=DIRECTION('ref_axis',(0.,1.,0.));
#20692=DIRECTION('center_axis',(1.,0.,0.));
#20693=DIRECTION('ref_axis',(0.,1.,0.));
#20694=DIRECTION('center_axis',(1.,0.,0.));
#20695=DIRECTION('ref_axis',(0.,1.,-6.12323399573677E-17));
#20696=DIRECTION('center_axis',(1.,0.,0.));
#20697=DIRECTION('ref_axis',(0.,1.,-6.12323399573677E-17));
#20698=DIRECTION('center_axis',(1.,0.,0.));
#20699=DIRECTION('ref_axis',(0.,1.,-6.12323399573677E-17));
#20700=DIRECTION('center_axis',(1.,0.,0.));
#20701=DIRECTION('ref_axis',(0.,1.,0.));
#20702=DIRECTION('center_axis',(1.,0.,0.));
#20703=DIRECTION('ref_axis',(0.,1.,0.));
#20704=DIRECTION('center_axis',(1.,0.,0.));
#20705=DIRECTION('ref_axis',(0.,0.866025403784439,-0.5));
#20706=DIRECTION('center_axis',(1.,0.,0.));
#20707=DIRECTION('ref_axis',(0.,0.866025403784439,-0.5));
#20708=DIRECTION('center_axis',(1.,0.,0.));
#20709=DIRECTION('ref_axis',(0.,0.866025403784439,-0.5));
#20710=DIRECTION('center_axis',(1.,0.,0.));
#20711=DIRECTION('ref_axis',(0.,1.,0.));
#20712=DIRECTION('center_axis',(1.,0.,0.));
#20713=DIRECTION('ref_axis',(0.,1.,0.));
#20714=DIRECTION('center_axis',(1.,0.,0.));
#20715=DIRECTION('ref_axis',(0.,0.5,-0.866025403784439));
#20716=DIRECTION('center_axis',(1.,0.,0.));
#20717=DIRECTION('ref_axis',(0.,1.,0.));
#20718=DIRECTION('center_axis',(1.,0.,0.));
#20719=DIRECTION('ref_axis',(0.,1.,0.));
#20720=DIRECTION('center_axis',(1.,0.,0.));
#20721=DIRECTION('ref_axis',(0.,0.,-1.));
#20722=DIRECTION('center_axis',(1.,0.,0.));
#20723=DIRECTION('ref_axis',(0.,1.,0.));
#20724=DIRECTION('center_axis',(1.,0.,0.));
#20725=DIRECTION('ref_axis',(0.,1.,0.));
#20726=DIRECTION('center_axis',(1.,0.,0.));
#20727=DIRECTION('ref_axis',(0.,1.,0.));
#20728=DIRECTION('center_axis',(1.,0.,0.));
#20729=DIRECTION('ref_axis',(0.,0.,-1.));
#20730=DIRECTION('',(1.,0.,0.));
#20731=DIRECTION('center_axis',(1.,0.,0.));
#20732=DIRECTION('ref_axis',(0.,0.,-1.));
#20733=DIRECTION('center_axis',(-1.,0.,0.));
#20734=DIRECTION('ref_axis',(0.,0.,1.));
#20735=DIRECTION('center_axis',(1.,0.,0.));
#20736=DIRECTION('ref_axis',(0.,0.,-1.));
#20737=DIRECTION('center_axis',(1.,0.,0.));
#20738=DIRECTION('ref_axis',(0.,1.,0.));
#20739=DIRECTION('center_axis',(1.,0.,0.));
#20740=DIRECTION('ref_axis',(0.,1.,0.));
#20741=DIRECTION('center_axis',(1.,0.,0.));
#20742=DIRECTION('ref_axis',(0.,0.,-1.));
#20743=DIRECTION('',(-1.,0.,0.));
#20744=DIRECTION('center_axis',(1.,0.,0.));
#20745=DIRECTION('ref_axis',(0.,1.,0.));
#20746=DIRECTION('',(1.,0.,0.));
#20747=DIRECTION('center_axis',(-1.,0.,0.));
#20748=DIRECTION('ref_axis',(0.,0.5,0.866025403784438));
#20749=DIRECTION('center_axis',(1.,0.,0.));
#20750=DIRECTION('ref_axis',(0.,-0.5,-0.866025403784438));
#20751=DIRECTION('center_axis',(1.,0.,0.));
#20752=DIRECTION('ref_axis',(0.,-0.5,-0.866025403784438));
#20753=DIRECTION('center_axis',(-1.,0.,0.));
#20754=DIRECTION('ref_axis',(0.,0.866025403784439,0.499999999999999));
#20755=DIRECTION('center_axis',(1.,0.,0.));
#20756=DIRECTION('ref_axis',(0.,-0.866025403784439,-0.499999999999999));
#20757=DIRECTION('center_axis',(1.,0.,0.));
#20758=DIRECTION('ref_axis',(0.,-0.866025403784439,-0.499999999999999));
#20759=DIRECTION('center_axis',(-1.,0.,0.));
#20760=DIRECTION('ref_axis',(0.,1.,-1.83697019872103E-16));
#20761=DIRECTION('center_axis',(1.,0.,0.));
#20762=DIRECTION('ref_axis',(0.,-1.,1.83697019872103E-16));
#20763=DIRECTION('center_axis',(1.,0.,0.));
#20764=DIRECTION('ref_axis',(0.,-1.,1.83697019872103E-16));
#20765=DIRECTION('center_axis',(-1.,0.,0.));
#20766=DIRECTION('ref_axis',(0.,0.866025403784438,-0.5));
#20767=DIRECTION('center_axis',(1.,0.,0.));
#20768=DIRECTION('ref_axis',(0.,-0.866025403784438,0.5));
#20769=DIRECTION('center_axis',(1.,0.,0.));
#20770=DIRECTION('ref_axis',(0.,-0.866025403784438,0.5));
#20771=DIRECTION('center_axis',(-1.,0.,0.));
#20772=DIRECTION('ref_axis',(0.,0.5,-0.866025403784439));
#20773=DIRECTION('center_axis',(1.,0.,0.));
#20774=DIRECTION('ref_axis',(0.,-0.5,0.866025403784439));
#20775=DIRECTION('center_axis',(1.,0.,0.));
#20776=DIRECTION('ref_axis',(0.,-0.5,0.866025403784439));
#20777=DIRECTION('center_axis',(-1.,0.,0.));
#20778=DIRECTION('ref_axis',(0.,-1.22464679914735E-16,-1.));
#20779=DIRECTION('center_axis',(1.,0.,0.));
#20780=DIRECTION('ref_axis',(0.,1.22464679914735E-16,1.));
#20781=DIRECTION('center_axis',(1.,0.,0.));
#20782=DIRECTION('ref_axis',(0.,1.22464679914735E-16,1.));
#20783=DIRECTION('center_axis',(-1.,0.,0.));
#20784=DIRECTION('ref_axis',(0.,-0.5,-0.866025403784438));
#20785=DIRECTION('center_axis',(1.,0.,0.));
#20786=DIRECTION('ref_axis',(0.,0.5,0.866025403784438));
#20787=DIRECTION('center_axis',(1.,0.,0.));
#20788=DIRECTION('ref_axis',(0.,0.5,0.866025403784438));
#20789=DIRECTION('center_axis',(-1.,0.,0.));
#20790=DIRECTION('ref_axis',(0.,-0.866025403784439,-0.5));
#20791=DIRECTION('center_axis',(1.,0.,0.));
#20792=DIRECTION('ref_axis',(0.,0.866025403784439,0.5));
#20793=DIRECTION('center_axis',(1.,0.,0.));
#20794=DIRECTION('ref_axis',(0.,0.866025403784439,0.5));
#20795=DIRECTION('center_axis',(-1.,0.,0.));
#20796=DIRECTION('ref_axis',(0.,-1.,6.12323399573677E-17));
#20797=DIRECTION('center_axis',(1.,0.,0.));
#20798=DIRECTION('ref_axis',(0.,1.,-6.12323399573676E-17));
#20799=DIRECTION('center_axis',(1.,0.,0.));
#20800=DIRECTION('ref_axis',(0.,1.,-6.12323399573677E-17));
#20801=DIRECTION('center_axis',(-1.,0.,0.));
#20802=DIRECTION('ref_axis',(0.,-0.866025403784439,0.5));
#20803=DIRECTION('center_axis',(1.,0.,0.));
#20804=DIRECTION('ref_axis',(0.,0.866025403784439,-0.5));
#20805=DIRECTION('center_axis',(1.,0.,0.));
#20806=DIRECTION('ref_axis',(0.,0.866025403784439,-0.5));
#20807=DIRECTION('center_axis',(-1.,0.,0.));
#20808=DIRECTION('ref_axis',(0.,-0.5,0.866025403784439));
#20809=DIRECTION('center_axis',(1.,0.,0.));
#20810=DIRECTION('ref_axis',(0.,0.5,-0.866025403784439));
#20811=DIRECTION('center_axis',(1.,0.,0.));
#20812=DIRECTION('ref_axis',(0.,0.5,-0.866025403784439));
#20813=DIRECTION('center_axis',(-1.,0.,0.));
#20814=DIRECTION('ref_axis',(0.,0.,1.));
#20815=DIRECTION('center_axis',(1.,0.,0.));
#20816=DIRECTION('ref_axis',(0.,0.,-1.));
#20817=DIRECTION('center_axis',(1.,0.,0.));
#20818=DIRECTION('ref_axis',(0.,0.,-1.));
#20819=DIRECTION('center_axis',(-0.707106781186548,0.336582777174955,-0.621861748388816));
#20820=DIRECTION('ref_axis',(-0.660393123266679,0.,0.750920050832365));
#20821=DIRECTION('',(0.,-0.879445318492508,-0.475999928342022));
#20822=DIRECTION('',(0.,0.879445318492508,0.475999928342022));
#20823=DIRECTION('center_axis',(0.,-0.99962195122482,0.0274946291024896));
#20824=DIRECTION('ref_axis',(0.,-0.0274946291024896,-0.99962195122482));
#20825=DIRECTION('',(0.,-0.0274946291024896,-0.99962195122482));
#20826=DIRECTION('center_axis',(0.,-0.879445318492508,-0.475999928342023));
#20827=DIRECTION('ref_axis',(0.,0.475999928342023,-0.879445318492508));
#20828=DIRECTION('',(0.,0.475999928342023,-0.879445318492508));
#20829=DIRECTION('center_axis',(0.,-0.523622022882798,-0.851950689390018));
#20830=DIRECTION('ref_axis',(0.,0.851950689390018,-0.523622022882798));
#20831=DIRECTION('',(0.,0.851950689390018,-0.523622022882798));
#20832=DIRECTION('center_axis',(0.,-0.0274946291024888,-0.99962195122482));
#20833=DIRECTION('ref_axis',(0.,0.99962195122482,-0.0274946291024888));
#20834=DIRECTION('',(0.,0.99962195122482,-0.0274946291024888));
#20835=DIRECTION('center_axis',(0.,0.475999928342022,-0.879445318492509));
#20836=DIRECTION('ref_axis',(0.,0.879445318492508,0.475999928342022));
#20837=DIRECTION('',(0.,0.879445318492508,0.475999928342022));
#20838=DIRECTION('center_axis',(0.,0.851950689390018,-0.523622022882797));
#20839=DIRECTION('ref_axis',(0.,0.523622022882797,0.851950689390018));
#20840=DIRECTION('',(0.,0.523622022882797,0.851950689390018));
#20841=DIRECTION('center_axis',(1.,0.,0.));
#20842=DIRECTION('ref_axis',(0.,0.,-1.));
#20843=DIRECTION('center_axis',(0.,-0.475999928342023,0.879445318492508));
#20844=DIRECTION('ref_axis',(0.,-0.879445318492508,-0.475999928342023));
#20845=DIRECTION('',(0.,-0.879445318492508,-0.475999928342023));
#20846=DIRECTION('center_axis',(0.,0.0274946291024905,0.99962195122482));
#20847=DIRECTION('ref_axis',(0.,-0.99962195122482,0.0274946291024905));
#20848=DIRECTION('',(0.,-0.99962195122482,0.0274946291024905));
#20849=DIRECTION('center_axis',(0.,0.523622022882797,0.851950689390018));
#20850=DIRECTION('ref_axis',(0.,-0.851950689390018,0.523622022882797));
#20851=DIRECTION('',(0.,-0.851950689390018,0.523622022882797));
#20852=DIRECTION('center_axis',(0.,0.879445318492508,0.475999928342023));
#20853=DIRECTION('ref_axis',(0.,-0.475999928342023,0.879445318492508));
#20854=DIRECTION('',(0.,-0.475999928342023,0.879445318492508));
#20855=DIRECTION('center_axis',(0.,0.99962195122482,-0.0274946291024904));
#20856=DIRECTION('ref_axis',(0.,0.0274946291024904,0.99962195122482));
#20857=DIRECTION('',(0.,0.0274946291024904,0.99962195122482));
#20858=DIRECTION('center_axis',(0.,-0.851950689390018,0.523622022882797));
#20859=DIRECTION('ref_axis',(0.,-0.523622022882797,-0.851950689390018));
#20860=DIRECTION('',(0.,-0.523622022882797,-0.851950689390018));
#20861=DIRECTION('center_axis',(-1.,0.,0.));
#20862=DIRECTION('ref_axis',(0.,0.,1.));
#20863=DIRECTION('center_axis',(-1.,0.,0.));
#20864=DIRECTION('ref_axis',(0.,1.,0.));
#20865=DIRECTION('center_axis',(1.,0.,0.));
#20866=DIRECTION('ref_axis',(0.,0.,-1.));
#20867=DIRECTION('',(-0.330350424728107,-0.943858356366017,-1.15589311497212E-16));
#20868=DIRECTION('center_axis',(-1.,0.,0.));
#20869=DIRECTION('ref_axis',(0.,1.,0.));
#20870=DIRECTION('',(-0.49613893835683,-0.868243142124461,-1.06329118488436E-16));
#20871=DIRECTION('center_axis',(1.,0.,0.));
#20872=DIRECTION('ref_axis',(0.,1.,0.));
#20873=DIRECTION('',(-0.70710678118654,0.707106781186555,8.65956056235503E-17));
#20874=DIRECTION('center_axis',(-1.,0.,0.));
#20875=DIRECTION('ref_axis',(0.,1.,0.));
#20876=DIRECTION('center_axis',(1.,0.,0.));
#20877=DIRECTION('ref_axis',(0.,0.,-1.));
#20878=DIRECTION('',(-0.707106781186547,-0.707106781186547,-8.65956056235493E-17));
#20879=DIRECTION('center_axis',(1.,0.,0.));
#20880=DIRECTION('ref_axis',(0.,0.,-1.));
#20881=DIRECTION('center_axis',(1.,0.,0.));
#20882=DIRECTION('ref_axis',(0.,0.,-1.));
#20883=DIRECTION('center_axis',(-1.,0.,0.));
#20884=DIRECTION('ref_axis',(0.,1.,0.));
#20885=DIRECTION('center_axis',(1.,0.,0.));
#20886=DIRECTION('ref_axis',(0.,0.,-1.));
#20887=DIRECTION('',(-0.70710678118655,-0.707106781186546,-8.65956056235491E-17));
#20888=DIRECTION('center_axis',(-1.,0.,0.));
#20889=DIRECTION('ref_axis',(0.,1.,0.));
#20890=DIRECTION('center_axis',(1.,0.,0.));
#20891=DIRECTION('ref_axis',(0.,0.,-1.));
#20892=DIRECTION('',(-0.581238193719095,-0.813733471206736,-9.96536090872394E-17));
#20893=DIRECTION('center_axis',(1.,0.,0.));
#20894=DIRECTION('ref_axis',(0.,1.,0.));
#20895=DIRECTION('center_axis',(1.,0.,0.));
#20896=DIRECTION('ref_axis',(0.,0.,-1.));
#20897=DIRECTION('',(-1.,0.,0.));
#20898=DIRECTION('center_axis',(-1.,0.,0.));
#20899=DIRECTION('ref_axis',(0.,1.,0.));
#20900=DIRECTION('center_axis',(1.,0.,0.));
#20901=DIRECTION('ref_axis',(0.,0.,-1.));
#20902=DIRECTION('',(-0.70710678118654,-0.707106781186555,-8.65956056235503E-17));
#20903=DIRECTION('center_axis',(1.,0.,0.));
#20904=DIRECTION('ref_axis',(0.,0.,-1.));
#20905=DIRECTION('center_axis',(1.,0.,0.));
#20906=DIRECTION('ref_axis',(0.,0.,-1.));
#20907=DIRECTION('center_axis',(1.,0.,0.));
#20908=DIRECTION('ref_axis',(0.,1.,0.));
#20909=DIRECTION('center_axis',(1.,0.,0.));
#20910=DIRECTION('ref_axis',(0.,0.,-1.));
#20911=DIRECTION('',(-1.,0.,0.));
#20912=DIRECTION('center_axis',(1.,0.,0.));
#20913=DIRECTION('ref_axis',(0.,1.,0.));
#20914=DIRECTION('center_axis',(1.,0.,0.));
#20915=DIRECTION('ref_axis',(0.,0.,-1.));
#20916=DIRECTION('',(-0.707106781186571,0.707106781186524,8.65956056235465E-17));
#20917=DIRECTION('center_axis',(1.,0.,0.));
#20918=DIRECTION('ref_axis',(0.,1.,0.));
#20919=DIRECTION('center_axis',(1.,0.,0.));
#20920=DIRECTION('ref_axis',(0.,0.,-1.));
#20921=DIRECTION('',(-1.,0.,0.));
#20922=DIRECTION('center_axis',(-1.,0.,0.));
#20923=DIRECTION('ref_axis',(0.,1.,0.));
#20924=DIRECTION('center_axis',(1.,0.,0.));
#20925=DIRECTION('ref_axis',(0.,0.,-1.));
#20926=DIRECTION('',(-0.316227766016807,-0.948683298050524,-1.16180196436213E-16));
#20927=DIRECTION('center_axis',(1.,0.,0.));
#20928=DIRECTION('ref_axis',(0.,1.,0.));
#20929=DIRECTION('center_axis',(1.,0.,0.));
#20930=DIRECTION('ref_axis',(0.,0.,-1.));
#20931=DIRECTION('',(-1.,0.,0.));
#20932=DIRECTION('center_axis',(1.,0.,0.));
#20933=DIRECTION('ref_axis',(0.,1.,0.));
#20934=DIRECTION('',(-0.447213595499971,0.894427190999909,1.0953573965284E-16));
#20935=DIRECTION('center_axis',(1.,0.,0.));
#20936=DIRECTION('ref_axis',(0.,0.959653292014118,-0.281185986717806));
#20937=DIRECTION('center_axis',(-1.,0.,0.));
#20938=DIRECTION('ref_axis',(0.,1.,0.));
#20939=DIRECTION('center_axis',(-1.,0.,0.));
#20940=DIRECTION('ref_axis',(0.,1.,0.));
#20941=DIRECTION('center_axis',(1.,0.,0.));
#20942=DIRECTION('ref_axis',(0.,0.,-1.));
#20943=DIRECTION('',(-0.707106781186553,-0.707106781186542,-8.65956056235487E-17));
#20944=DIRECTION('center_axis',(1.,0.,0.));
#20945=DIRECTION('ref_axis',(0.,0.,-1.));
#20946=DIRECTION('axis',(0.,0.,1.));
#20947=DIRECTION('refdir',(1.,0.,0.));
#20948=DIRECTION('center_axis',(0.,0.0210510764790368,0.999778401536597));
#20949=DIRECTION('ref_axis',(0.,-0.999778401536597,0.0210510764790368));
#20950=DIRECTION('',(1.,0.,0.));
#20951=DIRECTION('',(0.,-0.999778401536597,0.0210510764790368));
#20952=DIRECTION('',(1.,0.,0.));
#20953=DIRECTION('',(0.,-0.999778401536597,0.0210510764790368));
#20954=DIRECTION('',(1.,0.,0.));
#20955=DIRECTION('',(1.,0.,0.));
#20956=DIRECTION('center_axis',(0.,0.0210510764790365,-0.999778401536597));
#20957=DIRECTION('ref_axis',(0.,0.999778401536597,0.0210510764790365));
#20958=DIRECTION('',(0.,0.999778401536597,0.0210510764790365));
#20959=DIRECTION('',(0.,0.999778401536597,0.0210510764790365));
#20960=DIRECTION('center_axis',(1.,0.,0.));
#20961=DIRECTION('ref_axis',(0.,0.,-1.));
#20962=DIRECTION('center_axis',(1.,0.,0.));
#20963=DIRECTION('ref_axis',(0.,0.,-1.));
#20964=DIRECTION('axis',(0.,0.,1.));
#20965=DIRECTION('refdir',(1.,0.,0.));
#20966=DIRECTION('center_axis',(1.,0.,0.));
#20967=DIRECTION('ref_axis',(0.,1.,0.));
#20968=DIRECTION('center_axis',(1.,0.,0.));
#20969=DIRECTION('ref_axis',(0.,0.,-1.));
#20970=DIRECTION('',(-0.707106781186549,0.707106781186546,8.65956056235491E-17));
#20971=DIRECTION('center_axis',(1.,0.,0.));
#20972=DIRECTION('ref_axis',(0.,0.,-1.));
#20973=DIRECTION('center_axis',(1.,0.,0.));
#20974=DIRECTION('ref_axis',(0.,1.,0.));
#20975=DIRECTION('center_axis',(1.,0.,0.));
#20976=DIRECTION('ref_axis',(0.,0.,-1.));
#20977=DIRECTION('',(-1.,0.,0.));
#20978=DIRECTION('center_axis',(-1.,0.,0.));
#20979=DIRECTION('ref_axis',(0.,1.,0.));
#20980=DIRECTION('center_axis',(1.,0.,0.));
#20981=DIRECTION('ref_axis',(0.,0.,-1.));
#20982=DIRECTION('',(-0.554700196225229,-0.832050294337844,-1.01896772969045E-16));
#20983=DIRECTION('center_axis',(1.,0.,0.));
#20984=DIRECTION('ref_axis',(0.,0.,-1.));
#20985=DIRECTION('center_axis',(1.,0.,0.));
#20986=DIRECTION('ref_axis',(0.,0.,-1.));
#20987=DIRECTION('center_axis',(1.,0.,0.));
#20988=DIRECTION('ref_axis',(0.,1.,0.));
#20989=DIRECTION('',(-0.701238976116887,0.712926292385503,8.73082901997897E-17));
#20990=DIRECTION('center_axis',(1.,0.,0.));
#20991=DIRECTION('ref_axis',(0.,0.,-1.));
#20992=DIRECTION('center_axis',(1.,0.,0.));
#20993=DIRECTION('ref_axis',(0.,1.,0.));
#20994=DIRECTION('',(-1.,0.,0.));
#20995=DIRECTION('center_axis',(1.,0.,0.));
#20996=DIRECTION('ref_axis',(0.,0.,-1.));
#20997=DIRECTION('center_axis',(-1.,0.,0.));
#20998=DIRECTION('ref_axis',(0.,1.,0.));
#20999=DIRECTION('',(-0.701238976116887,-0.712926292385503,-8.73082901997896E-17));
#21000=DIRECTION('center_axis',(1.,0.,0.));
#21001=DIRECTION('ref_axis',(0.,0.,-1.));
#21002=DIRECTION('center_axis',(-1.,0.,0.));
#21003=DIRECTION('ref_axis',(0.,0.,1.));
#21004=DIRECTION('axis',(0.,0.,1.));
#21005=DIRECTION('refdir',(1.,0.,0.));
#21006=DIRECTION('center_axis',(0.707106781186548,0.,0.707106781186548));
#21007=DIRECTION('ref_axis',(0.707106781186548,0.,-0.707106781186548));
#21008=DIRECTION('',(0.707106781186548,0.,-0.707106781186548));
#21009=DIRECTION('',(0.,-1.,0.));
#21010=DIRECTION('',(-0.707106781186548,0.,0.707106781186548));
#21011=DIRECTION('',(0.,1.,0.));
#21012=DIRECTION('center_axis',(0.,0.,1.));
#21013=DIRECTION('ref_axis',(0.,-1.,0.));
#21014=DIRECTION('',(1.,0.,0.));
#21015=DIRECTION('',(0.,1.,0.));
#21016=DIRECTION('',(1.,0.,0.));
#21017=DIRECTION('center_axis',(0.,0.,1.));
#21018=DIRECTION('ref_axis',(1.,0.,0.));
#21019=DIRECTION('center_axis',(-0.707106781186548,0.,0.707106781186547));
#21020=DIRECTION('ref_axis',(0.707106781186547,0.,0.707106781186548));
#21021=DIRECTION('',(0.707106781186547,0.,0.707106781186548));
#21022=DIRECTION('',(0.,-1.,0.));
#21023=DIRECTION('',(-0.707106781186547,0.,-0.707106781186548));
#21024=DIRECTION('center_axis',(1.,0.,0.));
#21025=DIRECTION('ref_axis',(0.,0.,-1.));
#21026=DIRECTION('',(0.,0.,1.));
#21027=DIRECTION('',(0.,0.,-1.));
#21028=DIRECTION('center_axis',(1.,0.,0.));
#21029=DIRECTION('ref_axis',(0.,0.,-1.));
#21030=DIRECTION('center_axis',(-1.,0.,0.));
#21031=DIRECTION('ref_axis',(0.,0.,-1.));
#21032=DIRECTION('center_axis',(-1.,0.,0.));
#21033=DIRECTION('ref_axis',(0.,0.,-1.));
#21034=DIRECTION('center_axis',(-1.,0.,0.));
#21035=DIRECTION('ref_axis',(0.,0.,-1.));
#21036=DIRECTION('',(0.,-0.754709580222771,-0.656059028990508));
#21037=DIRECTION('',(0.,0.615661475325658,-0.788010753606722));
#21038=DIRECTION('',(0.,0.754709580222772,0.656059028990508));
#21039=DIRECTION('',(0.,0.681998360062499,0.73135370161917));
#21040=DIRECTION('',(0.,0.601815023152048,0.798635510047293));
#21041=DIRECTION('',(0.,0.515038074910053,0.857167300702113));
#21042=DIRECTION('',(0.,0.422618261740699,0.90630778703665));
#21043=DIRECTION('',(0.,0.325568154457157,0.945518575599317));
#21044=DIRECTION('',(0.,-0.961261695938319,0.275637355816999));
#21045=DIRECTION('',(0.,-0.325568154457155,-0.945518575599317));
#21046=DIRECTION('',(0.,-0.422618261740698,-0.90630778703665));
#21047=DIRECTION('',(0.,-0.515038074910055,-0.857167300702112));
#21048=DIRECTION('',(0.,-0.601815023152048,-0.798635510047293));
#21049=DIRECTION('',(0.,-0.681998360062499,-0.73135370161917));
#21050=DIRECTION('',(0.,-0.190808995376545,0.981627183447664));
#21051=DIRECTION('',(0.,-0.99026806874157,-0.139173100960066));
#21052=DIRECTION('',(0.,0.190808995376543,-0.981627183447664));
#21053=DIRECTION('',(0.,0.292371704722737,-0.956304755963035));
#21054=DIRECTION('',(0.,0.390731128489274,-0.92050485345244));
#21055=DIRECTION('',(0.,0.484809620246337,-0.874619707139396));
#21056=DIRECTION('',(0.,0.573576436351047,-0.819152044288991));
#21057=DIRECTION('',(0.,0.656059028990507,-0.754709580222772));
#21058=DIRECTION('',(0.,0.719339800338651,0.694658370458997));
#21059=DIRECTION('',(0.,-0.656059028990507,0.754709580222772));
#21060=DIRECTION('',(0.,-0.573576436351047,0.819152044288992));
#21061=DIRECTION('',(0.,-0.484809620246337,0.874619707139396));
#21062=DIRECTION('',(0.,-0.390731128489274,0.92050485345244));
#21063=DIRECTION('',(0.,-0.292371704722737,0.956304755963036));
#21064=DIRECTION('',(0.,0.754709580222772,0.656059028990507));
#21065=DIRECTION('',(0.,-0.615661475325659,0.788010753606722));
#21066=DIRECTION('',(0.,-0.754709580222772,-0.656059028990507));
#21067=DIRECTION('',(0.,-0.681998360062498,-0.731353701619171));
#21068=DIRECTION('',(0.,-0.601815023152048,-0.798635510047293));
#21069=DIRECTION('',(0.,-0.515038074910054,-0.857167300702112));
#21070=DIRECTION('',(0.,-0.4226182617407,-0.90630778703665));
#21071=DIRECTION('',(0.,-0.325568154457159,-0.945518575599316));
#21072=DIRECTION('',(0.,0.961261695938319,-0.275637355816999));
#21073=DIRECTION('',(0.,0.325568154457156,0.945518575599317));
#21074=DIRECTION('',(0.,0.422618261740699,0.90630778703665));
#21075=DIRECTION('',(0.,0.515038074910054,0.857167300702112));
#21076=DIRECTION('',(0.,0.601815023152049,0.798635510047292));
#21077=DIRECTION('',(0.,0.681998360062498,0.731353701619171));
#21078=DIRECTION('',(0.,0.945518575599317,-0.325568154457157));
#21079=DIRECTION('',(0.,0.374606593415912,0.927183854566787));
#21080=DIRECTION('',(0.,-0.945518575599316,0.325568154457158));
#21081=DIRECTION('',(0.,-0.974370064785235,0.224951054343866));
#21082=DIRECTION('',(0.,-0.992546151641322,0.121869343405146));
#21083=DIRECTION('',(0.,-0.999847695156391,0.017452406437284));
#21084=DIRECTION('',(0.,-0.996194698091745,-0.0871557427476604));
#21085=DIRECTION('',(0.,-0.981627183447664,-0.190808995376544));
#21086=DIRECTION('',(0.,0.241921895599668,-0.970295726275996));
#21087=DIRECTION('',(0.,0.981627183447664,0.190808995376545));
#21088=DIRECTION('',(0.,0.996194698091746,0.0871557427476587));
#21089=DIRECTION('',(0.,0.999847695156391,-0.0174524064372842));
#21090=DIRECTION('',(0.,0.992546151641322,-0.121869343405146));
#21091=DIRECTION('',(0.,0.974370064785235,-0.224951054343866));
#21092=DIRECTION('',(0.,0.190808995376546,-0.981627183447664));
#21093=DIRECTION('',(0.,0.99026806874157,0.139173100960065));
#21094=DIRECTION('',(0.,-0.190808995376545,0.981627183447664));
#21095=DIRECTION('',(0.,-0.292371704722736,0.956304755963036));
#21096=DIRECTION('',(0.,-0.390731128489274,0.92050485345244));
#21097=DIRECTION('',(0.,-0.484809620246338,0.874619707139396));
#21098=DIRECTION('',(0.,-0.573576436351046,0.819152044288992));
#21099=DIRECTION('',(0.,-0.656059028990507,0.754709580222772));
#21100=DIRECTION('',(0.,-0.719339800338651,-0.694658370458997));
#21101=DIRECTION('',(0.,0.656059028990507,-0.754709580222773));
#21102=DIRECTION('',(0.,0.573576436351045,-0.819152044288992));
#21103=DIRECTION('',(0.,0.484809620246337,-0.874619707139396));
#21104=DIRECTION('',(0.,0.390731128489275,-0.92050485345244));
#21105=DIRECTION('',(0.,0.292371704722736,-0.956304755963036));
#21106=DIRECTION('',(0.,-0.945518575599317,0.325568154457156));
#21107=DIRECTION('',(0.,-0.374606593415912,-0.927183854566787));
#21108=DIRECTION('',(0.,0.945518575599317,-0.325568154457156));
#21109=DIRECTION('',(0.,0.974370064785235,-0.224951054343867));
#21110=DIRECTION('',(0.,0.992546151641322,-0.121869343405148));
#21111=DIRECTION('',(0.,0.999847695156391,-0.017452406437284));
#21112=DIRECTION('',(0.,0.996194698091746,0.087155742747658));
#21113=DIRECTION('',(0.,0.981627183447664,0.190808995376544));
#21114=DIRECTION('',(0.,-0.241921895599667,0.970295726275997));
#21115=DIRECTION('',(0.,-0.981627183447664,-0.190808995376545));
#21116=DIRECTION('',(0.,-0.996194698091746,-0.0871557427476568));
#21117=DIRECTION('',(0.,-0.999847695156391,0.0174524064372842));
#21118=DIRECTION('',(0.,-0.992546151641322,0.121869343405148));
#21119=DIRECTION('',(0.,-0.974370064785235,0.224951054343865));
#21120=DIRECTION('center_axis',(-1.,0.,0.));
#21121=DIRECTION('ref_axis',(0.,0.,-1.));
#21122=DIRECTION('center_axis',(1.,0.,0.));
#21123=DIRECTION('ref_axis',(0.,0.,-1.));
#21124=DIRECTION('center_axis',(-1.,0.,0.));
#21125=DIRECTION('ref_axis',(0.,0.,-1.));
#21126=DIRECTION('center_axis',(0.,-0.591720064565827,0.806143514016092));
#21127=DIRECTION('ref_axis',(1.,0.,0.));
#21128=DIRECTION('',(-1.,0.,0.));
#21129=DIRECTION('',(1.,0.,0.));
#21130=DIRECTION('center_axis',(-1.,0.,0.));
#21131=DIRECTION('ref_axis',(0.,0.,-1.));
#21132=DIRECTION('center_axis',(1.,0.,0.));
#21133=DIRECTION('ref_axis',(0.,0.,-1.));
#21134=DIRECTION('center_axis',(-1.,0.,0.));
#21135=DIRECTION('ref_axis',(0.,0.,-1.));
#21136=DIRECTION('center_axis',(0.,0.591720064565827,0.806143514016092));
#21137=DIRECTION('ref_axis',(1.,0.,0.));
#21138=DIRECTION('',(-1.,0.,0.));
#21139=DIRECTION('',(1.,0.,0.));
#21140=DIRECTION('center_axis',(0.,1.,0.));
#21141=DIRECTION('ref_axis',(0.,0.,1.));
#21142=DIRECTION('',(0.,0.,1.));
#21143=DIRECTION('center_axis',(1.,0.,0.));
#21144=DIRECTION('ref_axis',(0.,0.,-1.));
#21145=DIRECTION('',(0.,0.,-1.));
#21146=DIRECTION('center_axis',(1.,0.,0.));
#21147=DIRECTION('ref_axis',(0.,0.,-1.));
#21148=DIRECTION('center_axis',(1.,0.,0.));
#21149=DIRECTION('ref_axis',(0.,0.,-1.));
#21150=DIRECTION('center_axis',(-1.,0.,0.));
#21151=DIRECTION('ref_axis',(0.,0.,-1.));
#21152=DIRECTION('',(0.,-0.754709580222772,-0.656059028990508));
#21153=DIRECTION('',(0.,-0.615661475325658,0.788010753606722));
#21154=DIRECTION('',(0.,0.754709580222771,0.656059028990508));
#21155=DIRECTION('',(0.,0.681998360062499,0.73135370161917));
#21156=DIRECTION('',(0.,0.601815023152048,0.798635510047293));
#21157=DIRECTION('',(0.,0.515038074910055,0.857167300702112));
#21158=DIRECTION('',(0.,0.422618261740698,0.90630778703665));
#21159=DIRECTION('',(0.,0.325568154457155,0.945518575599317));
#21160=DIRECTION('',(0.,0.961261695938319,-0.275637355816999));
#21161=DIRECTION('',(0.,-0.325568154457157,-0.945518575599317));
#21162=DIRECTION('',(0.,-0.422618261740699,-0.90630778703665));
#21163=DIRECTION('',(0.,-0.515038074910053,-0.857167300702113));
#21164=DIRECTION('',(0.,-0.601815023152048,-0.798635510047293));
#21165=DIRECTION('',(0.,-0.681998360062499,-0.73135370161917));
#21166=DIRECTION('',(0.,-0.190808995376543,0.981627183447664));
#21167=DIRECTION('',(0.,0.99026806874157,0.139173100960066));
#21168=DIRECTION('',(0.,0.190808995376545,-0.981627183447664));
#21169=DIRECTION('',(0.,0.292371704722737,-0.956304755963036));
#21170=DIRECTION('',(0.,0.390731128489274,-0.92050485345244));
#21171=DIRECTION('',(0.,0.484809620246337,-0.874619707139396));
#21172=DIRECTION('',(0.,0.573576436351047,-0.819152044288992));
#21173=DIRECTION('',(0.,0.656059028990507,-0.754709580222772));
#21174=DIRECTION('',(0.,-0.719339800338651,-0.694658370458997));
#21175=DIRECTION('',(0.,-0.656059028990507,0.754709580222772));
#21176=DIRECTION('',(0.,-0.573576436351047,0.819152044288991));
#21177=DIRECTION('',(0.,-0.484809620246337,0.874619707139396));
#21178=DIRECTION('',(0.,-0.390731128489274,0.92050485345244));
#21179=DIRECTION('',(0.,-0.292371704722737,0.956304755963035));
#21180=DIRECTION('',(0.,0.754709580222772,0.656059028990507));
#21181=DIRECTION('',(0.,0.615661475325659,-0.788010753606722));
#21182=DIRECTION('',(0.,-0.754709580222772,-0.656059028990507));
#21183=DIRECTION('',(0.,-0.681998360062498,-0.731353701619171));
#21184=DIRECTION('',(0.,-0.601815023152049,-0.798635510047292));
#21185=DIRECTION('',(0.,-0.515038074910054,-0.857167300702112));
#21186=DIRECTION('',(0.,-0.422618261740699,-0.90630778703665));
#21187=DIRECTION('',(0.,-0.325568154457156,-0.945518575599317));
#21188=DIRECTION('',(0.,-0.961261695938319,0.275637355816999));
#21189=DIRECTION('',(0.,0.325568154457159,0.945518575599316));
#21190=DIRECTION('',(0.,0.4226182617407,0.90630778703665));
#21191=DIRECTION('',(0.,0.515038074910054,0.857167300702112));
#21192=DIRECTION('',(0.,0.601815023152048,0.798635510047293));
#21193=DIRECTION('',(0.,0.681998360062498,0.731353701619171));
#21194=DIRECTION('',(0.,0.945518575599316,-0.325568154457158));
#21195=DIRECTION('',(0.,-0.374606593415912,-0.927183854566787));
#21196=DIRECTION('',(0.,-0.945518575599317,0.325568154457157));
#21197=DIRECTION('',(0.,-0.974370064785235,0.224951054343866));
#21198=DIRECTION('',(0.,-0.992546151641322,0.121869343405146));
#21199=DIRECTION('',(0.,-0.999847695156391,0.0174524064372842));
#21200=DIRECTION('',(0.,-0.996194698091746,-0.0871557427476587));
#21201=DIRECTION('',(0.,-0.981627183447664,-0.190808995376545));
#21202=DIRECTION('',(0.,-0.241921895599668,0.970295726275996));
#21203=DIRECTION('',(0.,0.981627183447664,0.190808995376544));
#21204=DIRECTION('',(0.,0.996194698091745,0.0871557427476604));
#21205=DIRECTION('',(0.,0.999847695156391,-0.017452406437284));
#21206=DIRECTION('',(0.,0.992546151641322,-0.121869343405146));
#21207=DIRECTION('',(0.,0.974370064785235,-0.224951054343866));
#21208=DIRECTION('',(0.,0.190808995376545,-0.981627183447664));
#21209=DIRECTION('',(0.,-0.99026806874157,-0.139173100960065));
#21210=DIRECTION('',(0.,-0.190808995376546,0.981627183447664));
#21211=DIRECTION('',(0.,-0.292371704722736,0.956304755963036));
#21212=DIRECTION('',(0.,-0.390731128489275,0.92050485345244));
#21213=DIRECTION('',(0.,-0.484809620246337,0.874619707139396));
#21214=DIRECTION('',(0.,-0.573576436351045,0.819152044288992));
#21215=DIRECTION('',(0.,-0.656059028990507,0.754709580222773));
#21216=DIRECTION('',(0.,0.719339800338651,0.694658370458997));
#21217=DIRECTION('',(0.,0.656059028990507,-0.754709580222772));
#21218=DIRECTION('',(0.,0.573576436351046,-0.819152044288992));
#21219=DIRECTION('',(0.,0.484809620246338,-0.874619707139396));
#21220=DIRECTION('',(0.,0.390731128489274,-0.92050485345244));
#21221=DIRECTION('',(0.,0.292371704722736,-0.956304755963036));
#21222=DIRECTION('',(0.,-0.945518575599317,0.325568154457156));
#21223=DIRECTION('',(0.,0.374606593415912,0.927183854566787));
#21224=DIRECTION('',(0.,0.945518575599317,-0.325568154457156));
#21225=DIRECTION('',(0.,0.974370064785235,-0.224951054343865));
#21226=DIRECTION('',(0.,0.992546151641322,-0.121869343405148));
#21227=DIRECTION('',(0.,0.999847695156391,-0.0174524064372842));
#21228=DIRECTION('',(0.,0.996194698091746,0.0871557427476568));
#21229=DIRECTION('',(0.,0.981627183447664,0.190808995376545));
#21230=DIRECTION('',(0.,0.241921895599667,-0.970295726275997));
#21231=DIRECTION('',(0.,-0.981627183447664,-0.190808995376544));
#21232=DIRECTION('',(0.,-0.996194698091746,-0.087155742747658));
#21233=DIRECTION('',(0.,-0.999847695156391,0.017452406437284));
#21234=DIRECTION('',(0.,-0.992546151641322,0.121869343405148));
#21235=DIRECTION('',(0.,-0.974370064785235,0.224951054343867));
#21236=DIRECTION('center_axis',(1.,0.,0.));
#21237=DIRECTION('ref_axis',(0.,0.,-1.));
#21238=DIRECTION('center_axis',(1.,0.,0.));
#21239=DIRECTION('ref_axis',(0.,0.,-1.));
#21240=DIRECTION('center_axis',(-1.,0.,0.));
#21241=DIRECTION('ref_axis',(0.,0.,-1.));
#21242=DIRECTION('',(0.707106781186547,-8.65956056235494E-17,-0.707106781186548));
#21243=DIRECTION('center_axis',(1.,0.,0.));
#21244=DIRECTION('ref_axis',(0.,0.,-1.));
#21245=DIRECTION('center_axis',(1.,0.,0.));
#21246=DIRECTION('ref_axis',(0.,0.,-1.));
#21247=DIRECTION('',(1.,0.,0.));
#21248=DIRECTION('center_axis',(-1.,0.,0.));
#21249=DIRECTION('ref_axis',(0.,0.,-1.));
#21250=DIRECTION('center_axis',(1.,0.,0.));
#21251=DIRECTION('ref_axis',(0.,0.,-1.));
#21252=DIRECTION('',(-0.707106781186548,8.65956056235493E-17,-0.707106781186548));
#21253=DIRECTION('center_axis',(-1.,0.,0.));
#21254=DIRECTION('ref_axis',(0.,0.,-1.));
#21255=DIRECTION('',(0.707106781186547,-8.65956056235494E-17,-0.707106781186548));
#21256=DIRECTION('center_axis',(1.,0.,0.));
#21257=DIRECTION('ref_axis',(0.,0.,-1.));
#21258=DIRECTION('center_axis',(1.,0.,0.));
#21259=DIRECTION('ref_axis',(0.,0.,-1.));
#21260=DIRECTION('',(1.,0.,0.));
#21261=DIRECTION('center_axis',(-1.,0.,0.));
#21262=DIRECTION('ref_axis',(0.,0.,-1.));
#21263=DIRECTION('center_axis',(1.,0.,0.));
#21264=DIRECTION('ref_axis',(0.,0.,-1.));
#21265=DIRECTION('',(-0.707106781186548,8.65956056235493E-17,-0.707106781186548));
#21266=DIRECTION('center_axis',(-1.,0.,0.));
#21267=DIRECTION('ref_axis',(0.,0.,-1.));
#21268=DIRECTION('',(0.707106781186547,-8.65956056235494E-17,-0.707106781186548));
#21269=DIRECTION('center_axis',(1.,0.,0.));
#21270=DIRECTION('ref_axis',(0.,0.,-1.));
#21271=DIRECTION('center_axis',(1.,0.,0.));
#21272=DIRECTION('ref_axis',(0.,0.,-1.));
#21273=DIRECTION('',(1.,0.,0.));
#21274=DIRECTION('center_axis',(-1.,0.,0.));
#21275=DIRECTION('ref_axis',(0.,0.,-1.));
#21276=DIRECTION('center_axis',(1.,0.,0.));
#21277=DIRECTION('ref_axis',(0.,0.,-1.));
#21278=DIRECTION('',(-0.707106781186548,8.65956056235493E-17,-0.707106781186548));
#21279=DIRECTION('center_axis',(0.,0.,1.));
#21280=DIRECTION('ref_axis',(1.,0.,0.));
#21281=DIRECTION('',(0.707106781186548,8.65956056235494E-17,-0.707106781186548));
#21282=DIRECTION('center_axis',(0.,0.,-1.));
#21283=DIRECTION('ref_axis',(1.,0.,0.));
#21284=DIRECTION('center_axis',(0.,0.,-1.));
#21285=DIRECTION('ref_axis',(1.,0.,0.));
#21286=DIRECTION('',(0.,0.,-1.));
#21287=DIRECTION('center_axis',(0.,-0.325568154457156,-0.945518575599317));
#21288=DIRECTION('ref_axis',(0.,-0.945518575599317,0.325568154457156));
#21289=DIRECTION('',(-1.,0.,0.));
#21290=DIRECTION('',(0.,-0.945518575599317,0.325568154457156));
#21291=DIRECTION('',(-1.,0.,0.));
#21292=DIRECTION('center_axis',(0.,-0.224951054343867,-0.974370064785235));
#21293=DIRECTION('ref_axis',(0.,-0.974370064785235,0.224951054343867));
#21294=DIRECTION('',(-1.,0.,0.));
#21295=DIRECTION('',(0.,-0.974370064785235,0.224951054343867));
#21296=DIRECTION('center_axis',(0.,-0.121869343405148,-0.992546151641322));
#21297=DIRECTION('ref_axis',(0.,-0.992546151641322,0.121869343405148));
#21298=DIRECTION('',(-1.,0.,0.));
#21299=DIRECTION('',(0.,-0.992546151641322,0.121869343405148));
#21300=DIRECTION('center_axis',(0.,-0.017452406437284,-0.999847695156391));
#21301=DIRECTION('ref_axis',(0.,-0.999847695156391,0.017452406437284));
#21302=DIRECTION('',(-1.,0.,0.));
#21303=DIRECTION('',(0.,-0.999847695156391,0.017452406437284));
#21304=DIRECTION('center_axis',(0.,0.087155742747658,-0.996194698091746));
#21305=DIRECTION('ref_axis',(0.,-0.996194698091746,-0.087155742747658));
#21306=DIRECTION('',(-1.,0.,0.));
#21307=DIRECTION('',(0.,-0.996194698091746,-0.087155742747658));
#21308=DIRECTION('center_axis',(0.,0.190808995376544,-0.981627183447664));
#21309=DIRECTION('ref_axis',(0.,-0.981627183447664,-0.190808995376544));
#21310=DIRECTION('',(-1.,0.,0.));
#21311=DIRECTION('',(0.,-0.981627183447664,-0.190808995376544));
#21312=DIRECTION('center_axis',(0.,0.970295726275997,0.241921895599667));
#21313=DIRECTION('ref_axis',(0.,0.241921895599667,-0.970295726275997));
#21314=DIRECTION('',(-1.,0.,0.));
#21315=DIRECTION('',(0.,0.241921895599667,-0.970295726275997));
#21316=DIRECTION('center_axis',(0.,-0.190808995376545,0.981627183447664));
#21317=DIRECTION('ref_axis',(0.,0.981627183447664,0.190808995376545));
#21318=DIRECTION('',(-1.,0.,0.));
#21319=DIRECTION('',(0.,0.981627183447664,0.190808995376545));
#21320=DIRECTION('center_axis',(0.,-0.0871557427476568,0.996194698091746));
#21321=DIRECTION('ref_axis',(0.,0.996194698091746,0.0871557427476568));
#21322=DIRECTION('',(-1.,0.,0.));
#21323=DIRECTION('',(0.,0.996194698091746,0.0871557427476568));
#21324=DIRECTION('center_axis',(0.,0.0174524064372842,0.999847695156391));
#21325=DIRECTION('ref_axis',(0.,0.999847695156391,-0.0174524064372842));
#21326=DIRECTION('',(-1.,0.,0.));
#21327=DIRECTION('',(0.,0.999847695156391,-0.0174524064372842));
#21328=DIRECTION('center_axis',(0.,0.121869343405148,0.992546151641322));
#21329=DIRECTION('ref_axis',(0.,0.992546151641322,-0.121869343405148));
#21330=DIRECTION('',(-1.,0.,0.));
#21331=DIRECTION('',(0.,0.992546151641322,-0.121869343405148));
#21332=DIRECTION('center_axis',(0.,0.224951054343865,0.974370064785235));
#21333=DIRECTION('ref_axis',(0.,0.974370064785235,-0.224951054343865));
#21334=DIRECTION('',(-1.,0.,0.));
#21335=DIRECTION('',(0.,0.974370064785235,-0.224951054343865));
#21336=DIRECTION('center_axis',(0.,0.325568154457156,0.945518575599317));
#21337=DIRECTION('ref_axis',(0.,0.945518575599317,-0.325568154457156));
#21338=DIRECTION('',(-1.,0.,0.));
#21339=DIRECTION('',(0.,0.945518575599317,-0.325568154457156));
#21340=DIRECTION('center_axis',(0.,-0.927183854566787,0.374606593415912));
#21341=DIRECTION('ref_axis',(0.,0.374606593415912,0.927183854566787));
#21342=DIRECTION('',(0.,0.374606593415912,0.927183854566787));
#21343=DIRECTION('center_axis',(-1.,0.,0.));
#21344=DIRECTION('ref_axis',(0.,0.,1.));
#21345=DIRECTION('center_axis',(0.,0.981627183447664,0.190808995376545));
#21346=DIRECTION('ref_axis',(0.,0.190808995376545,-0.981627183447664));
#21347=DIRECTION('',(-1.,0.,0.));
#21348=DIRECTION('',(0.,0.190808995376545,-0.981627183447664));
#21349=DIRECTION('',(-1.,0.,0.));
#21350=DIRECTION('center_axis',(0.,0.956304755963036,0.292371704722736));
#21351=DIRECTION('ref_axis',(0.,0.292371704722736,-0.956304755963036));
#21352=DIRECTION('',(-1.,0.,0.));
#21353=DIRECTION('',(0.,0.292371704722736,-0.956304755963036));
#21354=DIRECTION('center_axis',(0.,0.92050485345244,0.390731128489274));
#21355=DIRECTION('ref_axis',(0.,0.390731128489274,-0.92050485345244));
#21356=DIRECTION('',(-1.,0.,0.));
#21357=DIRECTION('',(0.,0.390731128489274,-0.92050485345244));
#21358=DIRECTION('center_axis',(0.,0.874619707139396,0.484809620246338));
#21359=DIRECTION('ref_axis',(0.,0.484809620246338,-0.874619707139396));
#21360=DIRECTION('',(-1.,0.,0.));
#21361=DIRECTION('',(0.,0.484809620246338,-0.874619707139396));
#21362=DIRECTION('center_axis',(0.,0.819152044288992,0.573576436351046));
#21363=DIRECTION('ref_axis',(0.,0.573576436351046,-0.819152044288992));
#21364=DIRECTION('',(-1.,0.,0.));
#21365=DIRECTION('',(0.,0.573576436351046,-0.819152044288992));
#21366=DIRECTION('center_axis',(0.,0.754709580222772,0.656059028990507));
#21367=DIRECTION('ref_axis',(0.,0.656059028990507,-0.754709580222772));
#21368=DIRECTION('',(-1.,0.,0.));
#21369=DIRECTION('',(0.,0.656059028990507,-0.754709580222772));
#21370=DIRECTION('center_axis',(0.,-0.694658370458997,0.719339800338651));
#21371=DIRECTION('ref_axis',(0.,0.719339800338651,0.694658370458997));
#21372=DIRECTION('',(-1.,0.,0.));
#21373=DIRECTION('',(0.,0.719339800338651,0.694658370458997));
#21374=DIRECTION('center_axis',(0.,-0.754709580222773,-0.656059028990507));
#21375=DIRECTION('ref_axis',(0.,-0.656059028990507,0.754709580222773));
#21376=DIRECTION('',(-1.,0.,0.));
#21377=DIRECTION('',(0.,-0.656059028990507,0.754709580222773));
#21378=DIRECTION('center_axis',(0.,-0.819152044288992,-0.573576436351045));
#21379=DIRECTION('ref_axis',(0.,-0.573576436351045,0.819152044288992));
#21380=DIRECTION('',(-1.,0.,0.));
#21381=DIRECTION('',(0.,-0.573576436351045,0.819152044288992));
#21382=DIRECTION('center_axis',(0.,-0.874619707139396,-0.484809620246337));
#21383=DIRECTION('ref_axis',(0.,-0.484809620246337,0.874619707139396));
#21384=DIRECTION('',(-1.,0.,0.));
#21385=DIRECTION('',(0.,-0.484809620246338,0.874619707139396));
#21386=DIRECTION('center_axis',(0.,-0.92050485345244,-0.390731128489275));
#21387=DIRECTION('ref_axis',(0.,-0.390731128489275,0.92050485345244));
#21388=DIRECTION('',(-1.,0.,0.));
#21389=DIRECTION('',(0.,-0.390731128489275,0.92050485345244));
#21390=DIRECTION('center_axis',(0.,-0.956304755963036,-0.292371704722736));
#21391=DIRECTION('ref_axis',(0.,-0.292371704722736,0.956304755963036));
#21392=DIRECTION('',(-1.,0.,0.));
#21393=DIRECTION('',(0.,-0.292371704722736,0.956304755963036));
#21394=DIRECTION('center_axis',(0.,-0.981627183447664,-0.190808995376546));
#21395=DIRECTION('ref_axis',(0.,-0.190808995376546,0.981627183447664));
#21396=DIRECTION('',(-1.,0.,0.));
#21397=DIRECTION('',(0.,-0.190808995376546,0.981627183447664));
#21398=DIRECTION('center_axis',(0.,0.139173100960065,-0.99026806874157));
#21399=DIRECTION('ref_axis',(0.,-0.99026806874157,-0.139173100960065));
#21400=DIRECTION('',(0.,-0.99026806874157,-0.139173100960065));
#21401=DIRECTION('center_axis',(-1.,0.,0.));
#21402=DIRECTION('ref_axis',(0.,0.,1.));
#21403=DIRECTION('center_axis',(0.,0.325568154457158,0.945518575599316));
#21404=DIRECTION('ref_axis',(0.,0.945518575599316,-0.325568154457158));
#21405=DIRECTION('',(-1.,0.,0.));
#21406=DIRECTION('',(0.,0.945518575599316,-0.325568154457158));
#21407=DIRECTION('',(-1.,0.,0.));
#21408=DIRECTION('center_axis',(0.,0.224951054343866,0.974370064785235));
#21409=DIRECTION('ref_axis',(0.,0.974370064785235,-0.224951054343866));
#21410=DIRECTION('',(-1.,0.,0.));
#21411=DIRECTION('',(0.,0.974370064785235,-0.224951054343866));
#21412=DIRECTION('center_axis',(0.,0.121869343405146,0.992546151641322));
#21413=DIRECTION('ref_axis',(0.,0.992546151641322,-0.121869343405146));
#21414=DIRECTION('',(-1.,0.,0.));
#21415=DIRECTION('',(0.,0.992546151641322,-0.121869343405145));
#21416=DIRECTION('center_axis',(0.,0.017452406437284,0.999847695156391));
#21417=DIRECTION('ref_axis',(0.,0.999847695156391,-0.017452406437284));
#21418=DIRECTION('',(-1.,0.,0.));
#21419=DIRECTION('',(0.,0.999847695156391,-0.017452406437284));
#21420=DIRECTION('center_axis',(0.,-0.0871557427476604,0.996194698091745));
#21421=DIRECTION('ref_axis',(0.,0.996194698091745,0.0871557427476604));
#21422=DIRECTION('',(-1.,0.,0.));
#21423=DIRECTION('',(0.,0.996194698091745,0.0871557427476604));
#21424=DIRECTION('center_axis',(0.,-0.190808995376544,0.981627183447664));
#21425=DIRECTION('ref_axis',(0.,0.981627183447664,0.190808995376544));
#21426=DIRECTION('',(-1.,0.,0.));
#21427=DIRECTION('',(0.,0.981627183447664,0.190808995376544));
#21428=DIRECTION('center_axis',(0.,-0.970295726275996,-0.241921895599668));
#21429=DIRECTION('ref_axis',(0.,-0.241921895599668,0.970295726275996));
#21430=DIRECTION('',(-1.,0.,0.));
#21431=DIRECTION('',(0.,-0.241921895599668,0.970295726275996));
#21432=DIRECTION('center_axis',(0.,0.190808995376545,-0.981627183447664));
#21433=DIRECTION('ref_axis',(0.,-0.981627183447664,-0.190808995376545));
#21434=DIRECTION('',(-1.,0.,0.));
#21435=DIRECTION('',(0.,-0.981627183447664,-0.190808995376545));
#21436=DIRECTION('center_axis',(0.,0.0871557427476587,-0.996194698091746));
#21437=DIRECTION('ref_axis',(0.,-0.996194698091746,-0.0871557427476587));
#21438=DIRECTION('',(-1.,0.,0.));
#21439=DIRECTION('',(0.,-0.996194698091746,-0.0871557427476587));
#21440=DIRECTION('center_axis',(0.,-0.0174524064372842,-0.999847695156391));
#21441=DIRECTION('ref_axis',(0.,-0.999847695156391,0.0174524064372842));
#21442=DIRECTION('',(-1.,0.,0.));
#21443=DIRECTION('',(0.,-0.999847695156391,0.0174524064372842));
#21444=DIRECTION('center_axis',(0.,-0.121869343405146,-0.992546151641322));
#21445=DIRECTION('ref_axis',(0.,-0.992546151641322,0.121869343405146));
#21446=DIRECTION('',(-1.,0.,0.));
#21447=DIRECTION('',(0.,-0.992546151641322,0.121869343405146));
#21448=DIRECTION('center_axis',(0.,-0.224951054343866,-0.974370064785235));
#21449=DIRECTION('ref_axis',(0.,-0.974370064785235,0.224951054343866));
#21450=DIRECTION('',(-1.,0.,0.));
#21451=DIRECTION('',(0.,-0.974370064785235,0.224951054343866));
#21452=DIRECTION('center_axis',(0.,-0.325568154457157,-0.945518575599317));
#21453=DIRECTION('ref_axis',(0.,-0.945518575599317,0.325568154457157));
#21454=DIRECTION('',(-1.,0.,0.));
#21455=DIRECTION('',(0.,-0.945518575599317,0.325568154457157));
#21456=DIRECTION('center_axis',(0.,0.927183854566787,-0.374606593415912));
#21457=DIRECTION('ref_axis',(0.,-0.374606593415912,-0.927183854566787));
#21458=DIRECTION('',(0.,-0.374606593415912,-0.927183854566787));
#21459=DIRECTION('center_axis',(-1.,0.,0.));
#21460=DIRECTION('ref_axis',(0.,0.,1.));
#21461=DIRECTION('center_axis',(0.,-0.656059028990507,0.754709580222772));
#21462=DIRECTION('ref_axis',(0.,0.754709580222772,0.656059028990507));
#21463=DIRECTION('',(-1.,0.,0.));
#21464=DIRECTION('',(0.,0.754709580222772,0.656059028990507));
#21465=DIRECTION('',(-1.,0.,0.));
#21466=DIRECTION('center_axis',(0.,-0.731353701619171,0.681998360062498));
#21467=DIRECTION('ref_axis',(0.,0.681998360062498,0.731353701619171));
#21468=DIRECTION('',(-1.,0.,0.));
#21469=DIRECTION('',(0.,0.681998360062498,0.731353701619171));
#21470=DIRECTION('center_axis',(0.,-0.798635510047293,0.601815023152048));
#21471=DIRECTION('ref_axis',(0.,0.601815023152048,0.798635510047293));
#21472=DIRECTION('',(-1.,0.,0.));
#21473=DIRECTION('',(0.,0.601815023152048,0.798635510047293));
#21474=DIRECTION('center_axis',(0.,-0.857167300702112,0.515038074910054));
#21475=DIRECTION('ref_axis',(0.,0.515038074910054,0.857167300702112));
#21476=DIRECTION('',(-1.,0.,0.));
#21477=DIRECTION('',(0.,0.515038074910054,0.857167300702112));
#21478=DIRECTION('center_axis',(0.,-0.90630778703665,0.4226182617407));
#21479=DIRECTION('ref_axis',(0.,0.4226182617407,0.90630778703665));
#21480=DIRECTION('',(-1.,0.,0.));
#21481=DIRECTION('',(0.,0.4226182617407,0.90630778703665));
#21482=DIRECTION('center_axis',(0.,-0.945518575599316,0.325568154457159));
#21483=DIRECTION('ref_axis',(0.,0.325568154457159,0.945518575599316));
#21484=DIRECTION('',(-1.,0.,0.));
#21485=DIRECTION('',(0.,0.325568154457159,0.945518575599316));
#21486=DIRECTION('center_axis',(0.,-0.275637355816999,-0.961261695938319));
#21487=DIRECTION('ref_axis',(0.,-0.961261695938319,0.275637355816999));
#21488=DIRECTION('',(-1.,0.,0.));
#21489=DIRECTION('',(0.,-0.961261695938319,0.275637355816999));
#21490=DIRECTION('center_axis',(0.,0.945518575599317,-0.325568154457157));
#21491=DIRECTION('ref_axis',(0.,-0.325568154457156,-0.945518575599317));
#21492=DIRECTION('',(-1.,0.,0.));
#21493=DIRECTION('',(0.,-0.325568154457156,-0.945518575599317));
#21494=DIRECTION('center_axis',(0.,0.90630778703665,-0.422618261740699));
#21495=DIRECTION('ref_axis',(0.,-0.422618261740699,-0.90630778703665));
#21496=DIRECTION('',(-1.,0.,0.));
#21497=DIRECTION('',(0.,-0.422618261740699,-0.90630778703665));
#21498=DIRECTION('center_axis',(0.,0.857167300702112,-0.515038074910054));
#21499=DIRECTION('ref_axis',(0.,-0.515038074910054,-0.857167300702112));
#21500=DIRECTION('',(-1.,0.,0.));
#21501=DIRECTION('',(0.,-0.515038074910054,-0.857167300702112));
#21502=DIRECTION('center_axis',(0.,0.798635510047292,-0.601815023152049));
#21503=DIRECTION('ref_axis',(0.,-0.601815023152049,-0.798635510047292));
#21504=DIRECTION('',(-1.,0.,0.));
#21505=DIRECTION('',(0.,-0.601815023152049,-0.798635510047292));
#21506=DIRECTION('center_axis',(0.,0.731353701619171,-0.681998360062498));
#21507=DIRECTION('ref_axis',(0.,-0.681998360062498,-0.731353701619171));
#21508=DIRECTION('',(-1.,0.,0.));
#21509=DIRECTION('',(0.,-0.681998360062498,-0.731353701619171));
#21510=DIRECTION('center_axis',(0.,0.656059028990507,-0.754709580222772));
#21511=DIRECTION('ref_axis',(0.,-0.754709580222772,-0.656059028990507));
#21512=DIRECTION('',(-1.,0.,0.));
#21513=DIRECTION('',(0.,-0.754709580222772,-0.656059028990507));
#21514=DIRECTION('center_axis',(0.,0.788010753606722,0.615661475325659));
#21515=DIRECTION('ref_axis',(0.,0.615661475325659,-0.788010753606722));
#21516=DIRECTION('',(0.,0.615661475325659,-0.788010753606722));
#21517=DIRECTION('center_axis',(-1.,0.,0.));
#21518=DIRECTION('ref_axis',(0.,0.,1.));
#21519=DIRECTION('center_axis',(0.,-0.981627183447664,-0.190808995376543));
#21520=DIRECTION('ref_axis',(0.,-0.190808995376543,0.981627183447664));
#21521=DIRECTION('',(-1.,0.,0.));
#21522=DIRECTION('',(0.,-0.190808995376543,0.981627183447664));
#21523=DIRECTION('',(-1.,0.,0.));
#21524=DIRECTION('center_axis',(0.,-0.956304755963035,-0.292371704722737));
#21525=DIRECTION('ref_axis',(0.,-0.292371704722737,0.956304755963035));
#21526=DIRECTION('',(-1.,0.,0.));
#21527=DIRECTION('',(0.,-0.292371704722737,0.956304755963035));
#21528=DIRECTION('center_axis',(0.,-0.92050485345244,-0.390731128489274));
#21529=DIRECTION('ref_axis',(0.,-0.390731128489274,0.92050485345244));
#21530=DIRECTION('',(-1.,0.,0.));
#21531=DIRECTION('',(0.,-0.390731128489274,0.92050485345244));
#21532=DIRECTION('center_axis',(0.,-0.874619707139396,-0.484809620246337));
#21533=DIRECTION('ref_axis',(0.,-0.484809620246337,0.874619707139396));
#21534=DIRECTION('',(-1.,0.,0.));
#21535=DIRECTION('',(0.,-0.484809620246337,0.874619707139396));
#21536=DIRECTION('center_axis',(0.,-0.819152044288991,-0.573576436351047));
#21537=DIRECTION('ref_axis',(0.,-0.573576436351047,0.819152044288991));
#21538=DIRECTION('',(-1.,0.,0.));
#21539=DIRECTION('',(0.,-0.573576436351047,0.819152044288991));
#21540=DIRECTION('center_axis',(0.,-0.754709580222772,-0.656059028990507));
#21541=DIRECTION('ref_axis',(0.,-0.656059028990507,0.754709580222772));
#21542=DIRECTION('',(-1.,0.,0.));
#21543=DIRECTION('',(0.,-0.656059028990507,0.754709580222772));
#21544=DIRECTION('center_axis',(0.,0.694658370458997,-0.719339800338651));
#21545=DIRECTION('ref_axis',(0.,-0.719339800338651,-0.694658370458997));
#21546=DIRECTION('',(-1.,0.,0.));
#21547=DIRECTION('',(0.,-0.719339800338651,-0.694658370458997));
#21548=DIRECTION('center_axis',(0.,0.754709580222772,0.656059028990507));
#21549=DIRECTION('ref_axis',(0.,0.656059028990507,-0.754709580222772));
#21550=DIRECTION('',(-1.,0.,0.));
#21551=DIRECTION('',(0.,0.656059028990507,-0.754709580222772));
#21552=DIRECTION('center_axis',(0.,0.819152044288992,0.573576436351047));
#21553=DIRECTION('ref_axis',(0.,0.573576436351047,-0.819152044288992));
#21554=DIRECTION('',(-1.,0.,0.));
#21555=DIRECTION('',(0.,0.573576436351047,-0.819152044288992));
#21556=DIRECTION('center_axis',(0.,0.874619707139396,0.484809620246337));
#21557=DIRECTION('ref_axis',(0.,0.484809620246337,-0.874619707139396));
#21558=DIRECTION('',(-1.,0.,0.));
#21559=DIRECTION('',(0.,0.484809620246337,-0.874619707139396));
#21560=DIRECTION('center_axis',(0.,0.92050485345244,0.390731128489274));
#21561=DIRECTION('ref_axis',(0.,0.390731128489274,-0.92050485345244));
#21562=DIRECTION('',(-1.,0.,0.));
#21563=DIRECTION('',(0.,0.390731128489274,-0.92050485345244));
#21564=DIRECTION('center_axis',(0.,0.956304755963036,0.292371704722737));
#21565=DIRECTION('ref_axis',(0.,0.292371704722737,-0.956304755963036));
#21566=DIRECTION('',(-1.,0.,0.));
#21567=DIRECTION('',(0.,0.292371704722737,-0.956304755963036));
#21568=DIRECTION('center_axis',(0.,0.981627183447664,0.190808995376545));
#21569=DIRECTION('ref_axis',(0.,0.190808995376545,-0.981627183447664));
#21570=DIRECTION('',(-1.,0.,0.));
#21571=DIRECTION('',(0.,0.190808995376545,-0.981627183447664));
#21572=DIRECTION('center_axis',(0.,-0.139173100960066,0.99026806874157));
#21573=DIRECTION('ref_axis',(0.,0.99026806874157,0.139173100960066));
#21574=DIRECTION('',(0.,0.99026806874157,0.139173100960066));
#21575=DIRECTION('center_axis',(-1.,0.,0.));
#21576=DIRECTION('ref_axis',(0.,0.,1.));
#21577=DIRECTION('center_axis',(0.,0.656059028990508,-0.754709580222772));
#21578=DIRECTION('ref_axis',(0.,-0.754709580222772,-0.656059028990508));
#21579=DIRECTION('',(-1.,0.,0.));
#21580=DIRECTION('',(0.,-0.754709580222772,-0.656059028990508));
#21581=DIRECTION('',(-1.,0.,0.));
#21582=DIRECTION('center_axis',(0.,0.73135370161917,-0.681998360062499));
#21583=DIRECTION('ref_axis',(0.,-0.681998360062499,-0.73135370161917));
#21584=DIRECTION('',(-1.,0.,0.));
#21585=DIRECTION('',(0.,-0.681998360062499,-0.73135370161917));
#21586=DIRECTION('center_axis',(0.,0.798635510047293,-0.601815023152048));
#21587=DIRECTION('ref_axis',(0.,-0.601815023152048,-0.798635510047293));
#21588=DIRECTION('',(-1.,0.,0.));
#21589=DIRECTION('',(0.,-0.601815023152048,-0.798635510047293));
#21590=DIRECTION('center_axis',(0.,0.857167300702113,-0.515038074910053));
#21591=DIRECTION('ref_axis',(0.,-0.515038074910053,-0.857167300702113));
#21592=DIRECTION('',(-1.,0.,0.));
#21593=DIRECTION('',(0.,-0.515038074910053,-0.857167300702113));
#21594=DIRECTION('center_axis',(0.,0.90630778703665,-0.422618261740699));
#21595=DIRECTION('ref_axis',(0.,-0.422618261740699,-0.90630778703665));
#21596=DIRECTION('',(-1.,0.,0.));
#21597=DIRECTION('',(0.,-0.422618261740699,-0.90630778703665));
#21598=DIRECTION('center_axis',(0.,0.945518575599317,-0.325568154457157));
#21599=DIRECTION('ref_axis',(0.,-0.325568154457157,-0.945518575599317));
#21600=DIRECTION('',(-1.,0.,0.));
#21601=DIRECTION('',(0.,-0.325568154457157,-0.945518575599317));
#21602=DIRECTION('center_axis',(0.,0.275637355816999,0.961261695938319));
#21603=DIRECTION('ref_axis',(0.,0.961261695938319,-0.275637355816999));
#21604=DIRECTION('',(-1.,0.,0.));
#21605=DIRECTION('',(0.,0.961261695938319,-0.275637355816999));
#21606=DIRECTION('center_axis',(0.,-0.945518575599317,0.325568154457155));
#21607=DIRECTION('ref_axis',(0.,0.325568154457155,0.945518575599317));
#21608=DIRECTION('',(-1.,0.,0.));
#21609=DIRECTION('',(0.,0.325568154457155,0.945518575599317));
#21610=DIRECTION('center_axis',(0.,-0.90630778703665,0.422618261740698));
#21611=DIRECTION('ref_axis',(0.,0.422618261740698,0.90630778703665));
#21612=DIRECTION('',(-1.,0.,0.));
#21613=DIRECTION('',(0.,0.422618261740698,0.90630778703665));
#21614=DIRECTION('center_axis',(0.,-0.857167300702112,0.515038074910055));
#21615=DIRECTION('ref_axis',(0.,0.515038074910055,0.857167300702112));
#21616=DIRECTION('',(-1.,0.,0.));
#21617=DIRECTION('',(0.,0.515038074910055,0.857167300702112));
#21618=DIRECTION('center_axis',(0.,-0.798635510047293,0.601815023152048));
#21619=DIRECTION('ref_axis',(0.,0.601815023152048,0.798635510047293));
#21620=DIRECTION('',(-1.,0.,0.));
#21621=DIRECTION('',(0.,0.601815023152048,0.798635510047293));
#21622=DIRECTION('center_axis',(0.,-0.73135370161917,0.681998360062499));
#21623=DIRECTION('ref_axis',(0.,0.681998360062499,0.73135370161917));
#21624=DIRECTION('',(-1.,0.,0.));
#21625=DIRECTION('',(0.,0.681998360062499,0.73135370161917));
#21626=DIRECTION('center_axis',(0.,-0.656059028990508,0.754709580222771));
#21627=DIRECTION('ref_axis',(0.,0.754709580222771,0.656059028990508));
#21628=DIRECTION('',(-1.,0.,0.));
#21629=DIRECTION('',(0.,0.754709580222771,0.656059028990508));
#21630=DIRECTION('center_axis',(0.,-0.788010753606722,-0.615661475325659));
#21631=DIRECTION('ref_axis',(0.,-0.615661475325658,0.788010753606722));
#21632=DIRECTION('',(0.,-0.615661475325658,0.788010753606722));
#21633=DIRECTION('center_axis',(-1.,0.,0.));
#21634=DIRECTION('ref_axis',(0.,0.,1.));
#21635=DIRECTION('center_axis',(0.,0.325568154457156,0.945518575599317));
#21636=DIRECTION('ref_axis',(0.,-0.945518575599317,0.325568154457156));
#21637=DIRECTION('',(1.,0.,0.));
#21638=DIRECTION('',(0.,-0.945518575599317,0.325568154457156));
#21639=DIRECTION('',(1.,0.,0.));
#21640=DIRECTION('center_axis',(0.,0.224951054343865,0.974370064785235));
#21641=DIRECTION('ref_axis',(0.,-0.974370064785235,0.224951054343865));
#21642=DIRECTION('',(1.,0.,0.));
#21643=DIRECTION('',(0.,-0.974370064785235,0.224951054343865));
#21644=DIRECTION('center_axis',(0.,0.121869343405148,0.992546151641322));
#21645=DIRECTION('ref_axis',(0.,-0.992546151641322,0.121869343405148));
#21646=DIRECTION('',(1.,0.,0.));
#21647=DIRECTION('',(0.,-0.992546151641322,0.121869343405148));
#21648=DIRECTION('center_axis',(0.,0.0174524064372842,0.999847695156391));
#21649=DIRECTION('ref_axis',(0.,-0.999847695156391,0.0174524064372842));
#21650=DIRECTION('',(1.,0.,0.));
#21651=DIRECTION('',(0.,-0.999847695156391,0.0174524064372842));
#21652=DIRECTION('center_axis',(0.,-0.0871557427476568,0.996194698091746));
#21653=DIRECTION('ref_axis',(0.,-0.996194698091746,-0.0871557427476568));
#21654=DIRECTION('',(1.,0.,0.));
#21655=DIRECTION('',(0.,-0.996194698091746,-0.0871557427476568));
#21656=DIRECTION('center_axis',(0.,-0.190808995376545,0.981627183447664));
#21657=DIRECTION('ref_axis',(0.,-0.981627183447664,-0.190808995376545));
#21658=DIRECTION('',(1.,0.,0.));
#21659=DIRECTION('',(0.,-0.981627183447664,-0.190808995376545));
#21660=DIRECTION('center_axis',(0.,0.970295726275997,0.241921895599667));
#21661=DIRECTION('ref_axis',(0.,-0.241921895599667,0.970295726275997));
#21662=DIRECTION('',(1.,0.,0.));
#21663=DIRECTION('',(0.,-0.241921895599667,0.970295726275997));
#21664=DIRECTION('center_axis',(0.,0.190808995376544,-0.981627183447664));
#21665=DIRECTION('ref_axis',(0.,0.981627183447664,0.190808995376544));
#21666=DIRECTION('',(1.,0.,0.));
#21667=DIRECTION('',(0.,0.981627183447664,0.190808995376544));
#21668=DIRECTION('center_axis',(0.,0.087155742747658,-0.996194698091746));
#21669=DIRECTION('ref_axis',(0.,0.996194698091746,0.087155742747658));
#21670=DIRECTION('',(1.,0.,0.));
#21671=DIRECTION('',(0.,0.996194698091746,0.087155742747658));
#21672=DIRECTION('center_axis',(0.,-0.017452406437284,-0.999847695156391));
#21673=DIRECTION('ref_axis',(0.,0.999847695156391,-0.017452406437284));
#21674=DIRECTION('',(1.,0.,0.));
#21675=DIRECTION('',(0.,0.999847695156391,-0.017452406437284));
#21676=DIRECTION('center_axis',(0.,-0.121869343405148,-0.992546151641322));
#21677=DIRECTION('ref_axis',(0.,0.992546151641322,-0.121869343405148));
#21678=DIRECTION('',(1.,0.,0.));
#21679=DIRECTION('',(0.,0.992546151641322,-0.121869343405148));
#21680=DIRECTION('center_axis',(0.,-0.224951054343867,-0.974370064785235));
#21681=DIRECTION('ref_axis',(0.,0.974370064785235,-0.224951054343867));
#21682=DIRECTION('',(1.,0.,0.));
#21683=DIRECTION('',(0.,0.974370064785235,-0.224951054343867));
#21684=DIRECTION('center_axis',(0.,-0.325568154457156,-0.945518575599317));
#21685=DIRECTION('ref_axis',(0.,0.945518575599317,-0.325568154457156));
#21686=DIRECTION('',(1.,0.,0.));
#21687=DIRECTION('',(0.,0.945518575599317,-0.325568154457156));
#21688=DIRECTION('center_axis',(0.,-0.927183854566787,0.374606593415912));
#21689=DIRECTION('ref_axis',(0.,-0.374606593415912,-0.927183854566787));
#21690=DIRECTION('',(0.,-0.374606593415912,-0.927183854566787));
#21691=DIRECTION('center_axis',(1.,0.,0.));
#21692=DIRECTION('ref_axis',(0.,0.,-1.));
#21693=DIRECTION('center_axis',(0.,-0.981627183447664,-0.190808995376546));
#21694=DIRECTION('ref_axis',(0.,0.190808995376546,-0.981627183447664));
#21695=DIRECTION('',(1.,0.,0.));
#21696=DIRECTION('',(0.,0.190808995376546,-0.981627183447664));
#21697=DIRECTION('',(1.,0.,0.));
#21698=DIRECTION('center_axis',(0.,-0.956304755963036,-0.292371704722736));
#21699=DIRECTION('ref_axis',(0.,0.292371704722736,-0.956304755963036));
#21700=DIRECTION('',(1.,0.,0.));
#21701=DIRECTION('',(0.,0.292371704722736,-0.956304755963036));
#21702=DIRECTION('center_axis',(0.,-0.92050485345244,-0.390731128489275));
#21703=DIRECTION('ref_axis',(0.,0.390731128489275,-0.92050485345244));
#21704=DIRECTION('',(1.,0.,0.));
#21705=DIRECTION('',(0.,0.390731128489275,-0.92050485345244));
#21706=DIRECTION('center_axis',(0.,-0.874619707139396,-0.484809620246337));
#21707=DIRECTION('ref_axis',(0.,0.484809620246337,-0.874619707139396));
#21708=DIRECTION('',(1.,0.,0.));
#21709=DIRECTION('',(0.,0.484809620246338,-0.874619707139396));
#21710=DIRECTION('center_axis',(0.,-0.819152044288992,-0.573576436351045));
#21711=DIRECTION('ref_axis',(0.,0.573576436351045,-0.819152044288992));
#21712=DIRECTION('',(1.,0.,0.));
#21713=DIRECTION('',(0.,0.573576436351045,-0.819152044288992));
#21714=DIRECTION('center_axis',(0.,-0.754709580222773,-0.656059028990507));
#21715=DIRECTION('ref_axis',(0.,0.656059028990507,-0.754709580222773));
#21716=DIRECTION('',(1.,0.,0.));
#21717=DIRECTION('',(0.,0.656059028990507,-0.754709580222773));
#21718=DIRECTION('center_axis',(0.,-0.694658370458997,0.719339800338651));
#21719=DIRECTION('ref_axis',(0.,-0.719339800338651,-0.694658370458997));
#21720=DIRECTION('',(1.,0.,0.));
#21721=DIRECTION('',(0.,-0.719339800338651,-0.694658370458997));
#21722=DIRECTION('center_axis',(0.,0.754709580222772,0.656059028990507));
#21723=DIRECTION('ref_axis',(0.,-0.656059028990507,0.754709580222772));
#21724=DIRECTION('',(1.,0.,0.));
#21725=DIRECTION('',(0.,-0.656059028990507,0.754709580222772));
#21726=DIRECTION('center_axis',(0.,0.819152044288992,0.573576436351046));
#21727=DIRECTION('ref_axis',(0.,-0.573576436351046,0.819152044288992));
#21728=DIRECTION('',(1.,0.,0.));
#21729=DIRECTION('',(0.,-0.573576436351046,0.819152044288992));
#21730=DIRECTION('center_axis',(0.,0.874619707139396,0.484809620246338));
#21731=DIRECTION('ref_axis',(0.,-0.484809620246338,0.874619707139396));
#21732=DIRECTION('',(1.,0.,0.));
#21733=DIRECTION('',(0.,-0.484809620246338,0.874619707139396));
#21734=DIRECTION('center_axis',(0.,0.92050485345244,0.390731128489274));
#21735=DIRECTION('ref_axis',(0.,-0.390731128489274,0.92050485345244));
#21736=DIRECTION('',(1.,0.,0.));
#21737=DIRECTION('',(0.,-0.390731128489274,0.92050485345244));
#21738=DIRECTION('center_axis',(0.,0.956304755963036,0.292371704722736));
#21739=DIRECTION('ref_axis',(0.,-0.292371704722736,0.956304755963036));
#21740=DIRECTION('',(1.,0.,0.));
#21741=DIRECTION('',(0.,-0.292371704722736,0.956304755963036));
#21742=DIRECTION('center_axis',(0.,0.981627183447664,0.190808995376545));
#21743=DIRECTION('ref_axis',(0.,-0.190808995376545,0.981627183447664));
#21744=DIRECTION('',(1.,0.,0.));
#21745=DIRECTION('',(0.,-0.190808995376545,0.981627183447664));
#21746=DIRECTION('center_axis',(0.,0.139173100960065,-0.99026806874157));
#21747=DIRECTION('ref_axis',(0.,0.99026806874157,0.139173100960065));
#21748=DIRECTION('',(0.,0.99026806874157,0.139173100960065));
#21749=DIRECTION('center_axis',(1.,0.,0.));
#21750=DIRECTION('ref_axis',(0.,0.,-1.));
#21751=DIRECTION('center_axis',(0.,-0.325568154457157,-0.945518575599317));
#21752=DIRECTION('ref_axis',(0.,0.945518575599317,-0.325568154457157));
#21753=DIRECTION('',(1.,0.,0.));
#21754=DIRECTION('',(0.,0.945518575599317,-0.325568154457157));
#21755=DIRECTION('',(1.,0.,0.));
#21756=DIRECTION('center_axis',(0.,-0.224951054343866,-0.974370064785235));
#21757=DIRECTION('ref_axis',(0.,0.974370064785235,-0.224951054343866));
#21758=DIRECTION('',(1.,0.,0.));
#21759=DIRECTION('',(0.,0.974370064785235,-0.224951054343866));
#21760=DIRECTION('center_axis',(0.,-0.121869343405146,-0.992546151641322));
#21761=DIRECTION('ref_axis',(0.,0.992546151641322,-0.121869343405146));
#21762=DIRECTION('',(1.,0.,0.));
#21763=DIRECTION('',(0.,0.992546151641322,-0.121869343405146));
#21764=DIRECTION('center_axis',(0.,-0.0174524064372842,-0.999847695156391));
#21765=DIRECTION('ref_axis',(0.,0.999847695156391,-0.0174524064372842));
#21766=DIRECTION('',(1.,0.,0.));
#21767=DIRECTION('',(0.,0.999847695156391,-0.0174524064372842));
#21768=DIRECTION('center_axis',(0.,0.0871557427476587,-0.996194698091746));
#21769=DIRECTION('ref_axis',(0.,0.996194698091746,0.0871557427476587));
#21770=DIRECTION('',(1.,0.,0.));
#21771=DIRECTION('',(0.,0.996194698091746,0.0871557427476587));
#21772=DIRECTION('center_axis',(0.,0.190808995376545,-0.981627183447664));
#21773=DIRECTION('ref_axis',(0.,0.981627183447664,0.190808995376545));
#21774=DIRECTION('',(1.,0.,0.));
#21775=DIRECTION('',(0.,0.981627183447664,0.190808995376545));
#21776=DIRECTION('center_axis',(0.,-0.970295726275996,-0.241921895599668));
#21777=DIRECTION('ref_axis',(0.,0.241921895599668,-0.970295726275996));
#21778=DIRECTION('',(1.,0.,0.));
#21779=DIRECTION('',(0.,0.241921895599668,-0.970295726275996));
#21780=DIRECTION('center_axis',(0.,-0.190808995376544,0.981627183447664));
#21781=DIRECTION('ref_axis',(0.,-0.981627183447664,-0.190808995376544));
#21782=DIRECTION('',(1.,0.,0.));
#21783=DIRECTION('',(0.,-0.981627183447664,-0.190808995376544));
#21784=DIRECTION('center_axis',(0.,-0.0871557427476604,0.996194698091745));
#21785=DIRECTION('ref_axis',(0.,-0.996194698091745,-0.0871557427476604));
#21786=DIRECTION('',(1.,0.,0.));
#21787=DIRECTION('',(0.,-0.996194698091745,-0.0871557427476604));
#21788=DIRECTION('center_axis',(0.,0.017452406437284,0.999847695156391));
#21789=DIRECTION('ref_axis',(0.,-0.999847695156391,0.017452406437284));
#21790=DIRECTION('',(1.,0.,0.));
#21791=DIRECTION('',(0.,-0.999847695156391,0.017452406437284));
#21792=DIRECTION('center_axis',(0.,0.121869343405146,0.992546151641322));
#21793=DIRECTION('ref_axis',(0.,-0.992546151641322,0.121869343405146));
#21794=DIRECTION('',(1.,0.,0.));
#21795=DIRECTION('',(0.,-0.992546151641322,0.121869343405145));
#21796=DIRECTION('center_axis',(0.,0.224951054343866,0.974370064785235));
#21797=DIRECTION('ref_axis',(0.,-0.974370064785235,0.224951054343866));
#21798=DIRECTION('',(1.,0.,0.));
#21799=DIRECTION('',(0.,-0.974370064785235,0.224951054343866));
#21800=DIRECTION('center_axis',(0.,0.325568154457158,0.945518575599316));
#21801=DIRECTION('ref_axis',(0.,-0.945518575599316,0.325568154457158));
#21802=DIRECTION('',(1.,0.,0.));
#21803=DIRECTION('',(0.,-0.945518575599316,0.325568154457158));
#21804=DIRECTION('center_axis',(0.,0.927183854566787,-0.374606593415912));
#21805=DIRECTION('ref_axis',(0.,0.374606593415912,0.927183854566787));
#21806=DIRECTION('',(0.,0.374606593415912,0.927183854566787));
#21807=DIRECTION('center_axis',(1.,0.,0.));
#21808=DIRECTION('ref_axis',(0.,0.,-1.));
#21809=DIRECTION('center_axis',(0.,0.656059028990507,-0.754709580222772));
#21810=DIRECTION('ref_axis',(0.,0.754709580222772,0.656059028990507));
#21811=DIRECTION('',(1.,0.,0.));
#21812=DIRECTION('',(0.,0.754709580222772,0.656059028990507));
#21813=DIRECTION('',(1.,0.,0.));
#21814=DIRECTION('center_axis',(0.,0.731353701619171,-0.681998360062498));
#21815=DIRECTION('ref_axis',(0.,0.681998360062498,0.731353701619171));
#21816=DIRECTION('',(1.,0.,0.));
#21817=DIRECTION('',(0.,0.681998360062498,0.731353701619171));
#21818=DIRECTION('center_axis',(0.,0.798635510047292,-0.601815023152049));
#21819=DIRECTION('ref_axis',(0.,0.601815023152049,0.798635510047292));
#21820=DIRECTION('',(1.,0.,0.));
#21821=DIRECTION('',(0.,0.601815023152049,0.798635510047292));
#21822=DIRECTION('center_axis',(0.,0.857167300702112,-0.515038074910054));
#21823=DIRECTION('ref_axis',(0.,0.515038074910054,0.857167300702112));
#21824=DIRECTION('',(1.,0.,0.));
#21825=DIRECTION('',(0.,0.515038074910054,0.857167300702112));
#21826=DIRECTION('center_axis',(0.,0.90630778703665,-0.422618261740699));
#21827=DIRECTION('ref_axis',(0.,0.422618261740699,0.90630778703665));
#21828=DIRECTION('',(1.,0.,0.));
#21829=DIRECTION('',(0.,0.422618261740699,0.90630778703665));
#21830=DIRECTION('center_axis',(0.,0.945518575599317,-0.325568154457157));
#21831=DIRECTION('ref_axis',(0.,0.325568154457156,0.945518575599317));
#21832=DIRECTION('',(1.,0.,0.));
#21833=DIRECTION('',(0.,0.325568154457156,0.945518575599317));
#21834=DIRECTION('center_axis',(0.,-0.275637355816999,-0.961261695938319));
#21835=DIRECTION('ref_axis',(0.,0.961261695938319,-0.275637355816999));
#21836=DIRECTION('',(1.,0.,0.));
#21837=DIRECTION('',(0.,0.961261695938319,-0.275637355816999));
#21838=DIRECTION('center_axis',(0.,-0.945518575599316,0.325568154457159));
#21839=DIRECTION('ref_axis',(0.,-0.325568154457159,-0.945518575599316));
#21840=DIRECTION('',(1.,0.,0.));
#21841=DIRECTION('',(0.,-0.325568154457159,-0.945518575599316));
#21842=DIRECTION('center_axis',(0.,-0.90630778703665,0.4226182617407));
#21843=DIRECTION('ref_axis',(0.,-0.4226182617407,-0.90630778703665));
#21844=DIRECTION('',(1.,0.,0.));
#21845=DIRECTION('',(0.,-0.4226182617407,-0.90630778703665));
#21846=DIRECTION('center_axis',(0.,-0.857167300702112,0.515038074910054));
#21847=DIRECTION('ref_axis',(0.,-0.515038074910054,-0.857167300702112));
#21848=DIRECTION('',(1.,0.,0.));
#21849=DIRECTION('',(0.,-0.515038074910054,-0.857167300702112));
#21850=DIRECTION('center_axis',(0.,-0.798635510047293,0.601815023152048));
#21851=DIRECTION('ref_axis',(0.,-0.601815023152048,-0.798635510047293));
#21852=DIRECTION('',(1.,0.,0.));
#21853=DIRECTION('',(0.,-0.601815023152048,-0.798635510047293));
#21854=DIRECTION('center_axis',(0.,-0.731353701619171,0.681998360062498));
#21855=DIRECTION('ref_axis',(0.,-0.681998360062498,-0.731353701619171));
#21856=DIRECTION('',(1.,0.,0.));
#21857=DIRECTION('',(0.,-0.681998360062498,-0.731353701619171));
#21858=DIRECTION('center_axis',(0.,-0.656059028990507,0.754709580222772));
#21859=DIRECTION('ref_axis',(0.,-0.754709580222772,-0.656059028990507));
#21860=DIRECTION('',(1.,0.,0.));
#21861=DIRECTION('',(0.,-0.754709580222772,-0.656059028990507));
#21862=DIRECTION('center_axis',(0.,0.788010753606722,0.615661475325659));
#21863=DIRECTION('ref_axis',(0.,-0.615661475325659,0.788010753606722));
#21864=DIRECTION('',(0.,-0.615661475325659,0.788010753606722));
#21865=DIRECTION('center_axis',(1.,0.,0.));
#21866=DIRECTION('ref_axis',(0.,0.,-1.));
#21867=DIRECTION('center_axis',(0.,0.981627183447664,0.190808995376545));
#21868=DIRECTION('ref_axis',(0.,-0.190808995376545,0.981627183447664));
#21869=DIRECTION('',(1.,0.,0.));
#21870=DIRECTION('',(0.,-0.190808995376545,0.981627183447664));
#21871=DIRECTION('',(1.,0.,0.));
#21872=DIRECTION('center_axis',(0.,0.956304755963036,0.292371704722737));
#21873=DIRECTION('ref_axis',(0.,-0.292371704722737,0.956304755963036));
#21874=DIRECTION('',(1.,0.,0.));
#21875=DIRECTION('',(0.,-0.292371704722737,0.956304755963036));
#21876=DIRECTION('center_axis',(0.,0.92050485345244,0.390731128489274));
#21877=DIRECTION('ref_axis',(0.,-0.390731128489274,0.92050485345244));
#21878=DIRECTION('',(1.,0.,0.));
#21879=DIRECTION('',(0.,-0.390731128489274,0.92050485345244));
#21880=DIRECTION('center_axis',(0.,0.874619707139396,0.484809620246337));
#21881=DIRECTION('ref_axis',(0.,-0.484809620246337,0.874619707139396));
#21882=DIRECTION('',(1.,0.,0.));
#21883=DIRECTION('',(0.,-0.484809620246337,0.874619707139396));
#21884=DIRECTION('center_axis',(0.,0.819152044288992,0.573576436351047));
#21885=DIRECTION('ref_axis',(0.,-0.573576436351047,0.819152044288992));
#21886=DIRECTION('',(1.,0.,0.));
#21887=DIRECTION('',(0.,-0.573576436351047,0.819152044288992));
#21888=DIRECTION('center_axis',(0.,0.754709580222772,0.656059028990507));
#21889=DIRECTION('ref_axis',(0.,-0.656059028990507,0.754709580222772));
#21890=DIRECTION('',(1.,0.,0.));
#21891=DIRECTION('',(0.,-0.656059028990507,0.754709580222772));
#21892=DIRECTION('center_axis',(0.,0.694658370458997,-0.719339800338651));
#21893=DIRECTION('ref_axis',(0.,0.719339800338651,0.694658370458997));
#21894=DIRECTION('',(1.,0.,0.));
#21895=DIRECTION('',(0.,0.719339800338651,0.694658370458997));
#21896=DIRECTION('center_axis',(0.,-0.754709580222772,-0.656059028990507));
#21897=DIRECTION('ref_axis',(0.,0.656059028990507,-0.754709580222772));
#21898=DIRECTION('',(1.,0.,0.));
#21899=DIRECTION('',(0.,0.656059028990507,-0.754709580222772));
#21900=DIRECTION('center_axis',(0.,-0.819152044288991,-0.573576436351047));
#21901=DIRECTION('ref_axis',(0.,0.573576436351047,-0.819152044288991));
#21902=DIRECTION('',(1.,0.,0.));
#21903=DIRECTION('',(0.,0.573576436351047,-0.819152044288991));
#21904=DIRECTION('center_axis',(0.,-0.874619707139396,-0.484809620246337));
#21905=DIRECTION('ref_axis',(0.,0.484809620246337,-0.874619707139396));
#21906=DIRECTION('',(1.,0.,0.));
#21907=DIRECTION('',(0.,0.484809620246337,-0.874619707139396));
#21908=DIRECTION('center_axis',(0.,-0.92050485345244,-0.390731128489274));
#21909=DIRECTION('ref_axis',(0.,0.390731128489274,-0.92050485345244));
#21910=DIRECTION('',(1.,0.,0.));
#21911=DIRECTION('',(0.,0.390731128489274,-0.92050485345244));
#21912=DIRECTION('center_axis',(0.,-0.956304755963035,-0.292371704722737));
#21913=DIRECTION('ref_axis',(0.,0.292371704722737,-0.956304755963035));
#21914=DIRECTION('',(1.,0.,0.));
#21915=DIRECTION('',(0.,0.292371704722737,-0.956304755963035));
#21916=DIRECTION('center_axis',(0.,-0.981627183447664,-0.190808995376543));
#21917=DIRECTION('ref_axis',(0.,0.190808995376543,-0.981627183447664));
#21918=DIRECTION('',(1.,0.,0.));
#21919=DIRECTION('',(0.,0.190808995376543,-0.981627183447664));
#21920=DIRECTION('center_axis',(0.,-0.139173100960066,0.99026806874157));
#21921=DIRECTION('ref_axis',(0.,-0.99026806874157,-0.139173100960066));
#21922=DIRECTION('',(0.,-0.99026806874157,-0.139173100960066));
#21923=DIRECTION('center_axis',(1.,0.,0.));
#21924=DIRECTION('ref_axis',(0.,0.,-1.));
#21925=DIRECTION('center_axis',(0.,-0.656059028990508,0.754709580222771));
#21926=DIRECTION('ref_axis',(0.,-0.754709580222771,-0.656059028990508));
#21927=DIRECTION('',(1.,0.,0.));
#21928=DIRECTION('',(0.,-0.754709580222771,-0.656059028990508));
#21929=DIRECTION('',(1.,0.,0.));
#21930=DIRECTION('center_axis',(0.,-0.73135370161917,0.681998360062499));
#21931=DIRECTION('ref_axis',(0.,-0.681998360062499,-0.73135370161917));
#21932=DIRECTION('',(1.,0.,0.));
#21933=DIRECTION('',(0.,-0.681998360062499,-0.73135370161917));
#21934=DIRECTION('center_axis',(0.,-0.798635510047293,0.601815023152048));
#21935=DIRECTION('ref_axis',(0.,-0.601815023152048,-0.798635510047293));
#21936=DIRECTION('',(1.,0.,0.));
#21937=DIRECTION('',(0.,-0.601815023152048,-0.798635510047293));
#21938=DIRECTION('center_axis',(0.,-0.857167300702112,0.515038074910055));
#21939=DIRECTION('ref_axis',(0.,-0.515038074910055,-0.857167300702112));
#21940=DIRECTION('',(1.,0.,0.));
#21941=DIRECTION('',(0.,-0.515038074910055,-0.857167300702112));
#21942=DIRECTION('center_axis',(0.,-0.90630778703665,0.422618261740698));
#21943=DIRECTION('ref_axis',(0.,-0.422618261740698,-0.90630778703665));
#21944=DIRECTION('',(1.,0.,0.));
#21945=DIRECTION('',(0.,-0.422618261740698,-0.90630778703665));
#21946=DIRECTION('center_axis',(0.,-0.945518575599317,0.325568154457155));
#21947=DIRECTION('ref_axis',(0.,-0.325568154457155,-0.945518575599317));
#21948=DIRECTION('',(1.,0.,0.));
#21949=DIRECTION('',(0.,-0.325568154457155,-0.945518575599317));
#21950=DIRECTION('center_axis',(0.,0.275637355816999,0.961261695938319));
#21951=DIRECTION('ref_axis',(0.,-0.961261695938319,0.275637355816999));
#21952=DIRECTION('',(1.,0.,0.));
#21953=DIRECTION('',(0.,-0.961261695938319,0.275637355816999));
#21954=DIRECTION('center_axis',(0.,0.945518575599317,-0.325568154457157));
#21955=DIRECTION('ref_axis',(0.,0.325568154457157,0.945518575599317));
#21956=DIRECTION('',(1.,0.,0.));
#21957=DIRECTION('',(0.,0.325568154457157,0.945518575599317));
#21958=DIRECTION('center_axis',(0.,0.90630778703665,-0.422618261740699));
#21959=DIRECTION('ref_axis',(0.,0.422618261740699,0.90630778703665));
#21960=DIRECTION('',(1.,0.,0.));
#21961=DIRECTION('',(0.,0.422618261740699,0.90630778703665));
#21962=DIRECTION('center_axis',(0.,0.857167300702113,-0.515038074910053));
#21963=DIRECTION('ref_axis',(0.,0.515038074910053,0.857167300702113));
#21964=DIRECTION('',(1.,0.,0.));
#21965=DIRECTION('',(0.,0.515038074910053,0.857167300702113));
#21966=DIRECTION('center_axis',(0.,0.798635510047293,-0.601815023152048));
#21967=DIRECTION('ref_axis',(0.,0.601815023152048,0.798635510047293));
#21968=DIRECTION('',(1.,0.,0.));
#21969=DIRECTION('',(0.,0.601815023152048,0.798635510047293));
#21970=DIRECTION('center_axis',(0.,0.73135370161917,-0.681998360062499));
#21971=DIRECTION('ref_axis',(0.,0.681998360062499,0.73135370161917));
#21972=DIRECTION('',(1.,0.,0.));
#21973=DIRECTION('',(0.,0.681998360062499,0.73135370161917));
#21974=DIRECTION('center_axis',(0.,0.656059028990508,-0.754709580222772));
#21975=DIRECTION('ref_axis',(0.,0.754709580222772,0.656059028990508));
#21976=DIRECTION('',(1.,0.,0.));
#21977=DIRECTION('',(0.,0.754709580222772,0.656059028990508));
#21978=DIRECTION('center_axis',(0.,-0.788010753606722,-0.615661475325659));
#21979=DIRECTION('ref_axis',(0.,0.615661475325658,-0.788010753606722));
#21980=DIRECTION('',(0.,0.615661475325658,-0.788010753606722));
#21981=DIRECTION('center_axis',(1.,0.,0.));
#21982=DIRECTION('ref_axis',(0.,0.,-1.));
#21983=DIRECTION('center_axis',(1.,0.,0.));
#21984=DIRECTION('ref_axis',(0.,0.,-1.));
#21985=DIRECTION('',(-1.,0.,0.));
#21986=DIRECTION('',(-1.,0.,0.));
#21987=DIRECTION('center_axis',(0.,-1.,0.));
#21988=DIRECTION('ref_axis',(0.,0.,-1.));
#21989=DIRECTION('axis',(0.,0.,1.));
#21990=DIRECTION('refdir',(1.,0.,0.));
#21991=DIRECTION('center_axis',(1.,0.,0.));
#21992=DIRECTION('ref_axis',(0.,0.,-1.));
#21993=DIRECTION('center_axis',(1.,0.,0.));
#21994=DIRECTION('ref_axis',(0.,0.,-1.));
#21995=DIRECTION('',(1.,0.,0.));
#21996=DIRECTION('center_axis',(1.,0.,0.));
#21997=DIRECTION('ref_axis',(0.,0.,-1.));
#21998=DIRECTION('center_axis',(1.,0.,0.));
#21999=DIRECTION('ref_axis',(0.,0.,-1.));
#22000=DIRECTION('center_axis',(1.,0.,0.));
#22001=DIRECTION('ref_axis',(0.,0.,-1.));
#22002=DIRECTION('center_axis',(1.,0.,0.));
#22003=DIRECTION('ref_axis',(0.,0.,-1.));
#22004=DIRECTION('',(1.,0.,0.));
#22005=DIRECTION('center_axis',(1.,0.,0.));
#22006=DIRECTION('ref_axis',(0.,0.,-1.));
#22007=DIRECTION('center_axis',(1.,0.,0.));
#22008=DIRECTION('ref_axis',(0.,0.,-1.));
#22009=DIRECTION('center_axis',(1.,0.,0.));
#22010=DIRECTION('ref_axis',(0.,0.,-1.));
#22011=DIRECTION('center_axis',(1.,0.,0.));
#22012=DIRECTION('ref_axis',(0.,0.,-1.));
#22013=DIRECTION('',(1.,0.,0.));
#22014=DIRECTION('center_axis',(1.,0.,0.));
#22015=DIRECTION('ref_axis',(0.,0.,-1.));
#22016=DIRECTION('center_axis',(1.,0.,0.));
#22017=DIRECTION('ref_axis',(0.,0.,-1.));
#22018=DIRECTION('center_axis',(1.,0.,0.));
#22019=DIRECTION('ref_axis',(0.,0.,-1.));
#22020=DIRECTION('center_axis',(1.,0.,0.));
#22021=DIRECTION('ref_axis',(0.,0.,-1.));
#22022=DIRECTION('',(1.,0.,0.));
#22023=DIRECTION('center_axis',(1.,0.,0.));
#22024=DIRECTION('ref_axis',(0.,0.,-1.));
#22025=DIRECTION('center_axis',(1.,0.,0.));
#22026=DIRECTION('ref_axis',(0.,0.,-1.));
#22027=DIRECTION('center_axis',(1.,0.,0.));
#22028=DIRECTION('ref_axis',(0.,0.,-1.));
#22029=DIRECTION('center_axis',(1.,0.,0.));
#22030=DIRECTION('ref_axis',(0.,0.,-1.));
#22031=DIRECTION('',(1.,0.,0.));
#22032=DIRECTION('center_axis',(1.,0.,0.));
#22033=DIRECTION('ref_axis',(0.,0.,-1.));
#22034=DIRECTION('center_axis',(1.,0.,0.));
#22035=DIRECTION('ref_axis',(0.,0.,-1.));
#22036=DIRECTION('center_axis',(1.,0.,0.));
#22037=DIRECTION('ref_axis',(0.,0.,-1.));
#22038=DIRECTION('center_axis',(1.,0.,0.));
#22039=DIRECTION('ref_axis',(0.,0.,-1.));
#22040=DIRECTION('',(1.,0.,0.));
#22041=DIRECTION('center_axis',(1.,0.,0.));
#22042=DIRECTION('ref_axis',(0.,0.,-1.));
#22043=DIRECTION('center_axis',(1.,0.,0.));
#22044=DIRECTION('ref_axis',(0.,0.,-1.));
#22045=DIRECTION('center_axis',(1.,0.,0.));
#22046=DIRECTION('ref_axis',(0.,1.,0.));
#22047=DIRECTION('center_axis',(1.,0.,0.));
#22048=DIRECTION('ref_axis',(0.,0.,-1.));
#22049=DIRECTION('',(1.,0.,0.));
#22050=DIRECTION('center_axis',(1.,0.,0.));
#22051=DIRECTION('ref_axis',(0.,0.,-1.));
#22052=DIRECTION('center_axis',(-1.,0.,0.));
#22053=DIRECTION('ref_axis',(0.,0.,1.));
#22054=DIRECTION('center_axis',(-1.,0.,0.));
#22055=DIRECTION('ref_axis',(0.,1.,0.));
#22056=DIRECTION('center_axis',(1.,0.,0.));
#22057=DIRECTION('ref_axis',(0.,0.,-1.));
#22058=DIRECTION('center_axis',(1.,0.,0.));
#22059=DIRECTION('ref_axis',(0.,1.,0.));
#22060=DIRECTION('center_axis',(1.,0.,0.));
#22061=DIRECTION('ref_axis',(0.,1.,0.));
#22062=DIRECTION('center_axis',(1.,0.,0.));
#22063=DIRECTION('ref_axis',(0.,0.,-1.));
#22064=DIRECTION('',(-1.,0.,0.));
#22065=DIRECTION('center_axis',(1.,0.,0.));
#22066=DIRECTION('ref_axis',(0.,1.,0.));
#22067=DIRECTION('center_axis',(1.,0.,0.));
#22068=DIRECTION('ref_axis',(0.,0.,-1.));
#22069=DIRECTION('',(-0.707106781186547,0.707106781186548,8.65956056235494E-17));
#22070=DIRECTION('center_axis',(1.,0.,0.));
#22071=DIRECTION('ref_axis',(0.,0.,-1.));
#22072=DIRECTION('center_axis',(1.,0.,0.));
#22073=DIRECTION('ref_axis',(0.,1.,0.));
#22074=DIRECTION('center_axis',(1.,0.,0.));
#22075=DIRECTION('ref_axis',(0.,0.,-1.));
#22076=DIRECTION('',(-1.,0.,0.));
#22077=DIRECTION('center_axis',(-1.,0.,0.));
#22078=DIRECTION('ref_axis',(0.,0.,1.));
#22079=DIRECTION('center_axis',(1.,0.,0.));
#22080=DIRECTION('ref_axis',(0.,0.,-1.));
#22081=DIRECTION('center_axis',(1.,0.,0.));
#22082=DIRECTION('ref_axis',(0.,1.,0.));
#22083=DIRECTION('center_axis',(1.,0.,0.));
#22084=DIRECTION('ref_axis',(0.,0.,-1.));
#22085=DIRECTION('',(-0.707106781186549,0.707106781186546,8.65956056235491E-17));
#22086=DIRECTION('center_axis',(1.,0.,0.));
#22087=DIRECTION('ref_axis',(0.,1.,0.));
#22088=DIRECTION('center_axis',(1.,0.,0.));
#22089=DIRECTION('ref_axis',(0.,0.,-1.));
#22090=DIRECTION('',(-1.,0.,0.));
#22091=DIRECTION('center_axis',(-1.,0.,0.));
#22092=DIRECTION('ref_axis',(0.,1.,0.));
#22093=DIRECTION('center_axis',(1.,0.,0.));
#22094=DIRECTION('ref_axis',(0.,0.,-1.));
#22095=DIRECTION('',(-0.707106781186549,-0.707106781186546,-8.65956056235491E-17));
#22096=DIRECTION('center_axis',(1.,0.,0.));
#22097=DIRECTION('ref_axis',(0.,0.,-1.));
#22098=DIRECTION('center_axis',(1.,0.,0.));
#22099=DIRECTION('ref_axis',(0.,0.,-1.));
#22100=DIRECTION('center_axis',(-1.,0.,0.));
#22101=DIRECTION('ref_axis',(0.,1.,0.));
#22102=DIRECTION('center_axis',(1.,0.,0.));
#22103=DIRECTION('ref_axis',(0.,0.,-1.));
#22104=DIRECTION('',(-0.707106781186547,-0.707106781186547,-8.65956056235493E-17));
#22105=DIRECTION('center_axis',(1.,0.,0.));
#22106=DIRECTION('ref_axis',(0.,1.,0.));
#22107=DIRECTION('',(-1.,0.,0.));
#22108=DIRECTION('center_axis',(-1.,0.,0.));
#22109=DIRECTION('ref_axis',(0.,1.,0.));
#22110=DIRECTION('center_axis',(1.,0.,0.));
#22111=DIRECTION('ref_axis',(0.,0.,-1.));
#22112=DIRECTION('',(-0.707106781186548,-0.707106781186548,-8.65956056235493E-17));
#22113=DIRECTION('center_axis',(1.,0.,0.));
#22114=DIRECTION('ref_axis',(0.,0.,-1.));
#22115=DIRECTION('center_axis',(1.,0.,0.));
#22116=DIRECTION('ref_axis',(0.,0.,-1.));
#22117=DIRECTION('center_axis',(1.,0.,0.));
#22118=DIRECTION('ref_axis',(0.,1.,0.));
#22119=DIRECTION('',(-0.701238976116888,0.712926292385503,8.73082901997896E-17));
#22120=DIRECTION('center_axis',(1.,0.,0.));
#22121=DIRECTION('ref_axis',(0.,0.,-1.));
#22122=DIRECTION('center_axis',(1.,0.,0.));
#22123=DIRECTION('ref_axis',(0.,1.,0.));
#22124=DIRECTION('',(-1.,0.,0.));
#22125=DIRECTION('center_axis',(1.,0.,0.));
#22126=DIRECTION('ref_axis',(0.,0.,-1.));
#22127=DIRECTION('center_axis',(-1.,0.,0.));
#22128=DIRECTION('ref_axis',(0.,1.,0.));
#22129=DIRECTION('',(-0.701238976116887,-0.712926292385503,-8.73082901997896E-17));
#22130=DIRECTION('center_axis',(1.,0.,0.));
#22131=DIRECTION('ref_axis',(0.,0.,-1.));
#22132=DIRECTION('center_axis',(-1.,0.,0.));
#22133=DIRECTION('ref_axis',(0.,0.,1.));
#22134=DIRECTION('axis',(0.,0.,1.));
#22135=DIRECTION('refdir',(1.,0.,0.));
#22136=DIRECTION('center_axis',(0.,0.024997395914712,0.999687516275703));
#22137=DIRECTION('ref_axis',(0.,-0.999687516275703,0.024997395914712));
#22138=DIRECTION('',(1.,0.,0.));
#22139=DIRECTION('',(0.,-0.999687516275703,0.024997395914712));
#22140=DIRECTION('',(1.,0.,0.));
#22141=DIRECTION('',(0.,-0.999687516275703,0.024997395914712));
#22142=DIRECTION('',(1.,0.,0.));
#22143=DIRECTION('',(1.,0.,0.));
#22144=DIRECTION('center_axis',(0.,0.0249973959147123,-0.999687516275703));
#22145=DIRECTION('ref_axis',(0.,0.999687516275703,0.0249973959147123));
#22146=DIRECTION('',(0.,0.999687516275703,0.0249973959147123));
#22147=DIRECTION('',(0.,0.999687516275703,0.0249973959147123));
#22148=DIRECTION('center_axis',(1.,0.,0.));
#22149=DIRECTION('ref_axis',(0.,0.,-1.));
#22150=DIRECTION('center_axis',(1.,0.,0.));
#22151=DIRECTION('ref_axis',(0.,0.,-1.));
#22152=DIRECTION('axis',(0.,0.,1.));
#22153=DIRECTION('refdir',(1.,0.,0.));
#22154=DIRECTION('center_axis',(1.,0.,0.));
#22155=DIRECTION('ref_axis',(0.,0.,-1.));
#22156=DIRECTION('center_axis',(1.,0.,0.));
#22157=DIRECTION('ref_axis',(0.,0.,-1.));
#22158=DIRECTION('center_axis',(-1.,0.,3.38602178801704E-15));
#22159=DIRECTION('ref_axis',(0.,1.,3.0434711729182E-17));
#22160=DIRECTION('center_axis',(1.,0.,0.));
#22161=DIRECTION('ref_axis',(0.,1.,0.));
#22162=DIRECTION('center_axis',(-1.,0.,0.));
#22163=DIRECTION('ref_axis',(0.,1.,6.12323399573677E-17));
#22164=DIRECTION('center_axis',(1.,0.,0.));
#22165=DIRECTION('ref_axis',(0.,1.,0.));
#22166=DIRECTION('center_axis',(1.,0.,0.));
#22167=DIRECTION('ref_axis',(0.,-0.78183148246803,-0.623489801858733));
#22168=DIRECTION('center_axis',(1.,0.,0.));
#22169=DIRECTION('ref_axis',(0.,1.,0.));
#22170=DIRECTION('center_axis',(1.,0.,0.));
#22171=DIRECTION('ref_axis',(0.,-0.78183148246803,-0.623489801858733));
#22172=DIRECTION('center_axis',(1.,0.,0.));
#22173=DIRECTION('ref_axis',(0.,1.,0.));
#22174=DIRECTION('center_axis',(1.,0.,0.));
#22175=DIRECTION('ref_axis',(0.,-0.974927912181824,0.222520933956315));
#22176=DIRECTION('center_axis',(1.,0.,0.));
#22177=DIRECTION('ref_axis',(0.,1.,0.));
#22178=DIRECTION('center_axis',(1.,0.,0.));
#22179=DIRECTION('ref_axis',(0.,-0.974927912181824,0.222520933956315));
#22180=DIRECTION('center_axis',(1.,0.,0.));
#22181=DIRECTION('ref_axis',(0.,-1.,0.));
#22182=DIRECTION('center_axis',(1.,0.,0.));
#22183=DIRECTION('ref_axis',(0.,-0.433883739117558,0.900968867902419));
#22184=DIRECTION('center_axis',(1.,0.,0.));
#22185=DIRECTION('ref_axis',(0.,-1.,0.));
#22186=DIRECTION('center_axis',(1.,0.,0.));
#22187=DIRECTION('ref_axis',(0.,-0.433883739117558,0.900968867902419));
#22188=DIRECTION('center_axis',(1.,0.,0.));
#22189=DIRECTION('ref_axis',(0.,-1.,0.));
#22190=DIRECTION('center_axis',(1.,0.,0.));
#22191=DIRECTION('ref_axis',(0.,0.433883739117558,0.900968867902419));
#22192=DIRECTION('',(-1.,0.,0.));
#22193=DIRECTION('center_axis',(1.,0.,0.));
#22194=DIRECTION('ref_axis',(0.,0.,-1.));
#22195=DIRECTION('center_axis',(1.,0.,0.));
#22196=DIRECTION('ref_axis',(0.,0.433883739117558,0.900968867902419));
#22197=DIRECTION('center_axis',(1.,0.,0.));
#22198=DIRECTION('ref_axis',(0.,-1.,0.));
#22199=DIRECTION('center_axis',(1.,0.,0.));
#22200=DIRECTION('ref_axis',(0.,0.433883739117558,0.900968867902419));
#22201=DIRECTION('center_axis',(1.,0.,0.));
#22202=DIRECTION('ref_axis',(0.,-1.,0.));
#22203=DIRECTION('center_axis',(1.,0.,0.));
#22204=DIRECTION('ref_axis',(0.,0.974927912181824,0.222520933956314));
#22205=DIRECTION('center_axis',(1.,0.,0.));
#22206=DIRECTION('ref_axis',(0.,-1.,0.));
#22207=DIRECTION('center_axis',(1.,0.,0.));
#22208=DIRECTION('ref_axis',(0.,0.974927912181824,0.222520933956314));
#22209=DIRECTION('center_axis',(1.,0.,0.));
#22210=DIRECTION('ref_axis',(0.,1.,0.));
#22211=DIRECTION('center_axis',(1.,0.,0.));
#22212=DIRECTION('ref_axis',(0.,0.78183148246803,-0.623489801858734));
#22213=DIRECTION('center_axis',(1.,0.,0.));
#22214=DIRECTION('ref_axis',(0.,1.,0.));
#22215=DIRECTION('center_axis',(1.,0.,0.));
#22216=DIRECTION('ref_axis',(0.,0.78183148246803,-0.623489801858734));
#22217=DIRECTION('center_axis',(1.,0.,0.));
#22218=DIRECTION('ref_axis',(0.,1.,0.));
#22219=DIRECTION('center_axis',(1.,0.,0.));
#22220=DIRECTION('ref_axis',(0.,0.,-1.));
#22221=DIRECTION('center_axis',(1.,0.,0.));
#22222=DIRECTION('ref_axis',(0.,1.,0.));
#22223=DIRECTION('center_axis',(1.,0.,0.));
#22224=DIRECTION('ref_axis',(0.,0.,-1.));
#22225=DIRECTION('center_axis',(-1.,0.,3.38602178801705E-15));
#22226=DIRECTION('ref_axis',(0.,1.,3.0434711729182E-17));
#22227=DIRECTION('center_axis',(-1.,0.,0.));
#22228=DIRECTION('ref_axis',(0.,1.,6.12323399573677E-17));
#22229=DIRECTION('center_axis',(-1.,0.,3.38602178801705E-15));
#22230=DIRECTION('ref_axis',(0.,1.,3.0434711729182E-17));
#22231=DIRECTION('center_axis',(-1.,0.,0.));
#22232=DIRECTION('ref_axis',(0.,1.,6.12323399573677E-17));
#22233=DIRECTION('center_axis',(-1.,0.,3.38602178801705E-15));
#22234=DIRECTION('ref_axis',(0.,-1.,-3.0434711729182E-17));
#22235=DIRECTION('center_axis',(-1.,0.,0.));
#22236=DIRECTION('ref_axis',(0.,-1.,-6.12323399573677E-17));
#22237=DIRECTION('center_axis',(-1.,0.,3.38602178801704E-15));
#22238=DIRECTION('ref_axis',(0.,-1.,-3.0434711729182E-17));
#22239=DIRECTION('center_axis',(-1.,0.,0.));
#22240=DIRECTION('ref_axis',(0.,-1.,-6.12323399573677E-17));
#22241=DIRECTION('center_axis',(-1.,0.,3.38602178801705E-15));
#22242=DIRECTION('ref_axis',(0.,-1.,-3.0434711729182E-17));
#22243=DIRECTION('center_axis',(-1.,0.,0.));
#22244=DIRECTION('ref_axis',(0.,-1.,-6.12323399573677E-17));
#22245=DIRECTION('center_axis',(-1.,0.,3.38602178801704E-15));
#22246=DIRECTION('ref_axis',(0.,1.,3.0434711729182E-17));
#22247=DIRECTION('center_axis',(-1.,0.,0.));
#22248=DIRECTION('ref_axis',(0.,1.,6.12323399573677E-17));
#22249=DIRECTION('center_axis',(-1.,0.,3.38602178801704E-15));
#22250=DIRECTION('ref_axis',(0.,1.,3.0434711729182E-17));
#22251=DIRECTION('center_axis',(-1.,0.,0.));
#22252=DIRECTION('ref_axis',(0.,1.,6.12323399573677E-17));
#22253=DIRECTION('center_axis',(-1.,0.,3.38602178801704E-15));
#22254=DIRECTION('ref_axis',(0.,1.,3.0434711729182E-17));
#22255=DIRECTION('center_axis',(-1.,0.,0.));
#22256=DIRECTION('ref_axis',(0.,1.,6.12323399573677E-17));
#22257=DIRECTION('center_axis',(-1.,0.,3.38602178801704E-15));
#22258=DIRECTION('ref_axis',(0.,-1.,-3.0434711729182E-17));
#22259=DIRECTION('center_axis',(-1.,0.,0.));
#22260=DIRECTION('ref_axis',(0.,-1.,-6.12323399573677E-17));
#22261=DIRECTION('center_axis',(-1.,0.,3.38602178801704E-15));
#22262=DIRECTION('ref_axis',(0.,-1.,-3.0434711729182E-17));
#22263=DIRECTION('center_axis',(-1.,0.,0.));
#22264=DIRECTION('ref_axis',(0.,-1.,-6.12323399573677E-17));
#22265=DIRECTION('center_axis',(-1.,0.,3.38602178801704E-15));
#22266=DIRECTION('ref_axis',(0.,-1.,-3.0434711729182E-17));
#22267=DIRECTION('center_axis',(-1.,0.,0.));
#22268=DIRECTION('ref_axis',(0.,-1.,-6.12323399573677E-17));
#22269=DIRECTION('center_axis',(-1.,0.,3.38602178801705E-15));
#22270=DIRECTION('ref_axis',(0.,1.,3.0434711729182E-17));
#22271=DIRECTION('center_axis',(-1.,0.,0.));
#22272=DIRECTION('ref_axis',(0.,1.,6.12323399573677E-17));
#22273=DIRECTION('center_axis',(-1.,0.,3.38602178801704E-15));
#22274=DIRECTION('ref_axis',(0.,1.,3.0434711729182E-17));
#22275=DIRECTION('center_axis',(-1.,0.,0.));
#22276=DIRECTION('ref_axis',(0.,1.,6.12323399573677E-17));
#22277=DIRECTION('center_axis',(-1.,0.,0.));
#22278=DIRECTION('ref_axis',(0.,-1.,0.));
#22279=DIRECTION('center_axis',(-1.,0.,0.));
#22280=DIRECTION('ref_axis',(0.,-1.,0.));
#22281=DIRECTION('',(0.707106781186548,-0.707106781186547,8.65956056235493E-17));
#22282=DIRECTION('center_axis',(1.,0.,0.));
#22283=DIRECTION('ref_axis',(0.,-1.,0.));
#22284=DIRECTION('center_axis',(1.,0.,0.));
#22285=DIRECTION('ref_axis',(0.,-1.,0.));
#22286=DIRECTION('center_axis',(1.,0.,0.));
#22287=DIRECTION('ref_axis',(0.,1.,0.));
#22288=DIRECTION('center_axis',(-1.,0.,0.));
#22289=DIRECTION('ref_axis',(0.,-1.,0.));
#22290=DIRECTION('center_axis',(-1.,0.,0.));
#22291=DIRECTION('ref_axis',(0.,-1.,0.));
#22292=DIRECTION('',(-1.,0.,0.));
#22293=DIRECTION('center_axis',(-1.,0.,0.));
#22294=DIRECTION('ref_axis',(0.,0.,1.));
#22295=DIRECTION('center_axis',(1.,0.,0.));
#22296=DIRECTION('ref_axis',(0.,0.,-1.));
#22297=DIRECTION('center_axis',(1.,0.,0.));
#22298=DIRECTION('ref_axis',(0.,-1.,0.));
#22299=DIRECTION('',(0.707106781186546,0.707106781186549,-8.65956056235496E-17));
#22300=DIRECTION('center_axis',(1.,0.,0.));
#22301=DIRECTION('ref_axis',(0.,-1.,0.));
#22302=DIRECTION('center_axis',(1.,0.,0.));
#22303=DIRECTION('ref_axis',(0.,0.,-1.));
#22304=DIRECTION('center_axis',(1.,0.,0.));
#22305=DIRECTION('ref_axis',(0.,0.,-1.));
#22306=DIRECTION('center_axis',(1.,0.,0.));
#22307=DIRECTION('ref_axis',(0.,-0.78183148246803,-0.623489801858733));
#22308=DIRECTION('center_axis',(1.,0.,0.));
#22309=DIRECTION('ref_axis',(0.,-0.78183148246803,-0.623489801858733));
#22310=DIRECTION('center_axis',(-1.,0.,0.));
#22311=DIRECTION('ref_axis',(0.,1.,0.));
#22312=DIRECTION('center_axis',(1.,0.,0.));
#22313=DIRECTION('ref_axis',(0.,0.,-1.));
#22314=DIRECTION('center_axis',(1.,0.,0.));
#22315=DIRECTION('ref_axis',(0.,-0.974927912181824,0.222520933956315));
#22316=DIRECTION('center_axis',(1.,0.,0.));
#22317=DIRECTION('ref_axis',(0.,-0.974927912181824,0.222520933956315));
#22318=DIRECTION('center_axis',(-1.,0.,0.));
#22319=DIRECTION('ref_axis',(0.,1.,0.));
#22320=DIRECTION('center_axis',(1.,0.,0.));
#22321=DIRECTION('ref_axis',(0.,0.,-1.));
#22322=DIRECTION('center_axis',(1.,0.,0.));
#22323=DIRECTION('ref_axis',(0.,-0.433883739117558,0.900968867902419));
#22324=DIRECTION('center_axis',(1.,0.,0.));
#22325=DIRECTION('ref_axis',(0.,-0.433883739117558,0.900968867902419));
#22326=DIRECTION('center_axis',(-1.,0.,0.));
#22327=DIRECTION('ref_axis',(0.,1.,0.));
#22328=DIRECTION('center_axis',(1.,0.,0.));
#22329=DIRECTION('ref_axis',(0.,0.,-1.));
#22330=DIRECTION('center_axis',(1.,0.,0.));
#22331=DIRECTION('ref_axis',(0.,0.433883739117558,0.900968867902419));
#22332=DIRECTION('center_axis',(1.,0.,0.));
#22333=DIRECTION('ref_axis',(0.,0.433883739117558,0.900968867902419));
#22334=DIRECTION('center_axis',(-1.,0.,0.));
#22335=DIRECTION('ref_axis',(0.,1.,0.));
#22336=DIRECTION('center_axis',(1.,0.,0.));
#22337=DIRECTION('ref_axis',(0.,0.,-1.));
#22338=DIRECTION('center_axis',(1.,0.,0.));
#22339=DIRECTION('ref_axis',(0.,0.974927912181824,0.222520933956314));
#22340=DIRECTION('center_axis',(1.,0.,0.));
#22341=DIRECTION('ref_axis',(0.,0.974927912181824,0.222520933956314));
#22342=DIRECTION('center_axis',(-1.,0.,0.));
#22343=DIRECTION('ref_axis',(0.,1.,0.));
#22344=DIRECTION('center_axis',(1.,0.,0.));
#22345=DIRECTION('ref_axis',(0.,0.,-1.));
#22346=DIRECTION('center_axis',(1.,0.,0.));
#22347=DIRECTION('ref_axis',(0.,0.78183148246803,-0.623489801858734));
#22348=DIRECTION('center_axis',(1.,0.,0.));
#22349=DIRECTION('ref_axis',(0.,0.78183148246803,-0.623489801858734));
#22350=DIRECTION('center_axis',(-1.,0.,0.));
#22351=DIRECTION('ref_axis',(0.,1.,0.));
#22352=DIRECTION('center_axis',(1.,0.,0.));
#22353=DIRECTION('ref_axis',(0.,0.,-1.));
#22354=DIRECTION('center_axis',(1.,0.,0.));
#22355=DIRECTION('ref_axis',(0.,0.,-1.));
#22356=DIRECTION('center_axis',(1.,0.,0.));
#22357=DIRECTION('ref_axis',(0.,0.,-1.));
#22358=DIRECTION('center_axis',(-1.,0.,0.));
#22359=DIRECTION('ref_axis',(0.,1.,0.));
#22360=DIRECTION('center_axis',(1.,0.,0.));
#22361=DIRECTION('ref_axis',(0.,-0.78183148246803,-0.623489801858733));
#22362=DIRECTION('center_axis',(1.,0.,0.));
#22363=DIRECTION('ref_axis',(0.,-0.78183148246803,-0.623489801858733));
#22364=DIRECTION('center_axis',(-1.,0.,0.));
#22365=DIRECTION('ref_axis',(0.,1.,0.));
#22366=DIRECTION('center_axis',(1.,0.,0.));
#22367=DIRECTION('ref_axis',(0.,0.,-1.));
#22368=DIRECTION('center_axis',(1.,0.,0.));
#22369=DIRECTION('ref_axis',(0.,-0.974927912181824,0.222520933956315));
#22370=DIRECTION('center_axis',(1.,0.,0.));
#22371=DIRECTION('ref_axis',(0.,-0.974927912181824,0.222520933956315));
#22372=DIRECTION('center_axis',(-1.,0.,0.));
#22373=DIRECTION('ref_axis',(0.,1.,0.));
#22374=DIRECTION('center_axis',(1.,0.,0.));
#22375=DIRECTION('ref_axis',(0.,0.,-1.));
#22376=DIRECTION('center_axis',(1.,0.,0.));
#22377=DIRECTION('ref_axis',(0.,-0.433883739117558,0.900968867902419));
#22378=DIRECTION('center_axis',(1.,0.,0.));
#22379=DIRECTION('ref_axis',(0.,-0.433883739117558,0.900968867902419));
#22380=DIRECTION('center_axis',(-1.,0.,0.));
#22381=DIRECTION('ref_axis',(0.,1.,0.));
#22382=DIRECTION('center_axis',(1.,0.,0.));
#22383=DIRECTION('ref_axis',(0.,0.,-1.));
#22384=DIRECTION('center_axis',(1.,0.,0.));
#22385=DIRECTION('ref_axis',(0.,0.433883739117558,0.900968867902419));
#22386=DIRECTION('center_axis',(1.,0.,0.));
#22387=DIRECTION('ref_axis',(0.,0.433883739117558,0.900968867902419));
#22388=DIRECTION('center_axis',(-1.,0.,0.));
#22389=DIRECTION('ref_axis',(0.,1.,0.));
#22390=DIRECTION('center_axis',(1.,0.,0.));
#22391=DIRECTION('ref_axis',(0.,0.,-1.));
#22392=DIRECTION('center_axis',(1.,0.,0.));
#22393=DIRECTION('ref_axis',(0.,0.974927912181824,0.222520933956314));
#22394=DIRECTION('center_axis',(1.,0.,0.));
#22395=DIRECTION('ref_axis',(0.,0.974927912181824,0.222520933956314));
#22396=DIRECTION('center_axis',(-1.,0.,0.));
#22397=DIRECTION('ref_axis',(0.,1.,0.));
#22398=DIRECTION('center_axis',(1.,0.,0.));
#22399=DIRECTION('ref_axis',(0.,0.,-1.));
#22400=DIRECTION('center_axis',(1.,0.,0.));
#22401=DIRECTION('ref_axis',(0.,0.78183148246803,-0.623489801858734));
#22402=DIRECTION('center_axis',(1.,0.,0.));
#22403=DIRECTION('ref_axis',(0.,0.78183148246803,-0.623489801858734));
#22404=DIRECTION('center_axis',(-1.,0.,0.));
#22405=DIRECTION('ref_axis',(0.,1.,0.));
#22406=DIRECTION('center_axis',(1.,0.,0.));
#22407=DIRECTION('ref_axis',(0.,0.,-1.));
#22408=DIRECTION('center_axis',(1.,0.,0.));
#22409=DIRECTION('ref_axis',(0.,0.,-1.));
#22410=DIRECTION('center_axis',(1.,0.,0.));
#22411=DIRECTION('ref_axis',(0.,0.,-1.));
#22412=DIRECTION('center_axis',(1.,0.,0.));
#22413=DIRECTION('ref_axis',(0.,0.,-1.));
#22414=DIRECTION('center_axis',(1.,0.,0.));
#22415=DIRECTION('ref_axis',(0.,0.,-1.));
#22416=DIRECTION('center_axis',(1.,0.,0.));
#22417=DIRECTION('ref_axis',(0.,1.,0.));
#22418=DIRECTION('',(-0.707106781186549,0.707106781186546,8.65956056235492E-17));
#22419=DIRECTION('center_axis',(-1.,0.,0.));
#22420=DIRECTION('ref_axis',(0.,1.,0.));
#22421=DIRECTION('center_axis',(-1.,0.,0.));
#22422=DIRECTION('ref_axis',(0.,1.,0.));
#22423=DIRECTION('center_axis',(1.,0.,0.));
#22424=DIRECTION('ref_axis',(0.,0.,-1.));
#22425=DIRECTION('',(-0.371390676354097,-0.928476690885262,-1.13705600757556E-16));
#22426=DIRECTION('center_axis',(1.,0.,0.));
#22427=DIRECTION('ref_axis',(0.,1.,0.));
#22428=DIRECTION('center_axis',(1.,0.,0.));
#22429=DIRECTION('ref_axis',(0.,0.,-1.));
#22430=DIRECTION('',(-1.,0.,0.));
#22431=DIRECTION('center_axis',(-1.,0.,0.));
#22432=DIRECTION('ref_axis',(0.,1.,0.));
#22433=DIRECTION('',(-0.707106781186548,-0.707106781186547,-8.65956056235493E-17));
#22434=DIRECTION('axis',(0.,0.,1.));
#22435=DIRECTION('refdir',(1.,0.,0.));
#22436=DIRECTION('center_axis',(0.,0.866025403784439,0.499999999999999));
#22437=DIRECTION('ref_axis',(0.,-0.499999999999999,0.866025403784439));
#22438=DIRECTION('',(-1.,0.,0.));
#22439=DIRECTION('',(0.,0.499999999999999,-0.866025403784439));
#22440=DIRECTION('',(1.,0.,0.));
#22441=DIRECTION('center_axis',(0.,0.996808887069657,-0.0798250753770538));
#22442=DIRECTION('ref_axis',(0.,0.0798250753770538,0.996808887069657));
#22443=DIRECTION('',(1.,0.,0.));
#22444=DIRECTION('',(0.,-0.0798250753770538,-0.996808887069657));
#22445=DIRECTION('center_axis',(0.,0.5,0.866025403784438));
#22446=DIRECTION('ref_axis',(1.,0.,0.));
#22447=DIRECTION('',(-1.,0.,0.));
#22448=DIRECTION('',(0.,0.866025403784438,-0.5));
#22449=DIRECTION('',(1.,0.,0.));
#22450=DIRECTION('center_axis',(0.,0.903174356608943,0.429273900399292));
#22451=DIRECTION('ref_axis',(0.,-0.429273900399292,0.903174356608943));
#22452=DIRECTION('',(1.,0.,0.));
#22453=DIRECTION('',(0.,0.429273900399292,-0.903174356608943));
#22454=DIRECTION('center_axis',(0.,0.,1.));
#22455=DIRECTION('ref_axis',(1.,0.,0.));
#22456=DIRECTION('',(-1.,0.,0.));
#22457=DIRECTION('',(0.,1.,0.));
#22458=DIRECTION('',(1.,0.,0.));
#22459=DIRECTION('center_axis',(0.,0.567534986670364,0.82334928123189));
#22460=DIRECTION('ref_axis',(0.,-0.82334928123189,0.567534986670364));
#22461=DIRECTION('',(1.,0.,0.));
#22462=DIRECTION('',(0.,0.82334928123189,-0.567534986670364));
#22463=DIRECTION('center_axis',(0.,-0.499999999999999,0.866025403784439));
#22464=DIRECTION('ref_axis',(1.,0.,0.));
#22465=DIRECTION('',(-1.,0.,0.));
#22466=DIRECTION('',(0.,0.866025403784439,0.499999999999999));
#22467=DIRECTION('',(1.,0.,0.));
#22468=DIRECTION('center_axis',(0.,0.0798250753770539,0.996808887069657));
#22469=DIRECTION('ref_axis',(0.,-0.996808887069657,0.0798250753770539));
#22470=DIRECTION('',(1.,0.,0.));
#22471=DIRECTION('',(0.,0.996808887069657,-0.0798250753770539));
#22472=DIRECTION('center_axis',(-1.,0.,0.));
#22473=DIRECTION('ref_axis',(0.,-0.707106781186596,0.707106781186499));
#22474=DIRECTION('center_axis',(1.,0.,0.));
#22475=DIRECTION('ref_axis',(0.,1.,0.));
#22476=DIRECTION('center_axis',(0.,-0.866025403784439,0.5));
#22477=DIRECTION('ref_axis',(0.,-0.5,-0.866025403784439));
#22478=DIRECTION('',(-1.,0.,0.));
#22479=DIRECTION('',(0.,0.5,0.866025403784439));
#22480=DIRECTION('',(1.,0.,0.));
#22481=DIRECTION('center_axis',(0.,-0.429273900399292,0.903174356608943));
#22482=DIRECTION('ref_axis',(0.,-0.903174356608943,-0.429273900399292));
#22483=DIRECTION('',(1.,0.,0.));
#22484=DIRECTION('',(0.,0.903174356608943,0.429273900399292));
#22485=DIRECTION('center_axis',(0.,0.500000000000001,-0.866025403784438));
#22486=DIRECTION('ref_axis',(-1.,0.,0.));
#22487=DIRECTION('',(-1.,0.,0.));
#22488=DIRECTION('',(0.,-0.866025403784438,-0.500000000000001));
#22489=DIRECTION('',(1.,0.,0.));
#22490=DIRECTION('center_axis',(0.,-0.0798250753770533,-0.996808887069657));
#22491=DIRECTION('ref_axis',(0.,0.996808887069657,-0.0798250753770533));
#22492=DIRECTION('',(1.,0.,0.));
#22493=DIRECTION('',(0.,-0.996808887069657,0.0798250753770533));
#22494=DIRECTION('center_axis',(0.,0.866025403784438,-0.500000000000001));
#22495=DIRECTION('ref_axis',(-1.,0.,0.));
#22496=DIRECTION('',(-1.,0.,0.));
#22497=DIRECTION('',(0.,-0.500000000000001,-0.866025403784438));
#22498=DIRECTION('',(1.,0.,0.));
#22499=DIRECTION('center_axis',(0.,0.429273900399291,-0.903174356608944));
#22500=DIRECTION('ref_axis',(0.,0.903174356608944,0.429273900399291));
#22501=DIRECTION('',(1.,0.,0.));
#22502=DIRECTION('',(0.,-0.903174356608944,-0.429273900399291));
#22503=DIRECTION('center_axis',(0.,1.,0.));
#22504=DIRECTION('ref_axis',(0.,0.,1.));
#22505=DIRECTION('',(-1.,0.,0.));
#22506=DIRECTION('',(0.,0.,-1.));
#22507=DIRECTION('',(1.,0.,0.));
#22508=DIRECTION('center_axis',(0.,0.82334928123189,-0.567534986670364));
#22509=DIRECTION('ref_axis',(0.,0.567534986670364,0.82334928123189));
#22510=DIRECTION('',(1.,0.,0.));
#22511=DIRECTION('',(0.,-0.567534986670364,-0.82334928123189));
#22512=DIRECTION('center_axis',(0.,-1.,0.));
#22513=DIRECTION('ref_axis',(0.,0.,-1.));
#22514=DIRECTION('',(-1.,0.,0.));
#22515=DIRECTION('',(0.,0.,1.));
#22516=DIRECTION('',(1.,0.,0.));
#22517=DIRECTION('center_axis',(0.,-0.82334928123189,0.567534986670365));
#22518=DIRECTION('ref_axis',(0.,-0.567534986670365,-0.82334928123189));
#22519=DIRECTION('',(1.,0.,0.));
#22520=DIRECTION('',(0.,0.567534986670365,0.82334928123189));
#22521=DIRECTION('center_axis',(0.,-0.866025403784438,-0.5));
#22522=DIRECTION('ref_axis',(-1.,0.,0.));
#22523=DIRECTION('',(-1.,0.,0.));
#22524=DIRECTION('',(0.,-0.5,0.866025403784438));
#22525=DIRECTION('',(1.,0.,0.));
#22526=DIRECTION('center_axis',(0.,-0.996808887069657,0.0798250753770534));
#22527=DIRECTION('ref_axis',(0.,-0.0798250753770534,-0.996808887069657));
#22528=DIRECTION('',(1.,0.,0.));
#22529=DIRECTION('',(0.,0.0798250753770534,0.996808887069657));
#22530=DIRECTION('center_axis',(0.,-0.500000000000001,-0.866025403784438));
#22531=DIRECTION('ref_axis',(-1.,0.,0.));
#22532=DIRECTION('',(-1.,0.,0.));
#22533=DIRECTION('',(0.,-0.866025403784438,0.500000000000001));
#22534=DIRECTION('',(1.,0.,0.));
#22535=DIRECTION('center_axis',(0.,-0.903174356608944,-0.429273900399291));
#22536=DIRECTION('ref_axis',(0.,0.429273900399291,-0.903174356608944));
#22537=DIRECTION('',(1.,0.,0.));
#22538=DIRECTION('',(0.,-0.429273900399291,0.903174356608944));
#22539=DIRECTION('center_axis',(0.,2.24737149820557E-15,-1.));
#22540=DIRECTION('ref_axis',(-1.,0.,0.));
#22541=DIRECTION('',(-1.,0.,0.));
#22542=DIRECTION('',(0.,-1.,-2.24737149820557E-15));
#22543=DIRECTION('',(1.,0.,0.));
#22544=DIRECTION('center_axis',(0.,-0.567534986670365,-0.823349281231889));
#22545=DIRECTION('ref_axis',(0.,0.823349281231889,-0.567534986670365));
#22546=DIRECTION('',(1.,0.,0.));
#22547=DIRECTION('',(0.,-0.823349281231889,0.567534986670365));
#22548=DIRECTION('center_axis',(0.,0.567534986670365,-0.82334928123189));
#22549=DIRECTION('ref_axis',(0.,0.823349281231889,0.567534986670365));
#22550=DIRECTION('',(0.,-0.823349281231889,-0.567534986670365));
#22551=DIRECTION('center_axis',(0.,0.0798250753770525,-0.996808887069657));
#22552=DIRECTION('ref_axis',(0.,0.996808887069657,0.0798250753770525));
#22553=DIRECTION('',(0.,-0.996808887069657,-0.0798250753770525));
#22554=DIRECTION('center_axis',(0.,-0.429273900399292,-0.903174356608943));
#22555=DIRECTION('ref_axis',(0.,0.903174356608943,-0.429273900399292));
#22556=DIRECTION('',(0.,-0.903174356608943,0.429273900399292));
#22557=DIRECTION('center_axis',(0.,-0.82334928123189,-0.567534986670364));
#22558=DIRECTION('ref_axis',(0.,0.567534986670364,-0.82334928123189));
#22559=DIRECTION('',(0.,-0.567534986670364,0.82334928123189));
#22560=DIRECTION('center_axis',(1.,0.,0.));
#22561=DIRECTION('ref_axis',(0.,0.,-1.));
#22562=DIRECTION('center_axis',(1.,0.,0.));
#22563=DIRECTION('ref_axis',(0.,1.,0.));
#22564=DIRECTION('center_axis',(1.,0.,0.));
#22565=DIRECTION('ref_axis',(0.,1.,0.));
#22566=DIRECTION('center_axis',(1.,0.,0.));
#22567=DIRECTION('ref_axis',(0.,1.,0.));
#22568=DIRECTION('center_axis',(1.,0.,0.));
#22569=DIRECTION('ref_axis',(0.,1.,0.));
#22570=DIRECTION('center_axis',(1.,0.,0.));
#22571=DIRECTION('ref_axis',(0.,1.,0.));
#22572=DIRECTION('center_axis',(1.,0.,0.));
#22573=DIRECTION('ref_axis',(0.,1.,0.));
#22574=DIRECTION('center_axis',(1.,0.,0.));
#22575=DIRECTION('ref_axis',(0.,1.,0.));
#22576=DIRECTION('center_axis',(1.,0.,0.));
#22577=DIRECTION('ref_axis',(0.,1.,0.));
#22578=DIRECTION('center_axis',(-1.,0.,0.));
#22579=DIRECTION('ref_axis',(0.,1.,0.));
#22580=DIRECTION('center_axis',(-1.,0.,0.));
#22581=DIRECTION('ref_axis',(0.,1.,0.));
#22582=DIRECTION('center_axis',(-1.,0.,0.));
#22583=DIRECTION('ref_axis',(0.,1.,0.));
#22584=DIRECTION('center_axis',(-1.,0.,0.));
#22585=DIRECTION('ref_axis',(0.,1.,0.));
#22586=DIRECTION('center_axis',(-1.,0.,0.));
#22587=DIRECTION('ref_axis',(0.,1.,0.));
#22588=DIRECTION('center_axis',(-1.,0.,0.));
#22589=DIRECTION('ref_axis',(0.,1.,0.));
#22590=DIRECTION('center_axis',(-1.,0.,0.));
#22591=DIRECTION('ref_axis',(0.,1.,0.));
#22592=DIRECTION('center_axis',(-1.,0.,0.));
#22593=DIRECTION('ref_axis',(0.,1.,0.));
#22594=DIRECTION('center_axis',(-1.,0.,0.));
#22595=DIRECTION('ref_axis',(0.,1.,0.));
#22596=DIRECTION('center_axis',(1.,0.,0.));
#22597=DIRECTION('ref_axis',(0.,1.,0.));
#22598=DIRECTION('center_axis',(1.,0.,0.));
#22599=DIRECTION('ref_axis',(0.,1.,0.));
#22600=DIRECTION('',(0.707106781186548,-0.707106781186547,-8.65956056235493E-17));
#22601=DIRECTION('center_axis',(-1.,0.,0.));
#22602=DIRECTION('ref_axis',(0.,1.,0.));
#22603=DIRECTION('center_axis',(1.,0.,0.));
#22604=DIRECTION('ref_axis',(0.,1.,0.));
#22605=DIRECTION('',(0.707106781186547,0.707106781186547,8.65956056235493E-17));
#22606=DIRECTION('center_axis',(-1.,0.,0.));
#22607=DIRECTION('ref_axis',(0.,1.,0.));
#22608=DIRECTION('center_axis',(0.,0.996808887069657,0.0798250753770525));
#22609=DIRECTION('ref_axis',(0.,-0.0798250753770525,0.996808887069657));
#22610=DIRECTION('',(0.,0.0798250753770525,-0.996808887069657));
#22611=DIRECTION('center_axis',(0.,0.903174356608943,-0.429273900399292));
#22612=DIRECTION('ref_axis',(0.,0.429273900399292,0.903174356608943));
#22613=DIRECTION('',(0.,-0.429273900399292,-0.903174356608943));
#22614=DIRECTION('center_axis',(0.,-0.996808887069657,-0.0798250753770546));
#22615=DIRECTION('ref_axis',(0.,0.0798250753770546,-0.996808887069657));
#22616=DIRECTION('',(0.,-0.0798250753770546,0.996808887069657));
#22617=DIRECTION('center_axis',(0.,-0.903174356608943,0.429273900399292));
#22618=DIRECTION('ref_axis',(0.,-0.429273900399292,-0.903174356608943));
#22619=DIRECTION('',(0.,0.429273900399292,0.903174356608943));
#22620=DIRECTION('center_axis',(0.,-0.567534986670364,0.82334928123189));
#22621=DIRECTION('ref_axis',(0.,-0.82334928123189,-0.567534986670364));
#22622=DIRECTION('',(0.,0.82334928123189,0.567534986670364));
#22623=DIRECTION('center_axis',(0.,-0.0798250753770534,0.996808887069657));
#22624=DIRECTION('ref_axis',(0.,-0.996808887069657,-0.0798250753770534));
#22625=DIRECTION('',(0.,0.996808887069657,0.0798250753770534));
#22626=DIRECTION('center_axis',(0.,0.429273900399292,0.903174356608943));
#22627=DIRECTION('ref_axis',(0.,-0.903174356608943,0.429273900399292));
#22628=DIRECTION('',(0.,0.903174356608943,-0.429273900399292));
#22629=DIRECTION('center_axis',(0.,0.82334928123189,0.567534986670364));
#22630=DIRECTION('ref_axis',(0.,-0.567534986670364,0.82334928123189));
#22631=DIRECTION('',(0.,0.567534986670364,-0.82334928123189));
#22632=DIRECTION('center_axis',(1.,0.,0.));
#22633=DIRECTION('ref_axis',(0.,1.,0.));
#22634=DIRECTION('',(-1.,0.,0.));
#22635=DIRECTION('center_axis',(-1.,0.,0.));
#22636=DIRECTION('ref_axis',(0.,0.,1.));
#22637=DIRECTION('center_axis',(1.,0.,0.));
#22638=DIRECTION('ref_axis',(0.,0.,-1.));
#22639=DIRECTION('center_axis',(1.,0.,0.));
#22640=DIRECTION('ref_axis',(0.,1.,0.));
#22641=DIRECTION('center_axis',(1.,0.,0.));
#22642=DIRECTION('ref_axis',(0.,0.,-1.));
#22643=DIRECTION('',(-0.707106781186547,0.707106781186548,8.65956056235494E-17));
#22644=DIRECTION('center_axis',(1.,0.,0.));
#22645=DIRECTION('ref_axis',(0.,1.,0.));
#22646=DIRECTION('center_axis',(1.,0.,0.));
#22647=DIRECTION('ref_axis',(0.,0.,-1.));
#22648=DIRECTION('',(-1.,0.,0.));
#22649=DIRECTION('center_axis',(-1.,0.,0.));
#22650=DIRECTION('ref_axis',(0.,1.,0.));
#22651=DIRECTION('center_axis',(1.,0.,0.));
#22652=DIRECTION('ref_axis',(0.,0.,-1.));
#22653=DIRECTION('',(-0.371390676354104,-0.928476690885259,-1.13705600757556E-16));
#22654=DIRECTION('center_axis',(1.,0.,0.));
#22655=DIRECTION('ref_axis',(0.,0.,-1.));
#22656=DIRECTION('axis',(0.,0.,1.));
#22657=DIRECTION('refdir',(1.,0.,0.));
#22658=DIRECTION('center_axis',(1.,0.,0.));
#22659=DIRECTION('ref_axis',(0.,-1.,1.83697019872103E-16));
#22660=DIRECTION('center_axis',(1.,0.,0.));
#22661=DIRECTION('ref_axis',(0.,1.,0.));
#22662=DIRECTION('center_axis',(1.,0.,0.));
#22663=DIRECTION('ref_axis',(0.,-1.,1.83697019872103E-16));
#22664=DIRECTION('center_axis',(1.,0.,0.));
#22665=DIRECTION('ref_axis',(0.,0.707106781186547,-0.707106781186548));
#22666=DIRECTION('',(-1.,0.,0.));
#22667=DIRECTION('center_axis',(1.,0.,0.));
#22668=DIRECTION('ref_axis',(0.,-1.,1.83697019872103E-16));
#22669=DIRECTION('',(1.,0.,0.));
#22670=DIRECTION('center_axis',(1.,0.,0.));
#22671=DIRECTION('ref_axis',(0.,-1.,1.83697019872103E-16));
#22672=DIRECTION('center_axis',(-1.,0.,0.));
#22673=DIRECTION('ref_axis',(0.,1.,0.));
#22674=DIRECTION('center_axis',(1.,0.,0.));
#22675=DIRECTION('ref_axis',(0.,1.22464679914735E-16,1.));
#22676=DIRECTION('center_axis',(1.,0.,0.));
#22677=DIRECTION('ref_axis',(0.,1.,0.));
#22678=DIRECTION('center_axis',(1.,0.,0.));
#22679=DIRECTION('ref_axis',(0.,1.22464679914735E-16,1.));
#22680=DIRECTION('center_axis',(1.,0.,0.));
#22681=DIRECTION('ref_axis',(0.,-0.707106781186548,-0.707106781186547));
#22682=DIRECTION('',(-1.,0.,0.));
#22683=DIRECTION('center_axis',(1.,0.,0.));
#22684=DIRECTION('ref_axis',(0.,1.22464679914735E-16,1.));
#22685=DIRECTION('',(1.,0.,0.));
#22686=DIRECTION('center_axis',(1.,0.,0.));
#22687=DIRECTION('ref_axis',(0.,1.22464679914735E-16,1.));
#22688=DIRECTION('center_axis',(-1.,0.,0.));
#22689=DIRECTION('ref_axis',(0.,1.,0.));
#22690=DIRECTION('center_axis',(1.,0.,0.));
#22691=DIRECTION('ref_axis',(0.,1.,-6.12323399573677E-17));
#22692=DIRECTION('center_axis',(1.,0.,0.));
#22693=DIRECTION('ref_axis',(0.,1.,0.));
#22694=DIRECTION('center_axis',(1.,0.,0.));
#22695=DIRECTION('ref_axis',(0.,1.,-6.12323399573676E-17));
#22696=DIRECTION('center_axis',(1.,0.,0.));
#22697=DIRECTION('ref_axis',(0.,-0.707106781186547,0.707106781186548));
#22698=DIRECTION('',(-1.,0.,0.));
#22699=DIRECTION('center_axis',(1.,0.,0.));
#22700=DIRECTION('ref_axis',(0.,1.,-6.12323399573676E-17));
#22701=DIRECTION('',(1.,0.,0.));
#22702=DIRECTION('center_axis',(1.,0.,0.));
#22703=DIRECTION('ref_axis',(0.,1.,-6.12323399573677E-17));
#22704=DIRECTION('center_axis',(-1.,0.,0.));
#22705=DIRECTION('ref_axis',(0.,1.,0.));
#22706=DIRECTION('center_axis',(1.,0.,0.));
#22707=DIRECTION('ref_axis',(0.,0.,-1.));
#22708=DIRECTION('center_axis',(1.,0.,0.));
#22709=DIRECTION('ref_axis',(0.,1.,0.));
#22710=DIRECTION('center_axis',(1.,0.,0.));
#22711=DIRECTION('ref_axis',(0.,0.,-1.));
#22712=DIRECTION('center_axis',(1.,0.,0.));
#22713=DIRECTION('ref_axis',(0.,0.707106781186548,0.707106781186547));
#22714=DIRECTION('',(-1.,0.,0.));
#22715=DIRECTION('center_axis',(1.,0.,0.));
#22716=DIRECTION('ref_axis',(0.,0.,-1.));
#22717=DIRECTION('',(1.,0.,0.));
#22718=DIRECTION('center_axis',(1.,0.,0.));
#22719=DIRECTION('ref_axis',(0.,0.,-1.));
#22720=DIRECTION('center_axis',(-1.,0.,0.));
#22721=DIRECTION('ref_axis',(0.,1.,0.));
#22722=DIRECTION('center_axis',(0.,-1.,1.83697019872103E-16));
#22723=DIRECTION('ref_axis',(1.,0.,0.));
#22724=DIRECTION('',(0.,-1.,1.83697019872103E-16));
#22725=DIRECTION('center_axis',(0.,1.22464679914735E-16,1.));
#22726=DIRECTION('ref_axis',(1.,0.,0.));
#22727=DIRECTION('',(0.,1.22464679914735E-16,1.));
#22728=DIRECTION('center_axis',(0.,1.,-6.12323399573677E-17));
#22729=DIRECTION('ref_axis',(1.,0.,0.));
#22730=DIRECTION('',(0.,1.,-6.12323399573677E-17));
#22731=DIRECTION('center_axis',(0.,0.,-1.));
#22732=DIRECTION('ref_axis',(1.,0.,0.));
#22733=DIRECTION('',(0.,0.,-1.));
#22734=DIRECTION('center_axis',(1.,0.,0.));
#22735=DIRECTION('ref_axis',(0.,1.,0.));
#22736=DIRECTION('center_axis',(1.,0.,0.));
#22737=DIRECTION('ref_axis',(0.,0.,-1.));
#22738=DIRECTION('',(1.,0.,0.));
#22739=DIRECTION('',(1.,0.,0.));
#22740=DIRECTION('center_axis',(1.,0.,0.));
#22741=DIRECTION('ref_axis',(0.,0.,-1.));
#22742=DIRECTION('center_axis',(-1.,0.,0.));
#22743=DIRECTION('ref_axis',(0.,0.,1.));
#22744=DIRECTION('center_axis',(-1.,0.,0.));
#22745=DIRECTION('ref_axis',(0.,1.,0.));
#22746=DIRECTION('center_axis',(1.,0.,0.));
#22747=DIRECTION('ref_axis',(0.,0.,-1.));
#22748=DIRECTION('center_axis',(1.,0.,0.));
#22749=DIRECTION('ref_axis',(0.,1.,0.));
#22750=DIRECTION('center_axis',(1.,0.,0.));
#22751=DIRECTION('ref_axis',(0.,1.,0.));
#22752=DIRECTION('center_axis',(1.,0.,0.));
#22753=DIRECTION('ref_axis',(0.,0.,-1.));
#22754=DIRECTION('',(-1.,0.,0.));
#22755=DIRECTION('center_axis',(1.,0.,0.));
#22756=DIRECTION('ref_axis',(0.,1.,0.));
#22757=DIRECTION('center_axis',(1.,0.,0.));
#22758=DIRECTION('ref_axis',(0.,0.,-1.));
#22759=DIRECTION('',(-0.707106781186547,0.707106781186548,8.65956056235494E-17));
#22760=DIRECTION('center_axis',(1.,0.,0.));
#22761=DIRECTION('ref_axis',(0.,0.,-1.));
#22762=DIRECTION('center_axis',(1.,0.,0.));
#22763=DIRECTION('ref_axis',(0.,1.,0.));
#22764=DIRECTION('',(-1.,0.,0.));
#22765=DIRECTION('center_axis',(-1.,0.,0.));
#22766=DIRECTION('ref_axis',(0.,1.,0.));
#22767=DIRECTION('center_axis',(1.,0.,0.));
#22768=DIRECTION('ref_axis',(0.,0.,-1.));
#22769=DIRECTION('',(-0.707106781186548,-0.707106781186548,-8.65956056235493E-17));
#22770=DIRECTION('center_axis',(1.,0.,0.));
#22771=DIRECTION('ref_axis',(0.,0.,-1.));
#22772=DIRECTION('center_axis',(1.,0.,0.));
#22773=DIRECTION('ref_axis',(0.,0.,-1.));
#22774=DIRECTION('center_axis',(1.,0.,0.));
#22775=DIRECTION('ref_axis',(0.,1.,0.));
#22776=DIRECTION('',(-0.707106781186546,0.707106781186549,8.65956056235495E-17));
#22777=DIRECTION('center_axis',(1.,0.,0.));
#22778=DIRECTION('ref_axis',(0.,0.,-1.));
#22779=DIRECTION('center_axis',(1.,0.,0.));
#22780=DIRECTION('ref_axis',(0.,1.,0.));
#22781=DIRECTION('',(-1.,0.,0.));
#22782=DIRECTION('',(-1.,0.,0.));
#22783=DIRECTION('center_axis',(1.,0.,0.));
#22784=DIRECTION('ref_axis',(0.,0.,-1.));
#22785=DIRECTION('center_axis',(-1.,0.,0.));
#22786=DIRECTION('ref_axis',(0.,1.,0.));
#22787=DIRECTION('',(-0.707106781186546,-0.707106781186549,-8.65956056235495E-17));
#22788=DIRECTION('center_axis',(1.,0.,0.));
#22789=DIRECTION('ref_axis',(0.,0.,-1.));
#22790=DIRECTION('center_axis',(-1.,0.,0.));
#22791=DIRECTION('ref_axis',(0.,0.,1.));
#22792=DIRECTION('axis',(0.,0.,1.));
#22793=DIRECTION('refdir',(1.,0.,0.));
#22794=DIRECTION('center_axis',(-1.,0.,0.));
#22795=DIRECTION('ref_axis',(0.,0.,-1.));
#22796=DIRECTION('center_axis',(-1.,0.,0.));
#22797=DIRECTION('ref_axis',(0.,0.,-1.));
#22798=DIRECTION('',(0.707106781186547,-8.65956056235494E-17,-0.707106781186548));
#22799=DIRECTION('center_axis',(1.,0.,0.));
#22800=DIRECTION('ref_axis',(0.,0.,-1.));
#22801=DIRECTION('center_axis',(1.,0.,0.));
#22802=DIRECTION('ref_axis',(0.,0.,-1.));
#22803=DIRECTION('',(1.,0.,0.));
#22804=DIRECTION('center_axis',(-1.,0.,0.));
#22805=DIRECTION('ref_axis',(0.,0.,-1.));
#22806=DIRECTION('center_axis',(1.,0.,0.));
#22807=DIRECTION('ref_axis',(0.,0.,-1.));
#22808=DIRECTION('',(0.,-0.275637355816999,0.961261695938319));
#22809=DIRECTION('',(0.,0.923879532511287,0.382683432365089));
#22810=DIRECTION('',(0.,0.48480962024634,-0.874619707139394));
#22811=DIRECTION('',(0.,0.856292125836473,0.516491815259888));
#22812=DIRECTION('',(0.,0.816221627432192,0.577738915871126));
#22813=DIRECTION('',(0.,0.771778750427187,0.635891154513923));
#22814=DIRECTION('',(0.,0.723201568743836,0.690637018242183));
#22815=DIRECTION('',(0.,0.670750303163526,0.741683241556689));
#22816=DIRECTION('',(0.,0.614705927362395,0.788756377385019));
#22817=DIRECTION('',(0.,0.555368662776888,0.831604261897095));
#22818=DIRECTION('',(0.,0.493056370361897,0.869997365309546));
#22819=DIRECTION('',(0.,0.428102847856614,0.903730021442829));
#22820=DIRECTION('',(0.,0.360856041679385,0.932621529444547));
#22821=DIRECTION('',(0.,0.291676183030194,0.956517121777199));
#22822=DIRECTION('',(0.,0.22093385818535,0.975288793285012));
#22823=DIRECTION('',(0.,0.14900802332161,0.98883598689863));
#22824=DIRECTION('',(0.,0.0762839745039533,0.997086132304467));
#22825=DIRECTION('',(0.,0.00315128371150461,0.999995034693158));
#22826=DIRECTION('',(0.,-0.069998288041949,0.997547111504613));
#22827=DIRECTION('',(0.,-0.142772889313813,0.98975547590149));
#22828=DIRECTION('',(0.,-0.214782677322933,0.976661866523923));
#22829=DIRECTION('',(0.,-0.285641906279744,0.958336423901791));
#22830=DIRECTION('',(0.,-0.354970993769443,0.934877314722276));
#22831=DIRECTION('',(0.,-0.422398554118871,0.906410205965427));
#22832=DIRECTION('',(0.,-0.487563387854682,0.873087591724716));
#22833=DIRECTION('',(0.,-0.550116416595493,0.835087976318743));
#22834=DIRECTION('',(0.,-0.609722553013204,0.792614918069967));
#22835=DIRECTION('',(0.,-0.666062495846264,0.745895938872873));
#22836=DIRECTION('',(0.,-0.718834440349327,0.695181305392823));
#22837=DIRECTION('',(0.,-0.767755695016677,0.640742688424503));
#22838=DIRECTION('',(0.,-0.812564195918804,0.582871707591668));
#22839=DIRECTION('',(0.,-0.853019910540169,0.521878369183895));
#22840=DIRECTION('',(0.,-0.888906123597886,0.458089405498731));
#22841=DIRECTION('',(0.,-0.920030597953456,0.39184652458508));
#22842=DIRECTION('',(0.,-0.946226604398715,0.323504579763685));
#22843=DIRECTION('',(0.,-0.967353814799542,0.253429668730349));
#22844=DIRECTION('',(0.,-0.983299053812935,0.181997172424701));
#22845=DIRECTION('',(0.,-0.993976905150596,0.109589744169988));
#22846=DIRECTION('',(0.,-0.999330169141354,0.0365952598557893));
#22847=DIRECTION('',(0.,-0.999330169141354,-0.0365952598557893));
#22848=DIRECTION('',(0.,-0.993976905150596,-0.109589744169987));
#22849=DIRECTION('',(0.,-0.983299053812935,-0.181997172424701));
#22850=DIRECTION('',(0.,-0.967353814799542,-0.253429668730349));
#22851=DIRECTION('',(0.,-0.946226604398715,-0.323504579763685));
#22852=DIRECTION('',(0.,-0.920030597953456,-0.39184652458508));
#22853=DIRECTION('',(0.,-0.888906123597886,-0.458089405498731));
#22854=DIRECTION('',(0.,-0.85301991054017,-0.521878369183893));
#22855=DIRECTION('',(0.,-0.812564195918805,-0.582871707591668));
#22856=DIRECTION('',(0.,-0.767755695016675,-0.640742688424505));
#22857=DIRECTION('',(0.,-0.71883444034933,-0.69518130539282));
#22858=DIRECTION('',(0.,-0.666062495846262,-0.745895938872875));
#22859=DIRECTION('',(0.,-0.609722553013205,-0.792614918069966));
#22860=DIRECTION('',(0.,-0.550116416595494,-0.835087976318742));
#22861=DIRECTION('',(0.,-0.48756338785468,-0.873087591724717));
#22862=DIRECTION('',(0.,-0.422398554118875,-0.906410205965425));
#22863=DIRECTION('',(0.,-0.354970993769442,-0.934877314722277));
#22864=DIRECTION('',(0.,-0.285641906279744,-0.958336423901791));
#22865=DIRECTION('',(0.,-0.214782677322933,-0.976661866523923));
#22866=DIRECTION('',(0.,-0.142772889313813,-0.98975547590149));
#22867=DIRECTION('',(0.,-0.0699982880419509,-0.997547111504613));
#22868=DIRECTION('',(0.,0.00315128371150461,-0.999995034693158));
#22869=DIRECTION('',(0.,0.0762839745039523,-0.997086132304467));
#22870=DIRECTION('',(0.,0.14900802332161,-0.98883598689863));
#22871=DIRECTION('',(0.,0.220933858185349,-0.975288793285013));
#22872=DIRECTION('',(0.,0.291676183030194,-0.956517121777199));
#22873=DIRECTION('',(0.,0.360856041679387,-0.932621529444546));
#22874=DIRECTION('',(0.,0.428102847856613,-0.90373002144283));
#22875=DIRECTION('',(0.,0.493056370361895,-0.869997365309547));
#22876=DIRECTION('',(0.,0.555368662776888,-0.831604261897095));
#22877=DIRECTION('',(0.,0.614705927362394,-0.788756377385019));
#22878=DIRECTION('',(0.,0.670750303163526,-0.741683241556689));
#22879=DIRECTION('',(0.,0.723201568743836,-0.690637018242184));
#22880=DIRECTION('',(0.,0.771778750427186,-0.635891154513924));
#22881=DIRECTION('',(0.,0.816221627432192,-0.577738915871126));
#22882=DIRECTION('',(0.,0.856292125836472,-0.516491815259888));
#22883=DIRECTION('',(0.,0.484809620246337,0.874619707139396));
#22884=DIRECTION('',(0.,0.923879532511286,-0.382683432365091));
#22885=DIRECTION('',(0.,-0.275637355817,-0.961261695938319));
#22886=DIRECTION('',(0.,-0.94954718849933,0.313624196791349));
#22887=DIRECTION('',(0.,-0.921637548163022,0.388051839083456));
#22888=DIRECTION('',(0.,-0.887904612902449,0.460027606113537));
#22889=DIRECTION('',(0.,-0.848561521636558,0.529096724614553));
#22890=DIRECTION('',(0.,-0.803856860617217,0.594822786751342));
#22891=DIRECTION('',(0.,-0.754073092756362,0.656790507529498));
#22892=DIRECTION('',(0.,-0.699524772906136,0.714608348741196));
#22893=DIRECTION('',(0.,-0.640556560368615,0.767910992868789));
#22894=DIRECTION('',(0.,-0.577541041192885,0.816361651315052));
#22895=DIRECTION('',(0.,-0.51087637401918,0.85965419237564));
#22896=DIRECTION('',(0.,-0.44098377434459,0.897515075508373));
#22897=DIRECTION('',(0.,-0.368304853105793,0.929705079677808));
#22898=DIRECTION('',(0.,-0.293298826394844,0.95602081485468));
#22899=DIRECTION('',(0.,-0.2164396139381,0.976296007119934));
#22900=DIRECTION('',(0.,-0.138212844671456,0.990402549253496));
#22901=DIRECTION('',(0.,-0.0591127883317614,0.998251310169761));
#22902=DIRECTION('',(0.,0.0203607675478923,0.999792698085389));
#22903=DIRECTION('',(0.,0.0997056755067372,0.995016973861122));
#22904=DIRECTION('',(0.,0.178420600935832,0.983954312537781));
#22905=DIRECTION('',(0.,0.256008189721705,0.966674612677614));
#22906=DIRECTION('',(0.,0.331978210739482,0.943287054715696));
#22907=DIRECTION('',(0.,0.405850653339991,0.913939411111865));
#22908=DIRECTION('',(0.,0.47715876025961,0.878817112661964));
#22909=DIRECTION('',(0.,0.545451976789583,0.83814207686784));
#22910=DIRECTION('',(0.,0.610298797570814,0.792171305768909));
#22911=DIRECTION('',(0.,0.671289493026783,0.741195262094844));
#22912=DIRECTION('',(0.,0.728038698207918,0.685536033999469));
#22913=DIRECTION('',(0.,0.780187847689935,0.62554529997191));
#22914=DIRECTION('',(0.,0.827407441141511,0.561602106783492));
#22915=DIRECTION('',(0.,0.869399125246396,0.494110474510307));
#22916=DIRECTION('',(0.,0.905897578825568,0.423496843763887));
#22917=DIRECTION('',(0.,0.936672189248398,0.350207381259467));
#22918=DIRECTION('',(0.,0.96152850954055,0.274705160746442));
#22919=DIRECTION('',(0.,0.980309486982024,0.197467237112997));
#22920=DIRECTION('',(0.,0.992896455432508,0.118981632152029));
#22921=DIRECTION('',(0.,0.999209885114126,0.0397442510335229));
#22922=DIRECTION('',(0.,0.999209885114126,-0.0397442510335258));
#22923=DIRECTION('',(0.,0.992896455432509,-0.118981632152026));
#22924=DIRECTION('',(0.,0.980309486982024,-0.197467237112996));
#22925=DIRECTION('',(0.,0.961528509540549,-0.274705160746445));
#22926=DIRECTION('',(0.,0.936672189248397,-0.350207381259469));
#22927=DIRECTION('',(0.,0.90589757882557,-0.423496843763883));
#22928=DIRECTION('',(0.,0.869399125246396,-0.494110474510309));
#22929=DIRECTION('',(0.,0.827407441141511,-0.561602106783492));
#22930=DIRECTION('',(0.,0.780187847689935,-0.62554529997191));
#22931=DIRECTION('',(0.,0.728038698207917,-0.685536033999469));
#22932=DIRECTION('',(0.,0.671289493026782,-0.741195262094845));
#22933=DIRECTION('',(0.,0.610298797570813,-0.79217130576891));
#22934=DIRECTION('',(0.,0.545451976789582,-0.83814207686784));
#22935=DIRECTION('',(0.,0.477158760259606,-0.878817112661967));
#22936=DIRECTION('',(0.,0.405850653339993,-0.913939411111864));
#22937=DIRECTION('',(0.,0.33197821073948,-0.943287054715696));
#22938=DIRECTION('',(0.,0.256008189721705,-0.966674612677614));
#22939=DIRECTION('',(0.,0.178420600935832,-0.983954312537781));
#22940=DIRECTION('',(0.,0.0997056755067357,-0.995016973861122));
#22941=DIRECTION('',(0.,0.0203607675478923,-0.999792698085389));
#22942=DIRECTION('',(0.,-0.0591127883317644,-0.998251310169761));
#22943=DIRECTION('',(0.,-0.138212844671453,-0.990402549253497));
#22944=DIRECTION('',(0.,-0.216439613938106,-0.976296007119933));
#22945=DIRECTION('',(0.,-0.293298826394842,-0.956020814854681));
#22946=DIRECTION('',(0.,-0.368304853105795,-0.929705079677808));
#22947=DIRECTION('',(0.,-0.44098377434459,-0.897515075508373));
#22948=DIRECTION('',(0.,-0.510876374019181,-0.85965419237564));
#22949=DIRECTION('',(0.,-0.577541041192886,-0.816361651315051));
#22950=DIRECTION('',(0.,-0.640556560368615,-0.767910992868789));
#22951=DIRECTION('',(0.,-0.699524772906137,-0.714608348741195));
#22952=DIRECTION('',(0.,-0.754073092756361,-0.656790507529498));
#22953=DIRECTION('',(0.,-0.803856860617218,-0.59482278675134));
#22954=DIRECTION('',(0.,-0.848561521636558,-0.529096724614554));
#22955=DIRECTION('',(0.,-0.88790461290245,-0.460027606113536));
#22956=DIRECTION('',(0.,-0.921637548163023,-0.388051839083454));
#22957=DIRECTION('',(0.,-0.94954718849933,-0.313624196791348));
#22958=DIRECTION('center_axis',(-1.,0.,0.));
#22959=DIRECTION('ref_axis',(0.,0.,-1.));
#22960=DIRECTION('center_axis',(1.,0.,0.));
#22961=DIRECTION('ref_axis',(0.,0.,-1.));
#22962=DIRECTION('center_axis',(1.,0.,0.));
#22963=DIRECTION('ref_axis',(0.,0.,-1.));
#22964=DIRECTION('',(-0.707106781186547,8.65956056235494E-17,-0.707106781186548));
#22965=DIRECTION('center_axis',(1.,0.,0.));
#22966=DIRECTION('ref_axis',(0.,0.,-1.));
#22967=DIRECTION('',(0.,-0.275637355816999,0.961261695938319));
#22968=DIRECTION('',(0.,-0.94954718849933,-0.313624196791348));
#22969=DIRECTION('',(0.,-0.921637548163023,-0.388051839083454));
#22970=DIRECTION('',(0.,-0.88790461290245,-0.460027606113536));
#22971=DIRECTION('',(0.,-0.848561521636558,-0.529096724614554));
#22972=DIRECTION('',(0.,-0.803856860617218,-0.59482278675134));
#22973=DIRECTION('',(0.,-0.754073092756361,-0.656790507529498));
#22974=DIRECTION('',(0.,-0.699524772906137,-0.714608348741195));
#22975=DIRECTION('',(0.,-0.640556560368615,-0.767910992868789));
#22976=DIRECTION('',(0.,-0.577541041192886,-0.816361651315051));
#22977=DIRECTION('',(0.,-0.510876374019181,-0.85965419237564));
#22978=DIRECTION('',(0.,-0.44098377434459,-0.897515075508373));
#22979=DIRECTION('',(0.,-0.368304853105795,-0.929705079677808));
#22980=DIRECTION('',(0.,-0.293298826394842,-0.956020814854681));
#22981=DIRECTION('',(0.,-0.216439613938106,-0.976296007119933));
#22982=DIRECTION('',(0.,-0.138212844671453,-0.990402549253497));
#22983=DIRECTION('',(0.,-0.0591127883317644,-0.998251310169761));
#22984=DIRECTION('',(0.,0.0203607675478923,-0.999792698085389));
#22985=DIRECTION('',(0.,0.0997056755067357,-0.995016973861122));
#22986=DIRECTION('',(0.,0.178420600935832,-0.983954312537781));
#22987=DIRECTION('',(0.,0.256008189721705,-0.966674612677614));
#22988=DIRECTION('',(0.,0.33197821073948,-0.943287054715696));
#22989=DIRECTION('',(0.,0.405850653339993,-0.913939411111864));
#22990=DIRECTION('',(0.,0.477158760259606,-0.878817112661967));
#22991=DIRECTION('',(0.,0.545451976789582,-0.83814207686784));
#22992=DIRECTION('',(0.,0.610298797570813,-0.79217130576891));
#22993=DIRECTION('',(0.,0.671289493026782,-0.741195262094845));
#22994=DIRECTION('',(0.,0.728038698207917,-0.685536033999469));
#22995=DIRECTION('',(0.,0.780187847689935,-0.62554529997191));
#22996=DIRECTION('',(0.,0.827407441141511,-0.561602106783492));
#22997=DIRECTION('',(0.,0.869399125246396,-0.494110474510309));
#22998=DIRECTION('',(0.,0.90589757882557,-0.423496843763883));
#22999=DIRECTION('',(0.,0.936672189248397,-0.350207381259469));
#23000=DIRECTION('',(0.,0.961528509540549,-0.274705160746445));
#23001=DIRECTION('',(0.,0.980309486982024,-0.197467237112996));
#23002=DIRECTION('',(0.,0.992896455432509,-0.118981632152026));
#23003=DIRECTION('',(0.,0.999209885114126,-0.0397442510335258));
#23004=DIRECTION('',(0.,0.999209885114126,0.0397442510335229));
#23005=DIRECTION('',(0.,0.992896455432508,0.118981632152029));
#23006=DIRECTION('',(0.,0.980309486982024,0.197467237112997));
#23007=DIRECTION('',(0.,0.96152850954055,0.274705160746442));
#23008=DIRECTION('',(0.,0.936672189248398,0.350207381259467));
#23009=DIRECTION('',(0.,0.905897578825568,0.423496843763887));
#23010=DIRECTION('',(0.,0.869399125246396,0.494110474510307));
#23011=DIRECTION('',(0.,0.827407441141511,0.561602106783492));
#23012=DIRECTION('',(0.,0.780187847689935,0.62554529997191));
#23013=DIRECTION('',(0.,0.728038698207918,0.685536033999469));
#23014=DIRECTION('',(0.,0.671289493026783,0.741195262094844));
#23015=DIRECTION('',(0.,0.610298797570814,0.792171305768909));
#23016=DIRECTION('',(0.,0.545451976789583,0.83814207686784));
#23017=DIRECTION('',(0.,0.47715876025961,0.878817112661964));
#23018=DIRECTION('',(0.,0.405850653339991,0.913939411111865));
#23019=DIRECTION('',(0.,0.331978210739482,0.943287054715696));
#23020=DIRECTION('',(0.,0.256008189721705,0.966674612677614));
#23021=DIRECTION('',(0.,0.178420600935832,0.983954312537781));
#23022=DIRECTION('',(0.,0.0997056755067372,0.995016973861122));
#23023=DIRECTION('',(0.,0.0203607675478923,0.999792698085389));
#23024=DIRECTION('',(0.,-0.0591127883317614,0.998251310169761));
#23025=DIRECTION('',(0.,-0.138212844671456,0.990402549253496));
#23026=DIRECTION('',(0.,-0.2164396139381,0.976296007119934));
#23027=DIRECTION('',(0.,-0.293298826394844,0.95602081485468));
#23028=DIRECTION('',(0.,-0.368304853105793,0.929705079677808));
#23029=DIRECTION('',(0.,-0.44098377434459,0.897515075508373));
#23030=DIRECTION('',(0.,-0.51087637401918,0.85965419237564));
#23031=DIRECTION('',(0.,-0.577541041192885,0.816361651315052));
#23032=DIRECTION('',(0.,-0.640556560368615,0.767910992868789));
#23033=DIRECTION('',(0.,-0.699524772906136,0.714608348741196));
#23034=DIRECTION('',(0.,-0.754073092756362,0.656790507529498));
#23035=DIRECTION('',(0.,-0.803856860617217,0.594822786751342));
#23036=DIRECTION('',(0.,-0.848561521636558,0.529096724614553));
#23037=DIRECTION('',(0.,-0.887904612902449,0.460027606113537));
#23038=DIRECTION('',(0.,-0.921637548163022,0.388051839083456));
#23039=DIRECTION('',(0.,-0.94954718849933,0.313624196791349));
#23040=DIRECTION('',(0.,-0.275637355817,-0.961261695938319));
#23041=DIRECTION('',(0.,0.923879532511286,-0.382683432365091));
#23042=DIRECTION('',(0.,0.484809620246337,0.874619707139396));
#23043=DIRECTION('',(0.,0.856292125836473,-0.516491815259889));
#23044=DIRECTION('',(0.,0.816221627432192,-0.577738915871126));
#23045=DIRECTION('',(0.,0.771778750427186,-0.635891154513924));
#23046=DIRECTION('',(0.,0.723201568743836,-0.690637018242184));
#23047=DIRECTION('',(0.,0.670750303163526,-0.741683241556689));
#23048=DIRECTION('',(0.,0.614705927362394,-0.788756377385019));
#23049=DIRECTION('',(0.,0.555368662776888,-0.831604261897095));
#23050=DIRECTION('',(0.,0.493056370361895,-0.869997365309547));
#23051=DIRECTION('',(0.,0.428102847856613,-0.90373002144283));
#23052=DIRECTION('',(0.,0.360856041679387,-0.932621529444546));
#23053=DIRECTION('',(0.,0.291676183030194,-0.956517121777199));
#23054=DIRECTION('',(0.,0.220933858185349,-0.975288793285013));
#23055=DIRECTION('',(0.,0.14900802332161,-0.98883598689863));
#23056=DIRECTION('',(0.,0.0762839745039523,-0.997086132304467));
#23057=DIRECTION('',(0.,0.00315128371150461,-0.999995034693158));
#23058=DIRECTION('',(0.,-0.0699982880419509,-0.997547111504613));
#23059=DIRECTION('',(0.,-0.142772889313813,-0.98975547590149));
#23060=DIRECTION('',(0.,-0.214782677322933,-0.976661866523923));
#23061=DIRECTION('',(0.,-0.285641906279744,-0.958336423901791));
#23062=DIRECTION('',(0.,-0.354970993769442,-0.934877314722277));
#23063=DIRECTION('',(0.,-0.422398554118875,-0.906410205965425));
#23064=DIRECTION('',(0.,-0.48756338785468,-0.873087591724717));
#23065=DIRECTION('',(0.,-0.550116416595494,-0.835087976318742));
#23066=DIRECTION('',(0.,-0.609722553013205,-0.792614918069966));
#23067=DIRECTION('',(0.,-0.666062495846262,-0.745895938872875));
#23068=DIRECTION('',(0.,-0.71883444034933,-0.69518130539282));
#23069=DIRECTION('',(0.,-0.767755695016675,-0.640742688424505));
#23070=DIRECTION('',(0.,-0.812564195918805,-0.582871707591668));
#23071=DIRECTION('',(0.,-0.85301991054017,-0.521878369183893));
#23072=DIRECTION('',(0.,-0.888906123597886,-0.458089405498731));
#23073=DIRECTION('',(0.,-0.920030597953456,-0.39184652458508));
#23074=DIRECTION('',(0.,-0.946226604398715,-0.323504579763685));
#23075=DIRECTION('',(0.,-0.967353814799542,-0.253429668730349));
#23076=DIRECTION('',(0.,-0.983299053812935,-0.181997172424701));
#23077=DIRECTION('',(0.,-0.993976905150596,-0.109589744169987));
#23078=DIRECTION('',(0.,-0.999330169141354,-0.0365952598557893));
#23079=DIRECTION('',(0.,-0.999330169141354,0.0365952598557893));
#23080=DIRECTION('',(0.,-0.993976905150596,0.109589744169988));
#23081=DIRECTION('',(0.,-0.983299053812935,0.181997172424701));
#23082=DIRECTION('',(0.,-0.967353814799542,0.253429668730349));
#23083=DIRECTION('',(0.,-0.946226604398715,0.323504579763685));
#23084=DIRECTION('',(0.,-0.920030597953456,0.39184652458508));
#23085=DIRECTION('',(0.,-0.888906123597886,0.458089405498731));
#23086=DIRECTION('',(0.,-0.853019910540169,0.521878369183895));
#23087=DIRECTION('',(0.,-0.812564195918804,0.582871707591668));
#23088=DIRECTION('',(0.,-0.767755695016677,0.640742688424503));
#23089=DIRECTION('',(0.,-0.718834440349327,0.695181305392823));
#23090=DIRECTION('',(0.,-0.666062495846264,0.745895938872873));
#23091=DIRECTION('',(0.,-0.609722553013204,0.792614918069967));
#23092=DIRECTION('',(0.,-0.550116416595493,0.835087976318743));
#23093=DIRECTION('',(0.,-0.487563387854682,0.873087591724716));
#23094=DIRECTION('',(0.,-0.422398554118871,0.906410205965427));
#23095=DIRECTION('',(0.,-0.354970993769443,0.934877314722276));
#23096=DIRECTION('',(0.,-0.285641906279744,0.958336423901791));
#23097=DIRECTION('',(0.,-0.214782677322933,0.976661866523923));
#23098=DIRECTION('',(0.,-0.142772889313813,0.98975547590149));
#23099=DIRECTION('',(0.,-0.069998288041949,0.997547111504613));
#23100=DIRECTION('',(0.,0.00315128371150461,0.999995034693158));
#23101=DIRECTION('',(0.,0.0762839745039533,0.997086132304467));
#23102=DIRECTION('',(0.,0.14900802332161,0.98883598689863));
#23103=DIRECTION('',(0.,0.22093385818535,0.975288793285012));
#23104=DIRECTION('',(0.,0.291676183030194,0.956517121777199));
#23105=DIRECTION('',(0.,0.360856041679385,0.932621529444547));
#23106=DIRECTION('',(0.,0.428102847856614,0.903730021442829));
#23107=DIRECTION('',(0.,0.493056370361897,0.869997365309546));
#23108=DIRECTION('',(0.,0.555368662776888,0.831604261897095));
#23109=DIRECTION('',(0.,0.614705927362395,0.788756377385019));
#23110=DIRECTION('',(0.,0.670750303163526,0.741683241556689));
#23111=DIRECTION('',(0.,0.723201568743836,0.690637018242183));
#23112=DIRECTION('',(0.,0.771778750427187,0.635891154513923));
#23113=DIRECTION('',(0.,0.816221627432192,0.577738915871126));
#23114=DIRECTION('',(0.,0.856292125836473,0.516491815259888));
#23115=DIRECTION('',(0.,0.48480962024634,-0.874619707139394));
#23116=DIRECTION('',(0.,0.923879532511287,0.382683432365089));
#23117=DIRECTION('center_axis',(1.,0.,0.));
#23118=DIRECTION('ref_axis',(0.,0.,-1.));
#23119=DIRECTION('center_axis',(-1.,0.,0.));
#23120=DIRECTION('ref_axis',(0.,0.,-1.));
#23121=DIRECTION('',(0.707106781186547,-8.65956056235494E-17,-0.707106781186548));
#23122=DIRECTION('center_axis',(1.,0.,0.));
#23123=DIRECTION('ref_axis',(0.,0.,-1.));
#23124=DIRECTION('center_axis',(1.,0.,0.));
#23125=DIRECTION('ref_axis',(0.,0.,-1.));
#23126=DIRECTION('',(1.,0.,0.));
#23127=DIRECTION('center_axis',(-1.,0.,0.));
#23128=DIRECTION('ref_axis',(0.,0.,-1.));
#23129=DIRECTION('center_axis',(1.,0.,0.));
#23130=DIRECTION('ref_axis',(0.,0.,-1.));
#23131=DIRECTION('',(-0.707106781186547,8.65956056235494E-17,-0.707106781186548));
#23132=DIRECTION('center_axis',(0.,0.382683432365089,-0.923879532511287));
#23133=DIRECTION('ref_axis',(0.,0.923879532511287,0.382683432365089));
#23134=DIRECTION('',(1.,0.,0.));
#23135=DIRECTION('',(1.,0.,0.));
#23136=DIRECTION('center_axis',(0.,-0.874619707139394,-0.48480962024634));
#23137=DIRECTION('ref_axis',(0.,0.48480962024634,-0.874619707139394));
#23138=DIRECTION('',(1.,0.,0.));
#23139=DIRECTION('center_axis',(0.,0.516491815259888,-0.856292125836473));
#23140=DIRECTION('ref_axis',(0.,0.856292125836473,0.516491815259888));
#23141=DIRECTION('',(1.,0.,0.));
#23142=DIRECTION('center_axis',(0.,0.577738915871126,-0.816221627432192));
#23143=DIRECTION('ref_axis',(0.,0.816221627432192,0.577738915871126));
#23144=DIRECTION('',(1.,0.,0.));
#23145=DIRECTION('center_axis',(0.,0.635891154513923,-0.771778750427187));
#23146=DIRECTION('ref_axis',(0.,0.771778750427187,0.635891154513923));
#23147=DIRECTION('',(1.,0.,0.));
#23148=DIRECTION('center_axis',(0.,0.690637018242184,-0.723201568743836));
#23149=DIRECTION('ref_axis',(0.,0.723201568743836,0.690637018242183));
#23150=DIRECTION('',(1.,0.,0.));
#23151=DIRECTION('center_axis',(0.,0.741683241556689,-0.670750303163526));
#23152=DIRECTION('ref_axis',(0.,0.670750303163526,0.741683241556689));
#23153=DIRECTION('',(1.,0.,0.));
#23154=DIRECTION('center_axis',(0.,0.788756377385019,-0.614705927362395));
#23155=DIRECTION('ref_axis',(0.,0.614705927362395,0.788756377385019));
#23156=DIRECTION('',(1.,0.,0.));
#23157=DIRECTION('center_axis',(0.,0.831604261897095,-0.555368662776888));
#23158=DIRECTION('ref_axis',(0.,0.555368662776888,0.831604261897095));
#23159=DIRECTION('',(1.,0.,0.));
#23160=DIRECTION('center_axis',(0.,0.869997365309546,-0.493056370361897));
#23161=DIRECTION('ref_axis',(0.,0.493056370361897,0.869997365309546));
#23162=DIRECTION('',(1.,0.,0.));
#23163=DIRECTION('center_axis',(0.,0.903730021442829,-0.428102847856614));
#23164=DIRECTION('ref_axis',(0.,0.428102847856614,0.903730021442829));
#23165=DIRECTION('',(1.,0.,0.));
#23166=DIRECTION('center_axis',(0.,0.932621529444547,-0.360856041679385));
#23167=DIRECTION('ref_axis',(0.,0.360856041679385,0.932621529444547));
#23168=DIRECTION('',(1.,0.,0.));
#23169=DIRECTION('center_axis',(0.,0.956517121777199,-0.291676183030194));
#23170=DIRECTION('ref_axis',(0.,0.291676183030194,0.956517121777199));
#23171=DIRECTION('',(1.,0.,0.));
#23172=DIRECTION('center_axis',(0.,0.975288793285012,-0.22093385818535));
#23173=DIRECTION('ref_axis',(0.,0.22093385818535,0.975288793285012));
#23174=DIRECTION('',(1.,0.,0.));
#23175=DIRECTION('center_axis',(0.,0.98883598689863,-0.14900802332161));
#23176=DIRECTION('ref_axis',(0.,0.14900802332161,0.98883598689863));
#23177=DIRECTION('',(1.,0.,0.));
#23178=DIRECTION('center_axis',(0.,0.997086132304467,-0.0762839745039533));
#23179=DIRECTION('ref_axis',(0.,0.0762839745039533,0.997086132304467));
#23180=DIRECTION('',(1.,0.,0.));
#23181=DIRECTION('center_axis',(0.,0.999995034693158,-0.00315128371150461));
#23182=DIRECTION('ref_axis',(0.,0.00315128371150461,0.999995034693158));
#23183=DIRECTION('',(1.,0.,0.));
#23184=DIRECTION('center_axis',(0.,0.997547111504613,0.069998288041949));
#23185=DIRECTION('ref_axis',(0.,-0.069998288041949,0.997547111504613));
#23186=DIRECTION('',(1.,0.,0.));
#23187=DIRECTION('center_axis',(0.,0.98975547590149,0.142772889313813));
#23188=DIRECTION('ref_axis',(0.,-0.142772889313813,0.98975547590149));
#23189=DIRECTION('',(1.,0.,0.));
#23190=DIRECTION('center_axis',(0.,0.976661866523923,0.214782677322933));
#23191=DIRECTION('ref_axis',(0.,-0.214782677322933,0.976661866523923));
#23192=DIRECTION('',(1.,0.,0.));
#23193=DIRECTION('center_axis',(0.,0.958336423901792,0.285641906279744));
#23194=DIRECTION('ref_axis',(0.,-0.285641906279744,0.958336423901791));
#23195=DIRECTION('',(1.,0.,0.));
#23196=DIRECTION('center_axis',(0.,0.934877314722276,0.354970993769443));
#23197=DIRECTION('ref_axis',(0.,-0.354970993769443,0.934877314722276));
#23198=DIRECTION('',(1.,0.,0.));
#23199=DIRECTION('center_axis',(0.,0.906410205965427,0.422398554118871));
#23200=DIRECTION('ref_axis',(0.,-0.422398554118871,0.906410205965427));
#23201=DIRECTION('',(1.,0.,0.));
#23202=DIRECTION('center_axis',(0.,0.873087591724716,0.487563387854682));
#23203=DIRECTION('ref_axis',(0.,-0.487563387854682,0.873087591724716));
#23204=DIRECTION('',(1.,0.,0.));
#23205=DIRECTION('center_axis',(0.,0.835087976318743,0.550116416595493));
#23206=DIRECTION('ref_axis',(0.,-0.550116416595493,0.835087976318743));
#23207=DIRECTION('',(1.,0.,0.));
#23208=DIRECTION('center_axis',(0.,0.792614918069967,0.609722553013204));
#23209=DIRECTION('ref_axis',(0.,-0.609722553013204,0.792614918069967));
#23210=DIRECTION('',(1.,0.,0.));
#23211=DIRECTION('center_axis',(0.,0.745895938872873,0.666062495846264));
#23212=DIRECTION('ref_axis',(0.,-0.666062495846264,0.745895938872873));
#23213=DIRECTION('',(1.,0.,0.));
#23214=DIRECTION('center_axis',(0.,0.695181305392823,0.718834440349327));
#23215=DIRECTION('ref_axis',(0.,-0.718834440349327,0.695181305392823));
#23216=DIRECTION('',(1.,0.,0.));
#23217=DIRECTION('center_axis',(0.,0.640742688424503,0.767755695016677));
#23218=DIRECTION('ref_axis',(0.,-0.767755695016677,0.640742688424503));
#23219=DIRECTION('',(1.,0.,0.));
#23220=DIRECTION('center_axis',(0.,0.582871707591668,0.812564195918804));
#23221=DIRECTION('ref_axis',(0.,-0.812564195918804,0.582871707591668));
#23222=DIRECTION('',(1.,0.,0.));
#23223=DIRECTION('center_axis',(0.,0.521878369183895,0.853019910540169));
#23224=DIRECTION('ref_axis',(0.,-0.853019910540169,0.521878369183895));
#23225=DIRECTION('',(1.,0.,0.));
#23226=DIRECTION('center_axis',(0.,0.458089405498731,0.888906123597886));
#23227=DIRECTION('ref_axis',(0.,-0.888906123597886,0.458089405498731));
#23228=DIRECTION('',(1.,0.,0.));
#23229=DIRECTION('center_axis',(0.,0.39184652458508,0.920030597953456));
#23230=DIRECTION('ref_axis',(0.,-0.920030597953456,0.39184652458508));
#23231=DIRECTION('',(1.,0.,0.));
#23232=DIRECTION('center_axis',(0.,0.323504579763685,0.946226604398715));
#23233=DIRECTION('ref_axis',(0.,-0.946226604398715,0.323504579763685));
#23234=DIRECTION('',(1.,0.,0.));
#23235=DIRECTION('center_axis',(0.,0.253429668730349,0.967353814799542));
#23236=DIRECTION('ref_axis',(0.,-0.967353814799542,0.253429668730349));
#23237=DIRECTION('',(1.,0.,0.));
#23238=DIRECTION('center_axis',(0.,0.181997172424701,0.983299053812935));
#23239=DIRECTION('ref_axis',(0.,-0.983299053812935,0.181997172424701));
#23240=DIRECTION('',(1.,0.,0.));
#23241=DIRECTION('center_axis',(0.,0.109589744169988,0.993976905150596));
#23242=DIRECTION('ref_axis',(0.,-0.993976905150596,0.109589744169988));
#23243=DIRECTION('',(1.,0.,0.));
#23244=DIRECTION('center_axis',(0.,0.0365952598557893,0.999330169141354));
#23245=DIRECTION('ref_axis',(0.,-0.999330169141354,0.0365952598557893));
#23246=DIRECTION('',(1.,0.,0.));
#23247=DIRECTION('center_axis',(0.,-0.0365952598557893,0.999330169141354));
#23248=DIRECTION('ref_axis',(0.,-0.999330169141354,-0.0365952598557893));
#23249=DIRECTION('',(1.,0.,0.));
#23250=DIRECTION('center_axis',(0.,-0.109589744169987,0.993976905150596));
#23251=DIRECTION('ref_axis',(0.,-0.993976905150596,-0.109589744169987));
#23252=DIRECTION('',(1.,0.,0.));
#23253=DIRECTION('center_axis',(0.,-0.181997172424701,0.983299053812935));
#23254=DIRECTION('ref_axis',(0.,-0.983299053812935,-0.181997172424701));
#23255=DIRECTION('',(1.,0.,0.));
#23256=DIRECTION('center_axis',(0.,-0.253429668730349,0.967353814799542));
#23257=DIRECTION('ref_axis',(0.,-0.967353814799542,-0.253429668730349));
#23258=DIRECTION('',(1.,0.,0.));
#23259=DIRECTION('center_axis',(0.,-0.323504579763685,0.946226604398715));
#23260=DIRECTION('ref_axis',(0.,-0.946226604398715,-0.323504579763685));
#23261=DIRECTION('',(1.,0.,0.));
#23262=DIRECTION('center_axis',(0.,-0.39184652458508,0.920030597953456));
#23263=DIRECTION('ref_axis',(0.,-0.920030597953456,-0.39184652458508));
#23264=DIRECTION('',(1.,0.,0.));
#23265=DIRECTION('center_axis',(0.,-0.458089405498731,0.888906123597886));
#23266=DIRECTION('ref_axis',(0.,-0.888906123597886,-0.458089405498731));
#23267=DIRECTION('',(1.,0.,0.));
#23268=DIRECTION('center_axis',(0.,-0.521878369183893,0.85301991054017));
#23269=DIRECTION('ref_axis',(0.,-0.85301991054017,-0.521878369183893));
#23270=DIRECTION('',(1.,0.,0.));
#23271=DIRECTION('center_axis',(0.,-0.582871707591668,0.812564195918805));
#23272=DIRECTION('ref_axis',(0.,-0.812564195918805,-0.582871707591668));
#23273=DIRECTION('',(1.,0.,0.));
#23274=DIRECTION('center_axis',(0.,-0.640742688424505,0.767755695016675));
#23275=DIRECTION('ref_axis',(0.,-0.767755695016675,-0.640742688424505));
#23276=DIRECTION('',(1.,0.,0.));
#23277=DIRECTION('center_axis',(0.,-0.69518130539282,0.71883444034933));
#23278=DIRECTION('ref_axis',(0.,-0.71883444034933,-0.69518130539282));
#23279=DIRECTION('',(1.,0.,0.));
#23280=DIRECTION('center_axis',(0.,-0.745895938872875,0.666062495846262));
#23281=DIRECTION('ref_axis',(0.,-0.666062495846262,-0.745895938872875));
#23282=DIRECTION('',(1.,0.,0.));
#23283=DIRECTION('center_axis',(0.,-0.792614918069966,0.609722553013205));
#23284=DIRECTION('ref_axis',(0.,-0.609722553013205,-0.792614918069966));
#23285=DIRECTION('',(1.,0.,0.));
#23286=DIRECTION('center_axis',(0.,-0.835087976318742,0.550116416595494));
#23287=DIRECTION('ref_axis',(0.,-0.550116416595494,-0.835087976318742));
#23288=DIRECTION('',(1.,0.,0.));
#23289=DIRECTION('center_axis',(0.,-0.873087591724717,0.487563387854681));
#23290=DIRECTION('ref_axis',(0.,-0.487563387854681,-0.873087591724717));
#23291=DIRECTION('',(1.,0.,0.));
#23292=DIRECTION('center_axis',(0.,-0.906410205965425,0.422398554118875));
#23293=DIRECTION('ref_axis',(0.,-0.422398554118875,-0.906410205965425));
#23294=DIRECTION('',(1.,0.,0.));
#23295=DIRECTION('center_axis',(0.,-0.934877314722277,0.354970993769442));
#23296=DIRECTION('ref_axis',(0.,-0.354970993769442,-0.934877314722277));
#23297=DIRECTION('',(1.,0.,0.));
#23298=DIRECTION('center_axis',(0.,-0.958336423901792,0.285641906279744));
#23299=DIRECTION('ref_axis',(0.,-0.285641906279744,-0.958336423901791));
#23300=DIRECTION('',(1.,0.,0.));
#23301=DIRECTION('center_axis',(0.,-0.976661866523923,0.214782677322933));
#23302=DIRECTION('ref_axis',(0.,-0.214782677322933,-0.976661866523923));
#23303=DIRECTION('',(1.,0.,0.));
#23304=DIRECTION('center_axis',(0.,-0.98975547590149,0.142772889313813));
#23305=DIRECTION('ref_axis',(0.,-0.142772889313813,-0.98975547590149));
#23306=DIRECTION('',(1.,0.,0.));
#23307=DIRECTION('center_axis',(0.,-0.997547111504613,0.0699982880419509));
#23308=DIRECTION('ref_axis',(0.,-0.0699982880419509,-0.997547111504613));
#23309=DIRECTION('',(1.,0.,0.));
#23310=DIRECTION('center_axis',(0.,-0.999995034693158,-0.00315128371150461));
#23311=DIRECTION('ref_axis',(0.,0.00315128371150461,-0.999995034693158));
#23312=DIRECTION('',(1.,0.,0.));
#23313=DIRECTION('center_axis',(0.,-0.997086132304467,-0.0762839745039523));
#23314=DIRECTION('ref_axis',(0.,0.0762839745039523,-0.997086132304467));
#23315=DIRECTION('',(1.,0.,0.));
#23316=DIRECTION('center_axis',(0.,-0.98883598689863,-0.14900802332161));
#23317=DIRECTION('ref_axis',(0.,0.14900802332161,-0.98883598689863));
#23318=DIRECTION('',(1.,0.,0.));
#23319=DIRECTION('center_axis',(0.,-0.975288793285013,-0.220933858185349));
#23320=DIRECTION('ref_axis',(0.,0.220933858185349,-0.975288793285013));
#23321=DIRECTION('',(1.,0.,0.));
#23322=DIRECTION('center_axis',(0.,-0.956517121777199,-0.291676183030194));
#23323=DIRECTION('ref_axis',(0.,0.291676183030194,-0.956517121777199));
#23324=DIRECTION('',(1.,0.,0.));
#23325=DIRECTION('center_axis',(0.,-0.932621529444546,-0.360856041679387));
#23326=DIRECTION('ref_axis',(0.,0.360856041679387,-0.932621529444546));
#23327=DIRECTION('',(1.,0.,0.));
#23328=DIRECTION('center_axis',(0.,-0.90373002144283,-0.428102847856613));
#23329=DIRECTION('ref_axis',(0.,0.428102847856613,-0.90373002144283));
#23330=DIRECTION('',(1.,0.,0.));
#23331=DIRECTION('center_axis',(0.,-0.869997365309547,-0.493056370361895));
#23332=DIRECTION('ref_axis',(0.,0.493056370361895,-0.869997365309547));
#23333=DIRECTION('',(1.,0.,0.));
#23334=DIRECTION('center_axis',(0.,-0.831604261897095,-0.555368662776888));
#23335=DIRECTION('ref_axis',(0.,0.555368662776888,-0.831604261897095));
#23336=DIRECTION('',(1.,0.,0.));
#23337=DIRECTION('center_axis',(0.,-0.788756377385019,-0.614705927362394));
#23338=DIRECTION('ref_axis',(0.,0.614705927362394,-0.788756377385019));
#23339=DIRECTION('',(1.,0.,0.));
#23340=DIRECTION('center_axis',(0.,-0.741683241556689,-0.670750303163526));
#23341=DIRECTION('ref_axis',(0.,0.670750303163526,-0.741683241556689));
#23342=DIRECTION('',(1.,0.,0.));
#23343=DIRECTION('center_axis',(0.,-0.690637018242184,-0.723201568743836));
#23344=DIRECTION('ref_axis',(0.,0.723201568743836,-0.690637018242184));
#23345=DIRECTION('',(1.,0.,0.));
#23346=DIRECTION('center_axis',(0.,-0.635891154513924,-0.771778750427186));
#23347=DIRECTION('ref_axis',(0.,0.771778750427186,-0.635891154513924));
#23348=DIRECTION('',(1.,0.,0.));
#23349=DIRECTION('center_axis',(0.,-0.577738915871126,-0.816221627432192));
#23350=DIRECTION('ref_axis',(0.,0.816221627432192,-0.577738915871126));
#23351=DIRECTION('',(1.,0.,0.));
#23352=DIRECTION('center_axis',(0.,-0.516491815259888,-0.856292125836473));
#23353=DIRECTION('ref_axis',(0.,0.856292125836472,-0.516491815259888));
#23354=DIRECTION('',(1.,0.,0.));
#23355=DIRECTION('center_axis',(0.,0.874619707139396,-0.484809620246337));
#23356=DIRECTION('ref_axis',(0.,0.484809620246337,0.874619707139396));
#23357=DIRECTION('',(1.,0.,0.));
#23358=DIRECTION('center_axis',(0.,-0.382683432365091,-0.923879532511286));
#23359=DIRECTION('ref_axis',(0.,0.923879532511286,-0.382683432365091));
#23360=DIRECTION('',(1.,0.,0.));
#23361=DIRECTION('center_axis',(0.,-0.961261695938319,0.275637355817));
#23362=DIRECTION('ref_axis',(0.,-0.275637355817,-0.961261695938319));
#23363=DIRECTION('',(1.,0.,0.));
#23364=DIRECTION('center_axis',(0.,0.313624196791349,0.94954718849933));
#23365=DIRECTION('ref_axis',(0.,-0.94954718849933,0.313624196791349));
#23366=DIRECTION('',(1.,0.,0.));
#23367=DIRECTION('center_axis',(0.,0.388051839083456,0.921637548163023));
#23368=DIRECTION('ref_axis',(0.,-0.921637548163022,0.388051839083456));
#23369=DIRECTION('',(1.,0.,0.));
#23370=DIRECTION('center_axis',(0.,0.460027606113537,0.88790461290245));
#23371=DIRECTION('ref_axis',(0.,-0.887904612902449,0.460027606113537));
#23372=DIRECTION('',(1.,0.,0.));
#23373=DIRECTION('center_axis',(0.,0.529096724614553,0.848561521636558));
#23374=DIRECTION('ref_axis',(0.,-0.848561521636558,0.529096724614553));
#23375=DIRECTION('',(1.,0.,0.));
#23376=DIRECTION('center_axis',(0.,0.594822786751342,0.803856860617217));
#23377=DIRECTION('ref_axis',(0.,-0.803856860617217,0.594822786751342));
#23378=DIRECTION('',(1.,0.,0.));
#23379=DIRECTION('center_axis',(0.,0.656790507529498,0.754073092756362));
#23380=DIRECTION('ref_axis',(0.,-0.754073092756362,0.656790507529498));
#23381=DIRECTION('',(1.,0.,0.));
#23382=DIRECTION('center_axis',(0.,0.714608348741196,0.699524772906136));
#23383=DIRECTION('ref_axis',(0.,-0.699524772906136,0.714608348741196));
#23384=DIRECTION('',(1.,0.,0.));
#23385=DIRECTION('center_axis',(0.,0.767910992868789,0.640556560368615));
#23386=DIRECTION('ref_axis',(0.,-0.640556560368615,0.767910992868789));
#23387=DIRECTION('',(1.,0.,0.));
#23388=DIRECTION('center_axis',(0.,0.816361651315052,0.577541041192885));
#23389=DIRECTION('ref_axis',(0.,-0.577541041192885,0.816361651315052));
#23390=DIRECTION('',(1.,0.,0.));
#23391=DIRECTION('center_axis',(0.,0.85965419237564,0.51087637401918));
#23392=DIRECTION('ref_axis',(0.,-0.51087637401918,0.85965419237564));
#23393=DIRECTION('',(1.,0.,0.));
#23394=DIRECTION('center_axis',(0.,0.897515075508373,0.44098377434459));
#23395=DIRECTION('ref_axis',(0.,-0.44098377434459,0.897515075508373));
#23396=DIRECTION('',(1.,0.,0.));
#23397=DIRECTION('center_axis',(0.,0.929705079677808,0.368304853105793));
#23398=DIRECTION('ref_axis',(0.,-0.368304853105793,0.929705079677808));
#23399=DIRECTION('',(1.,0.,0.));
#23400=DIRECTION('center_axis',(0.,0.95602081485468,0.293298826394844));
#23401=DIRECTION('ref_axis',(0.,-0.293298826394844,0.95602081485468));
#23402=DIRECTION('',(1.,0.,0.));
#23403=DIRECTION('center_axis',(0.,0.976296007119934,0.2164396139381));
#23404=DIRECTION('ref_axis',(0.,-0.2164396139381,0.976296007119934));
#23405=DIRECTION('',(1.,0.,0.));
#23406=DIRECTION('center_axis',(0.,0.990402549253496,0.138212844671456));
#23407=DIRECTION('ref_axis',(0.,-0.138212844671456,0.990402549253496));
#23408=DIRECTION('',(1.,0.,0.));
#23409=DIRECTION('center_axis',(0.,0.998251310169761,0.0591127883317614));
#23410=DIRECTION('ref_axis',(0.,-0.0591127883317614,0.998251310169761));
#23411=DIRECTION('',(1.,0.,0.));
#23412=DIRECTION('center_axis',(0.,0.999792698085388,-0.0203607675478923));
#23413=DIRECTION('ref_axis',(0.,0.0203607675478923,0.999792698085389));
#23414=DIRECTION('',(1.,0.,0.));
#23415=DIRECTION('center_axis',(0.,0.995016973861122,-0.0997056755067372));
#23416=DIRECTION('ref_axis',(0.,0.0997056755067372,0.995016973861122));
#23417=DIRECTION('',(1.,0.,0.));
#23418=DIRECTION('center_axis',(0.,0.983954312537781,-0.178420600935832));
#23419=DIRECTION('ref_axis',(0.,0.178420600935832,0.983954312537781));
#23420=DIRECTION('',(1.,0.,0.));
#23421=DIRECTION('center_axis',(0.,0.966674612677614,-0.256008189721705));
#23422=DIRECTION('ref_axis',(0.,0.256008189721705,0.966674612677614));
#23423=DIRECTION('',(1.,0.,0.));
#23424=DIRECTION('center_axis',(0.,0.943287054715696,-0.331978210739482));
#23425=DIRECTION('ref_axis',(0.,0.331978210739482,0.943287054715696));
#23426=DIRECTION('',(1.,0.,0.));
#23427=DIRECTION('center_axis',(0.,0.913939411111865,-0.405850653339991));
#23428=DIRECTION('ref_axis',(0.,0.405850653339991,0.913939411111865));
#23429=DIRECTION('',(1.,0.,0.));
#23430=DIRECTION('center_axis',(0.,0.878817112661964,-0.47715876025961));
#23431=DIRECTION('ref_axis',(0.,0.47715876025961,0.878817112661964));
#23432=DIRECTION('',(1.,0.,0.));
#23433=DIRECTION('center_axis',(0.,0.83814207686784,-0.545451976789583));
#23434=DIRECTION('ref_axis',(0.,0.545451976789583,0.83814207686784));
#23435=DIRECTION('',(1.,0.,0.));
#23436=DIRECTION('center_axis',(0.,0.792171305768909,-0.610298797570814));
#23437=DIRECTION('ref_axis',(0.,0.610298797570814,0.792171305768909));
#23438=DIRECTION('',(1.,0.,0.));
#23439=DIRECTION('center_axis',(0.,0.741195262094844,-0.671289493026783));
#23440=DIRECTION('ref_axis',(0.,0.671289493026783,0.741195262094844));
#23441=DIRECTION('',(1.,0.,0.));
#23442=DIRECTION('center_axis',(0.,0.685536033999469,-0.728038698207918));
#23443=DIRECTION('ref_axis',(0.,0.728038698207918,0.685536033999469));
#23444=DIRECTION('',(1.,0.,0.));
#23445=DIRECTION('center_axis',(0.,0.62554529997191,-0.780187847689935));
#23446=DIRECTION('ref_axis',(0.,0.780187847689935,0.62554529997191));
#23447=DIRECTION('',(1.,0.,0.));
#23448=DIRECTION('center_axis',(0.,0.561602106783492,-0.827407441141511));
#23449=DIRECTION('ref_axis',(0.,0.827407441141511,0.561602106783492));
#23450=DIRECTION('',(1.,0.,0.));
#23451=DIRECTION('center_axis',(0.,0.494110474510307,-0.869399125246396));
#23452=DIRECTION('ref_axis',(0.,0.869399125246396,0.494110474510307));
#23453=DIRECTION('',(1.,0.,0.));
#23454=DIRECTION('center_axis',(0.,0.423496843763887,-0.905897578825568));
#23455=DIRECTION('ref_axis',(0.,0.905897578825568,0.423496843763887));
#23456=DIRECTION('',(1.,0.,0.));
#23457=DIRECTION('center_axis',(0.,0.350207381259467,-0.936672189248398));
#23458=DIRECTION('ref_axis',(0.,0.936672189248398,0.350207381259467));
#23459=DIRECTION('',(1.,0.,0.));
#23460=DIRECTION('center_axis',(0.,0.274705160746442,-0.96152850954055));
#23461=DIRECTION('ref_axis',(0.,0.96152850954055,0.274705160746442));
#23462=DIRECTION('',(1.,0.,0.));
#23463=DIRECTION('center_axis',(0.,0.197467237112997,-0.980309486982024));
#23464=DIRECTION('ref_axis',(0.,0.980309486982024,0.197467237112997));
#23465=DIRECTION('',(1.,0.,0.));
#23466=DIRECTION('center_axis',(0.,0.118981632152029,-0.992896455432509));
#23467=DIRECTION('ref_axis',(0.,0.992896455432508,0.118981632152029));
#23468=DIRECTION('',(1.,0.,0.));
#23469=DIRECTION('center_axis',(0.,0.0397442510335229,-0.999209885114126));
#23470=DIRECTION('ref_axis',(0.,0.999209885114126,0.0397442510335229));
#23471=DIRECTION('',(1.,0.,0.));
#23472=DIRECTION('center_axis',(0.,-0.0397442510335258,-0.999209885114126));
#23473=DIRECTION('ref_axis',(0.,0.999209885114126,-0.0397442510335258));
#23474=DIRECTION('',(1.,0.,0.));
#23475=DIRECTION('center_axis',(0.,-0.118981632152026,-0.992896455432509));
#23476=DIRECTION('ref_axis',(0.,0.992896455432509,-0.118981632152026));
#23477=DIRECTION('',(1.,0.,0.));
#23478=DIRECTION('center_axis',(0.,-0.197467237112996,-0.980309486982024));
#23479=DIRECTION('ref_axis',(0.,0.980309486982024,-0.197467237112996));
#23480=DIRECTION('',(1.,0.,0.));
#23481=DIRECTION('center_axis',(0.,-0.274705160746445,-0.961528509540549));
#23482=DIRECTION('ref_axis',(0.,0.961528509540549,-0.274705160746445));
#23483=DIRECTION('',(1.,0.,0.));
#23484=DIRECTION('center_axis',(0.,-0.350207381259469,-0.936672189248397));
#23485=DIRECTION('ref_axis',(0.,0.936672189248397,-0.350207381259469));
#23486=DIRECTION('',(1.,0.,0.));
#23487=DIRECTION('center_axis',(0.,-0.423496843763883,-0.90589757882557));
#23488=DIRECTION('ref_axis',(0.,0.905897578825569,-0.423496843763883));
#23489=DIRECTION('',(1.,0.,0.));
#23490=DIRECTION('center_axis',(0.,-0.494110474510309,-0.869399125246396));
#23491=DIRECTION('ref_axis',(0.,0.869399125246396,-0.494110474510309));
#23492=DIRECTION('',(1.,0.,0.));
#23493=DIRECTION('center_axis',(0.,-0.561602106783492,-0.827407441141511));
#23494=DIRECTION('ref_axis',(0.,0.827407441141511,-0.561602106783492));
#23495=DIRECTION('',(1.,0.,0.));
#23496=DIRECTION('center_axis',(0.,-0.62554529997191,-0.780187847689935));
#23497=DIRECTION('ref_axis',(0.,0.780187847689935,-0.62554529997191));
#23498=DIRECTION('',(1.,0.,0.));
#23499=DIRECTION('center_axis',(0.,-0.685536033999469,-0.728038698207917));
#23500=DIRECTION('ref_axis',(0.,0.728038698207917,-0.685536033999469));
#23501=DIRECTION('',(1.,0.,0.));
#23502=DIRECTION('center_axis',(0.,-0.741195262094845,-0.671289493026783));
#23503=DIRECTION('ref_axis',(0.,0.671289493026782,-0.741195262094845));
#23504=DIRECTION('',(1.,0.,0.));
#23505=DIRECTION('center_axis',(0.,-0.79217130576891,-0.610298797570813));
#23506=DIRECTION('ref_axis',(0.,0.610298797570813,-0.79217130576891));
#23507=DIRECTION('',(1.,0.,0.));
#23508=DIRECTION('center_axis',(0.,-0.838142076867841,-0.545451976789582));
#23509=DIRECTION('ref_axis',(0.,0.545451976789582,-0.83814207686784));
#23510=DIRECTION('',(1.,0.,0.));
#23511=DIRECTION('center_axis',(0.,-0.878817112661967,-0.477158760259606));
#23512=DIRECTION('ref_axis',(0.,0.477158760259606,-0.878817112661967));
#23513=DIRECTION('',(1.,0.,0.));
#23514=DIRECTION('center_axis',(0.,-0.913939411111864,-0.405850653339993));
#23515=DIRECTION('ref_axis',(0.,0.405850653339993,-0.913939411111864));
#23516=DIRECTION('',(1.,0.,0.));
#23517=DIRECTION('center_axis',(0.,-0.943287054715697,-0.33197821073948));
#23518=DIRECTION('ref_axis',(0.,0.33197821073948,-0.943287054715696));
#23519=DIRECTION('',(1.,0.,0.));
#23520=DIRECTION('center_axis',(0.,-0.966674612677614,-0.256008189721705));
#23521=DIRECTION('ref_axis',(0.,0.256008189721705,-0.966674612677614));
#23522=DIRECTION('',(1.,0.,0.));
#23523=DIRECTION('center_axis',(0.,-0.983954312537781,-0.178420600935832));
#23524=DIRECTION('ref_axis',(0.,0.178420600935832,-0.983954312537781));
#23525=DIRECTION('',(1.,0.,0.));
#23526=DIRECTION('center_axis',(0.,-0.995016973861122,-0.0997056755067357));
#23527=DIRECTION('ref_axis',(0.,0.0997056755067357,-0.995016973861122));
#23528=DIRECTION('',(1.,0.,0.));
#23529=DIRECTION('center_axis',(0.,-0.999792698085388,-0.0203607675478923));
#23530=DIRECTION('ref_axis',(0.,0.0203607675478923,-0.999792698085389));
#23531=DIRECTION('',(1.,0.,0.));
#23532=DIRECTION('center_axis',(0.,-0.998251310169761,0.0591127883317644));
#23533=DIRECTION('ref_axis',(0.,-0.0591127883317644,-0.998251310169761));
#23534=DIRECTION('',(1.,0.,0.));
#23535=DIRECTION('center_axis',(0.,-0.990402549253497,0.138212844671453));
#23536=DIRECTION('ref_axis',(0.,-0.138212844671453,-0.990402549253497));
#23537=DIRECTION('',(1.,0.,0.));
#23538=DIRECTION('center_axis',(0.,-0.976296007119933,0.216439613938106));
#23539=DIRECTION('ref_axis',(0.,-0.216439613938106,-0.976296007119933));
#23540=DIRECTION('',(1.,0.,0.));
#23541=DIRECTION('center_axis',(0.,-0.956020814854681,0.293298826394842));
#23542=DIRECTION('ref_axis',(0.,-0.293298826394842,-0.956020814854681));
#23543=DIRECTION('',(1.,0.,0.));
#23544=DIRECTION('center_axis',(0.,-0.929705079677808,0.368304853105795));
#23545=DIRECTION('ref_axis',(0.,-0.368304853105795,-0.929705079677808));
#23546=DIRECTION('',(1.,0.,0.));
#23547=DIRECTION('center_axis',(0.,-0.897515075508373,0.44098377434459));
#23548=DIRECTION('ref_axis',(0.,-0.44098377434459,-0.897515075508373));
#23549=DIRECTION('',(1.,0.,0.));
#23550=DIRECTION('center_axis',(0.,-0.85965419237564,0.510876374019181));
#23551=DIRECTION('ref_axis',(0.,-0.510876374019181,-0.85965419237564));
#23552=DIRECTION('',(1.,0.,0.));
#23553=DIRECTION('center_axis',(0.,-0.816361651315051,0.577541041192886));
#23554=DIRECTION('ref_axis',(0.,-0.577541041192886,-0.816361651315051));
#23555=DIRECTION('',(1.,0.,0.));
#23556=DIRECTION('center_axis',(0.,-0.767910992868789,0.640556560368615));
#23557=DIRECTION('ref_axis',(0.,-0.640556560368615,-0.767910992868789));
#23558=DIRECTION('',(1.,0.,0.));
#23559=DIRECTION('center_axis',(0.,-0.714608348741195,0.699524772906137));
#23560=DIRECTION('ref_axis',(0.,-0.699524772906137,-0.714608348741195));
#23561=DIRECTION('',(1.,0.,0.));
#23562=DIRECTION('center_axis',(0.,-0.656790507529498,0.754073092756361));
#23563=DIRECTION('ref_axis',(0.,-0.754073092756361,-0.656790507529498));
#23564=DIRECTION('',(1.,0.,0.));
#23565=DIRECTION('center_axis',(0.,-0.59482278675134,0.803856860617219));
#23566=DIRECTION('ref_axis',(0.,-0.803856860617218,-0.59482278675134));
#23567=DIRECTION('',(1.,0.,0.));
#23568=DIRECTION('center_axis',(0.,-0.529096724614554,0.848561521636558));
#23569=DIRECTION('ref_axis',(0.,-0.848561521636558,-0.529096724614554));
#23570=DIRECTION('',(1.,0.,0.));
#23571=DIRECTION('center_axis',(0.,-0.460027606113536,0.88790461290245));
#23572=DIRECTION('ref_axis',(0.,-0.88790461290245,-0.460027606113536));
#23573=DIRECTION('',(1.,0.,0.));
#23574=DIRECTION('center_axis',(0.,-0.388051839083455,0.921637548163023));
#23575=DIRECTION('ref_axis',(0.,-0.921637548163023,-0.388051839083454));
#23576=DIRECTION('',(1.,0.,0.));
#23577=DIRECTION('center_axis',(0.,-0.313624196791348,0.94954718849933));
#23578=DIRECTION('ref_axis',(0.,-0.94954718849933,-0.313624196791348));
#23579=DIRECTION('',(1.,0.,0.));
#23580=DIRECTION('center_axis',(0.,0.961261695938319,0.275637355816999));
#23581=DIRECTION('ref_axis',(0.,-0.275637355816999,0.961261695938319));
#23582=DIRECTION('',(0.,0.,1.));
#23583=DIRECTION('',(1.,0.,0.));
#23584=DIRECTION('',(0.,0.,1.));
#23585=DIRECTION('',(1.,0.,0.));
#23586=DIRECTION('',(0.,0.,1.));
#23587=DIRECTION('',(1.,0.,0.));
#23588=DIRECTION('',(0.,0.,1.));
#23589=DIRECTION('',(1.,0.,0.));
#23590=DIRECTION('',(0.,0.,1.));
#23591=DIRECTION('',(1.,0.,0.));
#23592=DIRECTION('',(0.,0.,1.));
#23593=DIRECTION('',(1.,0.,0.));
#23594=DIRECTION('',(0.,0.,1.));
#23595=DIRECTION('',(1.,0.,0.));
#23596=DIRECTION('',(0.,0.,1.));
#23597=DIRECTION('',(1.,0.,0.));
#23598=DIRECTION('',(0.,0.,1.));
#23599=DIRECTION('',(1.,0.,0.));
#23600=DIRECTION('',(0.,0.,1.));
#23601=DIRECTION('',(1.,0.,0.));
#23602=DIRECTION('',(0.,0.,1.));
#23603=DIRECTION('',(1.,0.,0.));
#23604=DIRECTION('',(0.,0.,1.));
#23605=DIRECTION('',(1.,0.,0.));
#23606=DIRECTION('',(0.,0.,1.));
#23607=DIRECTION('',(1.,0.,0.));
#23608=DIRECTION('',(0.,0.,1.));
#23609=DIRECTION('',(1.,0.,0.));
#23610=CARTESIAN_POINT('',(0.,0.,0.));
#23611=CARTESIAN_POINT('',(0.,0.,0.));
#23612=CARTESIAN_POINT('Origin',(165.,0.,0.));
#23613=CARTESIAN_POINT('',(157.293320454657,-3.44544707048975,0.00244461032172155));
#23614=CARTESIAN_POINT('',(157.148679545343,-3.4447563047016,0.00308232498356144));
#23615=CARTESIAN_POINT('',(165.,-3.442,-4.21523428266519E-16));
#23616=CARTESIAN_POINT('',(156.971,1.51264420613078,3.09472314487926));
#23617=CARTESIAN_POINT('Ctrl Pts',(157.293320454657,-3.44544707048975,0.00244461032172155));
#23618=CARTESIAN_POINT('Ctrl Pts',(157.286646439823,-3.44655406665934,0.146366209264783));
#23619=CARTESIAN_POINT('Ctrl Pts',(157.279972424989,-3.43831085885886,0.290155103803701));
#23620=CARTESIAN_POINT('Ctrl Pts',(157.273298410156,-3.42028738572634,0.432700406627246));
#23621=CARTESIAN_POINT('Ctrl Pts',(157.22068273819,-3.27819642943416,1.5564792834418));
#23622=CARTESIAN_POINT('Ctrl Pts',(157.168067066223,-2.52824130408745,2.6029663057877));
#23623=CARTESIAN_POINT('Ctrl Pts',(157.115451394257,-1.50964233980923,3.09927108189291));
#23624=CARTESIAN_POINT('Ctrl Pts',(157.067300929505,-0.577486354841783,
3.55345715868931));
#23625=CARTESIAN_POINT('Ctrl Pts',(157.019150464752,0.579651545136316,3.5468805548435));
#23626=CARTESIAN_POINT('Ctrl Pts',(156.971,1.5145057733605,3.09672906731558));
#23627=CARTESIAN_POINT('',(156.971,-1.51078263890264,3.09271722244216));
#23628=CARTESIAN_POINT('Origin',(156.971,0.,0.));
#23629=CARTESIAN_POINT('Ctrl Pts',(156.971,-1.51078263890258,3.0927172224422));
#23630=CARTESIAN_POINT('Ctrl Pts',(157.023615671966,-2.53321644899237,2.59326152099565));
#23631=CARTESIAN_POINT('Ctrl Pts',(157.076231343932,-3.27990605922292,1.5510599284818));
#23632=CARTESIAN_POINT('Ctrl Pts',(157.128847015898,-3.42018516348441,0.428800544168781));
#23633=CARTESIAN_POINT('Ctrl Pts',(157.135457859047,-3.43781039035294,0.287795393344797));
#23634=CARTESIAN_POINT('Ctrl Pts',(157.142068702195,-3.44586257045956,0.145526417146741));
#23635=CARTESIAN_POINT('Ctrl Pts',(157.148679545343,-3.4447563047016,0.00308232498356144));
#23636=CARTESIAN_POINT('Origin',(165.,0.,0.));
#23637=CARTESIAN_POINT('',(158.293320454657,-3.43670969417942,0.000689374022927458));
#23638=CARTESIAN_POINT('',(158.148679545343,-3.43671104026434,0.000722531392082319));
#23639=CARTESIAN_POINT('',(165.,-3.442,-4.21523428266519E-16));
#23640=CARTESIAN_POINT('Ctrl Pts',(158.293320454657,-3.43670969417942,0.000689374022927458));
#23641=CARTESIAN_POINT('Ctrl Pts',(158.269007138287,-3.43766262966877,0.528446666858329));
#23642=CARTESIAN_POINT('Ctrl Pts',(158.244693821917,-3.32341965147669,1.05581244132256));
#23643=CARTESIAN_POINT('Ctrl Pts',(158.220380505546,-3.09181810624384,1.52528055684926));
#23644=CARTESIAN_POINT('Ctrl Pts',(158.16776483358,-2.59061659406446,2.54124152198624));
#23645=CARTESIAN_POINT('Ctrl Pts',(158.115149161614,-1.53980253555905,3.28605671091484));
#23646=CARTESIAN_POINT('Ctrl Pts',(158.062533489648,-0.415180135400307,
3.42248722507319));
#23647=CARTESIAN_POINT('Ctrl Pts',(158.009917817682,0.709442264758436,3.55891773923153));
#23648=CARTESIAN_POINT('Ctrl Pts',(157.957302145716,1.90787300657052,3.08696357861963));
#23649=CARTESIAN_POINT('Ctrl Pts',(157.904686473749,2.63745093069739,2.22029759264997));
#23650=CARTESIAN_POINT('Ctrl Pts',(157.852070801783,3.36702885482427,1.35363160668031));
#23651=CARTESIAN_POINT('Ctrl Pts',(157.799455129817,3.62775396126593,0.0922537953528965));
#23652=CARTESIAN_POINT('Ctrl Pts',(157.746839457851,3.30159132076051,-0.992625515603271));
#23653=CARTESIAN_POINT('Ctrl Pts',(157.694223785885,2.97542868025509,-2.07750482655944));
#23654=CARTESIAN_POINT('Ctrl Pts',(157.641608113919,2.06237829280258,-2.98588563714436));
#23655=CARTESIAN_POINT('Ctrl Pts',(157.588992441953,0.975826462102337,-3.3065682899409));
#23656=CARTESIAN_POINT('Ctrl Pts',(157.536376769987,-0.110725368597905,
-3.62725094273743));
#23657=CARTESIAN_POINT('Ctrl Pts',(157.48376109802,-1.37077864254588,-3.36023543774558));
#23658=CARTESIAN_POINT('Ctrl Pts',(157.431145426054,-2.23369188590104,-2.62619231960805));
#23659=CARTESIAN_POINT('Ctrl Pts',(157.385203768922,-2.98714922816898,-1.98525862069813));
#23660=CARTESIAN_POINT('Ctrl Pts',(157.339262111789,-3.43782688387983,-0.988262919902665));
#23661=CARTESIAN_POINT('Ctrl Pts',(157.293320454657,-3.44544707048975,0.00244461032172155));
#23662=CARTESIAN_POINT('Ctrl Pts',(157.148679545343,-3.4447563047016,0.00308232498356144));
#23663=CARTESIAN_POINT('Ctrl Pts',(157.194684374161,-3.43705780608635,-0.988185495048805));
#23664=CARTESIAN_POINT('Ctrl Pts',(157.240689202979,-2.98583756510872,-1.98793376461549));
#23665=CARTESIAN_POINT('Ctrl Pts',(157.286694031797,-2.23081923614179,-2.62925913604816));
#23666=CARTESIAN_POINT('Ctrl Pts',(157.339309703763,-1.36730560624524,-3.36274225583985));
#23667=CARTESIAN_POINT('Ctrl Pts',(157.391925375729,-0.106409748159716,
-3.62739131931104));
#23668=CARTESIAN_POINT('Ctrl Pts',(157.444541047695,0.97989223421638,-3.30519505703097));
#23669=CARTESIAN_POINT('Ctrl Pts',(157.497156719662,2.06619421659248,-2.98299879475091));
#23670=CARTESIAN_POINT('Ctrl Pts',(157.549772391628,2.97790232325914,-2.07395720671959));
#23671=CARTESIAN_POINT('Ctrl Pts',(157.602388063594,3.3027072388958,-0.988797871088526));
#23672=CARTESIAN_POINT('Ctrl Pts',(157.65500373556,3.62751215453247,0.0963614645425373));
#23673=CARTESIAN_POINT('Ctrl Pts',(157.707619407526,3.36541387913912,1.35763854777334));
#23674=CARTESIAN_POINT('Ctrl Pts',(157.760235079492,2.63483694617998,2.22348839844289));
#23675=CARTESIAN_POINT('Ctrl Pts',(157.812850751458,1.90426001322083,3.08933824911244));
#23676=CARTESIAN_POINT('Ctrl Pts',(157.865466423424,0.705204422695883,3.55976086722073));
#23677=CARTESIAN_POINT('Ctrl Pts',(157.918082095391,-0.419270853672587,
3.42196497454828));
#23678=CARTESIAN_POINT('Ctrl Pts',(157.970697767357,-1.54374613004106,3.28416908187583));
#23679=CARTESIAN_POINT('Ctrl Pts',(158.023313439323,-2.59364109225305,2.53815467842265));
#23680=CARTESIAN_POINT('Ctrl Pts',(158.075929111289,-3.0936245505079,1.52161060115695));
#23681=CARTESIAN_POINT('Ctrl Pts',(158.100179255974,-3.32406294936394,1.0530935219133));
#23682=CARTESIAN_POINT('Ctrl Pts',(158.124429400658,-3.43768833393163,0.527110129590025));
#23683=CARTESIAN_POINT('Ctrl Pts',(158.148679545343,-3.43671104026434,0.000722531392082319));
#23684=CARTESIAN_POINT('Origin',(165.,0.,0.));
#23685=CARTESIAN_POINT('',(159.293320454657,-3.44310231280533,-0.00296426346809486));
#23686=CARTESIAN_POINT('',(159.148679545343,-3.44306193045544,-0.00296971903132968));
#23687=CARTESIAN_POINT('',(165.,-3.442,-4.21523428266519E-16));
#23688=CARTESIAN_POINT('Ctrl Pts',(159.293320454657,-3.44310231280533,-0.00296426346809486));
#23689=CARTESIAN_POINT('Ctrl Pts',(159.25136783675,-3.43491299719851,0.903398659033635));
#23690=CARTESIAN_POINT('Ctrl Pts',(159.209415218844,-3.06678173055999,1.81564946014422));
#23691=CARTESIAN_POINT('Ctrl Pts',(159.167462600937,-2.42463302112472,2.45091276876142));
#23692=CARTESIAN_POINT('Ctrl Pts',(159.114846928971,-1.61927002984871,3.24764030392345));
#23693=CARTESIAN_POINT('Ctrl Pts',(159.062231257005,-0.382894089265012,
3.6086831803192));
#23694=CARTESIAN_POINT('Ctrl Pts',(159.009615585039,0.724662800527638,3.37056108274876));
#23695=CARTESIAN_POINT('Ctrl Pts',(158.956999913072,1.83221969032029,3.13243898517832));
#23696=CARTESIAN_POINT('Ctrl Pts',(158.904384241106,2.81095752932189,2.2951519136417));
#23697=CARTESIAN_POINT('Ctrl Pts',(158.85176856914,3.21770283408525,1.23782374941761));
#23698=CARTESIAN_POINT('Ctrl Pts',(158.799152897174,3.62444813884861,0.180495585193521));
#23699=CARTESIAN_POINT('Ctrl Pts',(158.746537225208,3.45920090937374,-1.09687367171803));
#23700=CARTESIAN_POINT('Ctrl Pts',(158.693921553242,2.79678554937194,-2.0158892920362));
#23701=CARTESIAN_POINT('Ctrl Pts',(158.641305881276,2.13437018937015,-2.93490491235436));
#23702=CARTESIAN_POINT('Ctrl Pts',(158.588690209309,0.974786698841445,-3.49556689607912));
#23703=CARTESIAN_POINT('Ctrl Pts',(158.536074537343,-0.156905172830018,
-3.44400872313727));
#23704=CARTESIAN_POINT('Ctrl Pts',(158.483458865377,-1.28859704450148,-3.39245055019542));
#23705=CARTESIAN_POINT('Ctrl Pts',(158.430843193411,-2.3923972973157,-2.72867222058695));
#23706=CARTESIAN_POINT('Ctrl Pts',(158.378227521445,-2.96850294079614,-1.75322968511002));
#23707=CARTESIAN_POINT('Ctrl Pts',(158.349925165849,-3.27839438897766,-1.2285319957928));
#23708=CARTESIAN_POINT('Ctrl Pts',(158.321622810253,-3.43560041239042,-0.613656046518903));
#23709=CARTESIAN_POINT('Ctrl Pts',(158.293320454657,-3.43670969417942,0.000689374022927458));
#23710=CARTESIAN_POINT('Ctrl Pts',(158.148679545343,-3.43671104026434,0.000722531392082319));
#23711=CARTESIAN_POINT('Ctrl Pts',(158.177045072625,-3.43556789449997,-0.614995930146503));
#23712=CARTESIAN_POINT('Ctrl Pts',(158.205410599906,-3.27762411237375,-1.23126743057864));
#23713=CARTESIAN_POINT('Ctrl Pts',(158.233776127187,-2.96641712416019,-1.75676955526741));
#23714=CARTESIAN_POINT('Ctrl Pts',(158.286391799154,-2.38915428525994,-2.73153188334787));
#23715=CARTESIAN_POINT('Ctrl Pts',(158.33900747112,-1.28455665316172,-3.39398278843057));
#23716=CARTESIAN_POINT('Ctrl Pts',(158.391623143086,-0.152802192417,-3.44419016734183));
#23717=CARTESIAN_POINT('Ctrl Pts',(158.444238815052,0.97895226832773,-3.49439754625309));
#23718=CARTESIAN_POINT('Ctrl Pts',(158.496854487018,2.13786355771897,-2.9323613989929));
#23719=CARTESIAN_POINT('Ctrl Pts',(158.549470158984,2.79918318783638,-2.01255919133261));
#23720=CARTESIAN_POINT('Ctrl Pts',(158.602085830951,3.46050281795378,-1.09275698367232));
#23721=CARTESIAN_POINT('Ctrl Pts',(158.654701502917,3.62423078879735,0.184811284388065));
#23722=CARTESIAN_POINT('Ctrl Pts',(158.707317174883,3.21622720968354,1.24165519098984));
#23723=CARTESIAN_POINT('Ctrl Pts',(158.759932846849,2.80822363056973,2.29849909759162));
#23724=CARTESIAN_POINT('Ctrl Pts',(158.812548518815,1.82848850149854,3.13461864273479));
#23725=CARTESIAN_POINT('Ctrl Pts',(158.865164190781,0.720648566411499,3.37142136336576));
#23726=CARTESIAN_POINT('Ctrl Pts',(158.917779862748,-0.38719136867554,3.60822408399673));
#23727=CARTESIAN_POINT('Ctrl Pts',(158.970395534714,-1.62313610977842,3.2457099801155));
#23728=CARTESIAN_POINT('Ctrl Pts',(159.02301120668,-2.42754973893992,2.44802417358987));
#23729=CARTESIAN_POINT('Ctrl Pts',(159.064900652901,-3.06797568427348,1.81295451762713));
#23730=CARTESIAN_POINT('Ctrl Pts',(159.106790099122,-3.43488035732093,0.902056040806694));
#23731=CARTESIAN_POINT('Ctrl Pts',(159.148679545343,-3.44306193045544,-0.00296971903132968));
#23732=CARTESIAN_POINT('Origin',(165.,0.,0.));
#23733=CARTESIAN_POINT('',(160.293320454657,-3.44534347095755,0.00235542500143092));
#23734=CARTESIAN_POINT('',(160.148679545343,-3.44537846153824,0.0023402370110744));
#23735=CARTESIAN_POINT('',(165.,-3.442,-4.21523428266519E-16));
#23736=CARTESIAN_POINT('Ctrl Pts',(160.293320454657,-3.44534347095755,0.00235542500143092));
#23737=CARTESIAN_POINT('Ctrl Pts',(160.28634420718,-3.44652575450077,0.152819085738542));
#23738=CARTESIAN_POINT('Ctrl Pts',(160.279367959703,-3.43751163365742,0.303140213126026));
#23739=CARTESIAN_POINT('Ctrl Pts',(160.272391712226,-3.41781664333112,0.452048662995567));
#23740=CARTESIAN_POINT('Ctrl Pts',(160.21977604026,-3.26927472967131,1.57513355602034));
#23741=CARTESIAN_POINT('Ctrl Pts',(160.167160368294,-2.51316733167226,2.61786037503484));
#23742=CARTESIAN_POINT('Ctrl Pts',(160.114544696328,-1.49186052305688,3.10808152767139));
#23743=CARTESIAN_POINT('Ctrl Pts',(160.061929024361,-0.470553714441506,
3.59830268030795));
#23744=CARTESIAN_POINT('Ctrl Pts',(160.009313352395,0.815952504790201,3.53601816656657));
#23745=CARTESIAN_POINT('Ctrl Pts',(159.956697680429,1.78512702507273,2.9494304702973));
#23746=CARTESIAN_POINT('Ctrl Pts',(159.904082008463,2.75430154535527,2.36284277402803));
#23747=CARTESIAN_POINT('Ctrl Pts',(159.851466336497,3.40614436668863,1.25195189523086));
#23748=CARTESIAN_POINT('Ctrl Pts',(159.798850664531,3.44550050263555,0.119770162913145));
#23749=CARTESIAN_POINT('Ctrl Pts',(159.746234992565,3.48485663858247,-1.01241156940458));
#23750=CARTESIAN_POINT('Ctrl Pts',(159.693619320599,2.91172608914295,-2.16588415524284));
#23751=CARTESIAN_POINT('Ctrl Pts',(159.641003648632,1.98562285942401,-2.81835421390573));
#23752=CARTESIAN_POINT('Ctrl Pts',(159.588387976666,1.05951962970507,-3.47082427256861));
#23753=CARTESIAN_POINT('Ctrl Pts',(159.5357723047,-0.219556280293278,-3.6222918040561));
#23754=CARTESIAN_POINT('Ctrl Pts',(159.483156632734,-1.27243821963341,-3.20417220625212));
#23755=CARTESIAN_POINT('Ctrl Pts',(159.430540960768,-2.32532015897354,-2.78605260844815));
#23756=CARTESIAN_POINT('Ctrl Pts',(159.377925288802,-3.15200812765545,-1.79834588135271));
#23757=CARTESIAN_POINT('Ctrl Pts',(159.325309616835,-3.37817709101225,-0.688286420840833));
#23758=CARTESIAN_POINT('Ctrl Pts',(159.314646562776,-3.42401232969197,-0.463322572724454));
#23759=CARTESIAN_POINT('Ctrl Pts',(159.303983508716,-3.44518378279179,-0.233333602080165));
#23760=CARTESIAN_POINT('Ctrl Pts',(159.293320454657,-3.44310231280533,-0.00296426346809486));
#23761=CARTESIAN_POINT('Ctrl Pts',(159.148679545343,-3.44306193045544,-0.00296971903132968));
#23762=CARTESIAN_POINT('Ctrl Pts',(159.159405771088,-3.4451569068351,-0.234710920714154));
#23763=CARTESIAN_POINT('Ctrl Pts',(159.170131996833,-3.42373152283689,-0.466067066570195));
#23764=CARTESIAN_POINT('Ctrl Pts',(159.180858222578,-3.37735531801846,-0.692308646474397));
#23765=CARTESIAN_POINT('Ctrl Pts',(159.233473894544,-3.14986475071538,-1.80209815084305));
#23766=CARTESIAN_POINT('Ctrl Pts',(159.28608956651,-2.32200109888913,-2.78881965041033));
#23767=CARTESIAN_POINT('Ctrl Pts',(159.338705238477,-1.2686219519135,-3.20568519574602));
#23768=CARTESIAN_POINT('Ctrl Pts',(159.391320910443,-0.215242804937871,
-3.62255074108171));
#23769=CARTESIAN_POINT('Ctrl Pts',(159.443936582409,1.06365183718713,-3.4695603321858));
#23770=CARTESIAN_POINT('Ctrl Pts',(159.496552254375,1.98897750290621,-2.81598796579658));
#23771=CARTESIAN_POINT('Ctrl Pts',(159.549167926341,2.91430316862528,-2.16241559940735));
#23772=CARTESIAN_POINT('Ctrl Pts',(159.601783598307,3.48605985793843,-1.00826127552482));
#23773=CARTESIAN_POINT('Ctrl Pts',(159.654399270274,3.44535560072704,0.123872851661023));
#23774=CARTESIAN_POINT('Ctrl Pts',(159.70701494224,3.40465134351564,1.25600697884687));
#23775=CARTESIAN_POINT('Ctrl Pts',(159.759630614206,2.75148613977968,2.36612090933602));
#23776=CARTESIAN_POINT('Ctrl Pts',(159.812246286172,1.78161377659822,2.95155415751702));
#23777=CARTESIAN_POINT('Ctrl Pts',(159.864861958138,0.811741413416756,3.53698740569803));
#23778=CARTESIAN_POINT('Ctrl Pts',(159.917477630104,-0.474838109210224,
3.59773997157089));
#23779=CARTESIAN_POINT('Ctrl Pts',(159.97009330207,-1.49556050213205,3.10630301852266));
#23780=CARTESIAN_POINT('Ctrl Pts',(160.022708974037,-2.51628289505388,2.61486606547443));
#23781=CARTESIAN_POINT('Ctrl Pts',(160.075324646003,-3.27114815827057,1.57123959350512));
#23782=CARTESIAN_POINT('Ctrl Pts',(160.127940317969,-3.41835265168146,0.447978568532901));
#23783=CARTESIAN_POINT('Ctrl Pts',(160.13485339376,-3.43769357771655,0.30039538069199));
#23784=CARTESIAN_POINT('Ctrl Pts',(160.141766469552,-3.44654454951433,0.151437473833138));
#23785=CARTESIAN_POINT('Ctrl Pts',(160.148679545343,-3.44537846153824,0.0023402370110744));
#23786=CARTESIAN_POINT('Origin',(165.,0.,0.));
#23787=CARTESIAN_POINT('',(161.293320454657,-3.43667385388915,0.000584777541659254));
#23788=CARTESIAN_POINT('',(161.148679545343,-3.43668114569526,0.000606329579010968));
#23789=CARTESIAN_POINT('',(165.,-3.442,-4.21523428266519E-16));
#23790=CARTESIAN_POINT('Ctrl Pts',(161.293320454657,-3.43667385388915,0.000584777541659254));
#23791=CARTESIAN_POINT('Ctrl Pts',(161.268704905644,-3.43749408857896,0.534915952136021));
#23792=CARTESIAN_POINT('Ctrl Pts',(161.24408935663,-3.32026410406894,1.06890639556271));
#23793=CARTESIAN_POINT('Ctrl Pts',(161.219473807617,-3.0830792634662,1.54286773768467));
#23794=CARTESIAN_POINT('Ctrl Pts',(161.166858135651,-2.57609728383533,2.5559588732179));
#23795=CARTESIAN_POINT('Ctrl Pts',(161.114242463684,-1.52105414681311,3.29478334035705));
#23796=CARTESIAN_POINT('Ctrl Pts',(161.061626791718,-0.395674282548231,
3.42480079172139));
#23797=CARTESIAN_POINT('Ctrl Pts',(161.009011119752,0.729705581716644,3.55481824308572));
#23798=CARTESIAN_POINT('Ctrl Pts',(160.956395447786,1.92542217322419,3.07602867867524));
#23799=CARTESIAN_POINT('Ctrl Pts',(160.90377977582,2.65005400196605,2.20522842068367));
#23800=CARTESIAN_POINT('Ctrl Pts',(160.851164103854,3.37468583070791,1.33442816269211));
#23801=CARTESIAN_POINT('Ctrl Pts',(160.798548431887,3.62823289668411,0.0716172111194516));
#23802=CARTESIAN_POINT('Ctrl Pts',(160.745932759921,3.29588887265298,-1.01140256077362));
#23803=CARTESIAN_POINT('Ctrl Pts',(160.693317087955,2.96354484862186,-2.09442233266669));
#23804=CARTESIAN_POINT('Ctrl Pts',(160.640701415989,2.04530973458342,-2.99765092488018));
#23805=CARTESIAN_POINT('Ctrl Pts',(160.588085744023,0.956961171534698,-3.31210566215452));
#23806=CARTESIAN_POINT('Ctrl Pts',(160.535470072057,-0.131387391514026,
-3.62656039942887));
#23807=CARTESIAN_POINT('Ctrl Pts',(160.482854400091,-1.38984940357303,-3.35224128176408));
#23808=CARTESIAN_POINT('Ctrl Pts',(160.430238728125,-2.24859219494225,-2.61336023941416));
#23809=CARTESIAN_POINT('Ctrl Pts',(160.384599303635,-2.99347533180661,-1.97244652913118));
#23810=CARTESIAN_POINT('Ctrl Pts',(160.338959879146,-3.43760883415252,-0.981995389001479));
#23811=CARTESIAN_POINT('Ctrl Pts',(160.293320454657,-3.44534347095755,0.00235542500143092));
#23812=CARTESIAN_POINT('Ctrl Pts',(160.148679545343,-3.44537846153824,0.0023402370110744));
#23813=CARTESIAN_POINT('Ctrl Pts',(160.194382141518,-3.43766941140137,-0.983347033151559));
#23814=CARTESIAN_POINT('Ctrl Pts',(160.240084737693,-2.992156718107,-1.97512383126673));
#23815=CARTESIAN_POINT('Ctrl Pts',(160.285787333867,-2.24547881951396,-2.61603602984151));
#23816=CARTESIAN_POINT('Ctrl Pts',(160.338403005833,-1.38585677033047,-3.35389402526855));
#23817=CARTESIAN_POINT('Ctrl Pts',(160.3910186778,-0.127068948358405,-3.6267144381475));
#23818=CARTESIAN_POINT('Ctrl Pts',(160.443634349766,0.960904451181222,-3.31096395059576));
#23819=CARTESIAN_POINT('Ctrl Pts',(160.496250021732,2.04887785072085,-2.99521346304401));
#23820=CARTESIAN_POINT('Ctrl Pts',(160.548865693698,2.96603682782804,-2.09089207506157));
#23821=CARTESIAN_POINT('Ctrl Pts',(160.601481365664,3.29709101648908,-1.00747728196484));
#23822=CARTESIAN_POINT('Ctrl Pts',(160.65409703763,3.62814520515012,0.0759375111318684));
#23823=CARTESIAN_POINT('Ctrl Pts',(160.706712709597,3.37309460536501,1.33844570934286));
#23824=CARTESIAN_POINT('Ctrl Pts',(160.759328381563,2.64742634612698,2.20838252698244));
#23825=CARTESIAN_POINT('Ctrl Pts',(160.811944053529,1.92175808688896,3.07831934462203));
#23826=CARTESIAN_POINT('Ctrl Pts',(160.864559725495,0.725472168198008,3.55568478169021));
#23827=CARTESIAN_POINT('Ctrl Pts',(160.917175397461,-0.39975212828439,3.42432736177104));
#23828=CARTESIAN_POINT('Ctrl Pts',(160.969791069427,-1.52497642476679,3.29296994185187));
#23829=CARTESIAN_POINT('Ctrl Pts',(161.022406741393,-2.57913909904063,2.55288966494535));
#23830=CARTESIAN_POINT('Ctrl Pts',(161.07502241336,-3.08491439514982,1.53919551030916));
#23831=CARTESIAN_POINT('Ctrl Pts',(161.099574790687,-3.32092745835213,1.06616912007933));
#23832=CARTESIAN_POINT('Ctrl Pts',(161.124127168015,-3.43752952918348,0.533563487206253));
#23833=CARTESIAN_POINT('Ctrl Pts',(161.148679545343,-3.43668114569526,0.000606329579010967));
#23834=CARTESIAN_POINT('Origin',(165.,0.,0.));
#23835=CARTESIAN_POINT('',(162.293320454657,-3.4432958299264,-0.0029358085113948));
#23836=CARTESIAN_POINT('',(162.148679545343,-3.44325559759246,-0.00294208160319024));
#23837=CARTESIAN_POINT('',(165.,-3.442,-4.21523428266519E-16));
#23838=CARTESIAN_POINT('Ctrl Pts',(162.293320454657,-3.4432958299264,-0.0029358085113948));
#23839=CARTESIAN_POINT('Ctrl Pts',(162.251065604107,-3.43507546920982,0.909824409735672));
#23840=CARTESIAN_POINT('Ctrl Pts',(162.208810753557,-3.06104050140918,1.82854105791307));
#23841=CARTESIAN_POINT('Ctrl Pts',(162.166555903007,-2.41063103125263,2.46468590939444));
#23842=CARTESIAN_POINT('Ctrl Pts',(162.113940231041,-1.6007422047593,3.25681245564849));
#23843=CARTESIAN_POINT('Ctrl Pts',(162.061324559075,-0.362329451333632,
3.61080605212497));
#23844=CARTESIAN_POINT('Ctrl Pts',(162.008708887109,0.743852880554024,3.36637809713911));
#23845=CARTESIAN_POINT('Ctrl Pts',(161.956093215143,1.85003521244167,3.12195014215324));
#23846=CARTESIAN_POINT('Ctrl Pts',(161.903477543177,2.82398712279132,2.27910063570504));
#23847=CARTESIAN_POINT('Ctrl Pts',(161.850861871211,3.22470235789767,1.21947255146401));
#23848=CARTESIAN_POINT('Ctrl Pts',(161.798246199244,3.62541759300402,0.159844467222955));
#23849=CARTESIAN_POINT('Ctrl Pts',(161.745630527278,3.45289615286705,-1.11656219481094));
#23850=CARTESIAN_POINT('Ctrl Pts',(161.693014855312,2.78525589237232,-2.03178941202339));
#23851=CARTESIAN_POINT('Ctrl Pts',(161.640399183346,2.11761563187759,-2.94701662923583));
#23852=CARTESIAN_POINT('Ctrl Pts',(161.58778351138,0.954856551025132,-3.50106440162682));
#23853=CARTESIAN_POINT('Ctrl Pts',(161.535167839414,-0.176523049025896,
-3.44305942643655));
#23854=CARTESIAN_POINT('Ctrl Pts',(161.482552167448,-1.30790264907693,-3.38505445124627));
#23855=CARTESIAN_POINT('Ctrl Pts',(161.429936495481,-2.40790276832652,-2.71499672847472));
#23856=CARTESIAN_POINT('Ctrl Pts',(161.377320823515,-2.97844241683156,-1.73628896512529));
#23857=CARTESIAN_POINT('Ctrl Pts',(161.349320700562,-3.28206260660803,-1.21545673616016));
#23858=CARTESIAN_POINT('Ctrl Pts',(161.32132057761,-3.43574083906375,-0.607215543224034));
#23859=CARTESIAN_POINT('Ctrl Pts',(161.293320454657,-3.43667385388915,0.000584777541659254));
#23860=CARTESIAN_POINT('Ctrl Pts',(161.148679545343,-3.43668114569526,0.000606329579010967));
#23861=CARTESIAN_POINT('Ctrl Pts',(161.176742839981,-3.4357114458785,-0.608562124634891));
#23862=CARTESIAN_POINT('Ctrl Pts',(161.20480613462,-3.28129951189907,-1.21818982563464));
#23863=CARTESIAN_POINT('Ctrl Pts',(161.232869429258,-2.97637293604331,-1.73983441449399));
#23864=CARTESIAN_POINT('Ctrl Pts',(161.285485101224,-2.40466826288309,-2.71786215229505));
#23865=CARTESIAN_POINT('Ctrl Pts',(161.33810077319,-1.30387099861813,-3.38660959553132));
#23866=CARTESIAN_POINT('Ctrl Pts',(161.390716445156,-0.172423081110959,
-3.44326733285217));
#23867=CARTESIAN_POINT('Ctrl Pts',(161.443332117123,0.959024836396215,-3.49992507017301));
#23868=CARTESIAN_POINT('Ctrl Pts',(161.495947789089,2.1211234071456,-2.94449310157842));
#23869=CARTESIAN_POINT('Ctrl Pts',(161.548563461055,2.78767340950389,-2.02847149506462));
#23870=CARTESIAN_POINT('Ctrl Pts',(161.601179133021,3.45422341186218,-1.11244988855083));
#23871=CARTESIAN_POINT('Ctrl Pts',(161.653794804987,3.62522484582938,0.164161355882143));
#23872=CARTESIAN_POINT('Ctrl Pts',(161.706410476953,3.22324811661227,1.2233115805444));
#23873=CARTESIAN_POINT('Ctrl Pts',(161.75902614892,2.82127138739515,2.28246180520667));
#23874=CARTESIAN_POINT('Ctrl Pts',(161.811641820886,1.84631649499369,3.12415101009821));
#23875=CARTESIAN_POINT('Ctrl Pts',(161.864257492852,0.739843844237031,3.36726160707729));
#23876=CARTESIAN_POINT('Ctrl Pts',(161.916873164818,-0.366628806519617,
3.61037220405638));
#23877=CARTESIAN_POINT('Ctrl Pts',(161.969488836784,-1.60461921563146,3.25490419312303));
#23878=CARTESIAN_POINT('Ctrl Pts',(162.02210450875,-2.41356427249153,2.46181379208476));
#23879=CARTESIAN_POINT('Ctrl Pts',(162.064296187615,-3.06224457595425,1.82584708747844));
#23880=CARTESIAN_POINT('Ctrl Pts',(162.106487866479,-3.43504084200054,0.908481152668783));
#23881=CARTESIAN_POINT('Ctrl Pts',(162.148679545343,-3.44325559759246,-0.00294208160319024));
#23882=CARTESIAN_POINT('Origin',(165.,0.,0.));
#23883=CARTESIAN_POINT('',(163.293320454657,-3.44517452324429,0.00242599488633463));
#23884=CARTESIAN_POINT('',(163.148679545343,-3.4452102901939,0.00241153213425219));
#23885=CARTESIAN_POINT('',(165.,-3.442,-4.21523428266519E-16));
#23886=CARTESIAN_POINT('Ctrl Pts',(163.293320454657,-3.44517452324429,0.00242599488633463));
#23887=CARTESIAN_POINT('Ctrl Pts',(163.286041974537,-3.44643442364397,0.159428330452332));
#23888=CARTESIAN_POINT('Ctrl Pts',(163.278763494417,-3.43661887138664,0.316272314327839));
#23889=CARTESIAN_POINT('Ctrl Pts',(163.271485014297,-3.41518589515111,0.471512356536619));
#23890=CARTESIAN_POINT('Ctrl Pts',(163.21886934233,-3.2602482669296,1.59373279295724));
#23891=CARTESIAN_POINT('Ctrl Pts',(163.166253670364,-2.49821280746788,2.63213520662755));
#23892=CARTESIAN_POINT('Ctrl Pts',(163.113637998398,-1.47412982119765,3.11653010109987));
#23893=CARTESIAN_POINT('Ctrl Pts',(163.061022326432,-0.450046834927408,
3.6009249955722));
#23894=CARTESIAN_POINT('Ctrl Pts',(163.008406654466,0.836083678151346,3.53131237084653));
#23895=CARTESIAN_POINT('Ctrl Pts',(162.9557909825,1.80190072739622,2.93921288262942));
#23896=CARTESIAN_POINT('Ctrl Pts',(162.903175310534,2.76771777664108,2.34711339441232));
#23897=CARTESIAN_POINT('Ctrl Pts',(162.850559638567,3.41322136205207,1.2325270427038));
#23898=CARTESIAN_POINT('Ctrl Pts',(162.797943966601,3.44612691092026,0.100139475917283));
#23899=CARTESIAN_POINT('Ctrl Pts',(162.745328294635,3.47903245978844,-1.03224809086925));
#23900=CARTESIAN_POINT('Ctrl Pts',(162.692712622669,2.8993399721138,-2.18243687273376));
#23901=CARTESIAN_POINT('Ctrl Pts',(162.640096950703,1.96953469955406,-2.82962041059543));
#23902=CARTESIAN_POINT('Ctrl Pts',(162.587481278737,1.03972942699433,-3.47680394845709));
#23903=CARTESIAN_POINT('Ctrl Pts',(162.53486560677,-0.240188630450497,-3.62098224231593));
#23904=CARTESIAN_POINT('Ctrl Pts',(162.482249934804,-1.29067148733502,-3.1968712380367));
#23905=CARTESIAN_POINT('Ctrl Pts',(162.429634262838,-2.34115434421955,-2.77276023375746));
#23906=CARTESIAN_POINT('Ctrl Pts',(162.377018590872,-3.16220200054378,-1.78035993134015));
#23907=CARTESIAN_POINT('Ctrl Pts',(162.324402918906,-3.38204337892538,-0.669030032115677));
#23908=CARTESIAN_POINT('Ctrl Pts',(162.31404209749,-3.42533347056955,-0.450192370441127));
#23909=CARTESIAN_POINT('Ctrl Pts',(162.303681276073,-3.44531144915719,-0.226743146465491));
#23910=CARTESIAN_POINT('Ctrl Pts',(162.293320454657,-3.4432958299264,-0.0029358085113948));
#23911=CARTESIAN_POINT('Ctrl Pts',(162.148679545343,-3.44325559759246,-0.00294208160319024));
#23912=CARTESIAN_POINT('Ctrl Pts',(162.159103538445,-3.44528515787374,-0.22812083159991));
#23913=CARTESIAN_POINT('Ctrl Pts',(162.169527531547,-3.42506065804876,-0.452936839079066));
#23914=CARTESIAN_POINT('Ctrl Pts',(162.179951524649,-3.38124447682805,-0.673056782348974));
#23915=CARTESIAN_POINT('Ctrl Pts',(162.232567196615,-3.1600799196962,-1.78412416460122));
#23916=CARTESIAN_POINT('Ctrl Pts',(162.285182868581,-2.3378511008242,-2.77554613796251));
#23917=CARTESIAN_POINT('Ctrl Pts',(162.337798540547,-1.28686392900068,-3.19840598933041));
#23918=CARTESIAN_POINT('Ctrl Pts',(162.390414212513,-0.235876757177136,
-3.62126584069832));
#23919=CARTESIAN_POINT('Ctrl Pts',(162.443029884479,1.04386876759795,-3.47556357007279));
#23920=CARTESIAN_POINT('Ctrl Pts',(162.495645556446,1.97290278281865,-2.827273289566));
#23921=CARTESIAN_POINT('Ctrl Pts',(162.548261228412,2.90193679803933,-2.17898300905921));
#23922=CARTESIAN_POINT('Ctrl Pts',(162.600876900378,3.48025930370564,-1.02810471867118));
#23923=CARTESIAN_POINT('Ctrl Pts',(162.653492572344,3.44600537717898,0.104242912471304));
#23924=CARTESIAN_POINT('Ctrl Pts',(162.70610824431,3.41175145065233,1.2365905436138));
#23925=CARTESIAN_POINT('Ctrl Pts',(162.758723916276,2.7649210919327,2.35040751551073));
#23926=CARTESIAN_POINT('Ctrl Pts',(162.811339588243,1.79839963781204,2.94135655558191));
#23927=CARTESIAN_POINT('Ctrl Pts',(162.863955260209,0.8318781836914,3.53230559565307));
#23928=CARTESIAN_POINT('Ctrl Pts',(162.916570932175,-0.454334365830267,
3.60038670389851));
#23929=CARTESIAN_POINT('Ctrl Pts',(162.969186604141,-1.47783987393939,3.11477269657705));
#23930=CARTESIAN_POINT('Ctrl Pts',(163.021802276107,-2.50134538204853,2.62915868925557));
#23931=CARTESIAN_POINT('Ctrl Pts',(163.074417948073,-3.26214384874513,1.58984956636719));
#23932=CARTESIAN_POINT('Ctrl Pts',(163.127033620039,-3.41574508097403,0.467445383064969));
#23933=CARTESIAN_POINT('Ctrl Pts',(163.134248928474,-3.43680877217194,0.313527509013778));
#23934=CARTESIAN_POINT('Ctrl Pts',(163.141464236908,-3.44645395580836,0.158047009967286));
#23935=CARTESIAN_POINT('Ctrl Pts',(163.148679545343,-3.4452102901939,0.00241153213425219));
#23936=CARTESIAN_POINT('Origin',(165.,0.,0.));
#23937=CARTESIAN_POINT('',(164.293320454657,-3.43664328220378,0.000481279145628788));
#23938=CARTESIAN_POINT('',(164.148679545343,-3.43664933101759,0.000502961695028516));
#23939=CARTESIAN_POINT('',(165.,-3.442,-4.21523428266519E-16));
#23940=CARTESIAN_POINT('Ctrl Pts',(164.293320454657,-3.43664328220378,0.000481279145628788));
#23941=CARTESIAN_POINT('Ctrl Pts',(164.268402673,-3.43732628447773,0.541385065300302));
#23942=CARTESIAN_POINT('Ctrl Pts',(164.243484891344,-3.31706603853791,1.08200166084634));
#23943=CARTESIAN_POINT('Ctrl Pts',(164.218567109687,-3.07423963801863,1.56040675749654));
#23944=CARTESIAN_POINT('Ctrl Pts',(164.165951437721,-2.5614943860317,2.57059321707906));
#23945=CARTESIAN_POINT('Ctrl Pts',(164.113335765755,-1.50225934571328,3.30339519821379));
#23946=CARTESIAN_POINT('Ctrl Pts',(164.060720093789,-0.37615704458299,3.42699934032914));
#23947=CARTESIAN_POINT('Ctrl Pts',(164.008104421823,0.749945256547313,3.5506034824445));
#23948=CARTESIAN_POINT('Ctrl Pts',(163.955488749856,1.94291481848948,3.06500978554047));
#23949=CARTESIAN_POINT('Ctrl Pts',(163.90287307789,2.66257400854294,2.1900954887487));
#23950=CARTESIAN_POINT('Ctrl Pts',(163.850257405924,3.38223319859638,1.31518119195694));
#23951=CARTESIAN_POINT('Ctrl Pts',(163.797641733958,3.62858201676113,0.0509462952774498));
#23952=CARTESIAN_POINT('Ctrl Pts',(163.745026061992,3.2900735085632,-1.03016256438313));
#23953=CARTESIAN_POINT('Ctrl Pts',(163.692410390026,2.95156500036526,-2.11127142404373));
#23954=CARTESIAN_POINT('Ctrl Pts',(163.63979471806,2.02819916580462,-3.00925424668543));
#23955=CARTESIAN_POINT('Ctrl Pts',(163.587179046093,0.938076840427768,-3.31750364615607));
#23956=CARTESIAN_POINT('Ctrl Pts',(163.534563374127,-0.152045484949063,
-3.62575304562671));
#23957=CARTESIAN_POINT('Ctrl Pts',(163.481947702161,-1.40892430114209,-3.34426902192632));
#23958=CARTESIAN_POINT('Ctrl Pts',(163.429332030195,-2.26344381074798,-2.60050778049066));
#23959=CARTESIAN_POINT('Ctrl Pts',(163.383994838349,-2.99975513198533,-1.95963321155401));
#23960=CARTESIAN_POINT('Ctrl Pts',(163.338657646503,-3.43732668342273,-0.975531613071623));
#23961=CARTESIAN_POINT('Ctrl Pts',(163.293320454657,-3.44517452324429,0.00242599488633463));
#23962=CARTESIAN_POINT('Ctrl Pts',(163.148679545343,-3.4452102901939,0.00241153213425219));
#23963=CARTESIAN_POINT('Ctrl Pts',(163.194079908875,-3.43738486297624,-0.976882331195102));
#23964=CARTESIAN_POINT('Ctrl Pts',(163.239480272406,-2.99844670811644,-1.96231213468243));
#23965=CARTESIAN_POINT('Ctrl Pts',(163.284880635938,-2.26034573001926,-2.60320126481429));
#23966=CARTESIAN_POINT('Ctrl Pts',(163.337496307904,-1.40494114907436,-3.34594448567534));
#23967=CARTESIAN_POINT('Ctrl Pts',(163.39011197987,-0.147727989423363,-3.62593168368139));
#23968=CARTESIAN_POINT('Ctrl Pts',(163.442727651836,0.942026560528155,-3.31638441734467));
#23969=CARTESIAN_POINT('Ctrl Pts',(163.495343323802,2.03178111047965,-3.00683715100795));
#23970=CARTESIAN_POINT('Ctrl Pts',(163.547958995769,2.95407705073166,-2.10775542032849));
#23971=CARTESIAN_POINT('Ctrl Pts',(163.600574667735,3.29129799479096,-1.02624419795294));
#23972=CARTESIAN_POINT('Ctrl Pts',(163.653190339701,3.62851893885027,0.0552670244226335));
#23973=CARTESIAN_POINT('Ctrl Pts',(163.705806011667,3.38066488671686,1.31920773849431));
#23974=CARTESIAN_POINT('Ctrl Pts',(163.758421683633,2.65996436408649,2.19326451349057));
#23975=CARTESIAN_POINT('Ctrl Pts',(163.811037355599,1.93926384145612,3.06732128848682));
#23976=CARTESIAN_POINT('Ctrl Pts',(163.863653027565,0.745716848328806,3.55149412440766));
#23977=CARTESIAN_POINT('Ctrl Pts',(163.916268699532,-0.380237521262959,
3.4265491491836));
#23978=CARTESIAN_POINT('Ctrl Pts',(163.968884371498,-1.50619189085473,3.30160417395954));
#23979=CARTESIAN_POINT('Ctrl Pts',(164.021500043464,-2.56455363691095,2.56754138759055));
#23980=CARTESIAN_POINT('Ctrl Pts',(164.07411571543,-3.07609566029694,1.55674504433108));
#23981=CARTESIAN_POINT('Ctrl Pts',(164.098970325401,-3.31773806454547,1.07926470562088));
#23982=CARTESIAN_POINT('Ctrl Pts',(164.123824935372,-3.43736136450879,0.540033154696634));
#23983=CARTESIAN_POINT('Ctrl Pts',(164.148679545343,-3.43664933101759,0.000502961695028516));
#23984=CARTESIAN_POINT('Origin',(165.,0.,0.));
#23985=CARTESIAN_POINT('',(165.293320454657,-3.44348846335203,-0.00290342158797974));
#23986=CARTESIAN_POINT('',(165.148679545343,-3.44344843612552,-0.00291051544235242));
#23987=CARTESIAN_POINT('',(165.,-3.442,-4.21523428266519E-16));
#23988=CARTESIAN_POINT('Ctrl Pts',(165.293320454657,-3.44348846335203,-0.00290342158797974));
#23989=CARTESIAN_POINT('Ctrl Pts',(165.250763371464,-3.43524791269343,0.916252704056434));
#23990=CARTESIAN_POINT('Ctrl Pts',(165.208206288271,-3.0552517495188,1.84142636681851));
#23991=CARTESIAN_POINT('Ctrl Pts',(165.165649205078,-2.396550793366,2.47837908634305));
#23992=CARTESIAN_POINT('Ctrl Pts',(165.113033533112,-1.58216242761392,3.26587890620758));
#23993=CARTESIAN_POINT('Ctrl Pts',(165.060417861146,-0.341753097329506,
3.61281161947734));
#23994=CARTESIAN_POINT('Ctrl Pts',(165.007802189179,0.7630187973166,3.36208579839172));
#23995=CARTESIAN_POINT('Ctrl Pts',(164.955186517213,1.86779069196271,3.11135997730611));
#23996=CARTESIAN_POINT('Ctrl Pts',(164.902570845247,2.8369251509705,2.26297562186511));
#23997=CARTESIAN_POINT('Ctrl Pts',(164.849955173281,3.23159726670101,1.20108189007092));
#23998=CARTESIAN_POINT('Ctrl Pts',(164.797339501315,3.62626938243153,0.139188158276714));
#23999=CARTESIAN_POINT('Ctrl Pts',(164.744723829349,3.44647915488475,-1.13621494987071));
#24000=CARTESIAN_POINT('Ctrl Pts',(164.692108157383,2.77363575207064,-2.0476238218094));
#24001=CARTESIAN_POINT('Ctrl Pts',(164.639492485417,2.10079234925652,-2.95903269374809));
#24002=CARTESIAN_POINT('Ctrl Pts',(164.58687681345,0.934895771175069,-3.50644732947806));
#24003=CARTESIAN_POINT('Ctrl Pts',(164.534261141484,-0.196135019600669,
-3.44199791616614));
#24004=CARTESIAN_POINT('Ctrl Pts',(164.481645469518,-1.32716581037639,-3.37754850285422));
#24005=CARTESIAN_POINT('Ctrl Pts',(164.429029797552,-2.42333081384639,-2.70123504050043));
#24006=CARTESIAN_POINT('Ctrl Pts',(164.376414125586,-2.98828558375369,-1.71929284030839));
#24007=CARTESIAN_POINT('Ctrl Pts',(164.348716235276,-3.28568851831746,-1.20237979263726));
#24008=CARTESIAN_POINT('Ctrl Pts',(164.321018344967,-3.43588407649575,-0.600771831723536));
#24009=CARTESIAN_POINT('Ctrl Pts',(164.293320454657,-3.43664328220378,0.000481279145628788));
#24010=CARTESIAN_POINT('Ctrl Pts',(164.148679545343,-3.43664933101759,0.000502961695028516));
#24011=CARTESIAN_POINT('Ctrl Pts',(164.176440607338,-3.43585403364963,-0.602118892102288));
#24012=CARTESIAN_POINT('Ctrl Pts',(164.204201669333,-3.28493429195908,-1.20511331706909));
#24013=CARTESIAN_POINT('Ctrl Pts',(164.231962731329,-2.98623633469664,-1.72285002181984));
#24014=CARTESIAN_POINT('Ctrl Pts',(164.284578403295,-2.42011268499457,-2.70411884456138));
#24015=CARTESIAN_POINT('Ctrl Pts',(164.337194075261,-1.32314308487464,-3.3791265898945));
#24016=CARTESIAN_POINT('Ctrl Pts',(164.389809747227,-0.192036302641559,
-3.44222917639352));
#24017=CARTESIAN_POINT('Ctrl Pts',(164.442425419193,0.939070479591511,-3.50533176289254));
#24018=CARTESIAN_POINT('Ctrl Pts',(164.495041091159,2.10431444393775,-2.95652919055749));
#24019=CARTESIAN_POINT('Ctrl Pts',(164.547656763125,2.7760721318787,-2.04431973109724));
#24020=CARTESIAN_POINT('Ctrl Pts',(164.600272435091,3.44782981981966,-1.13211027163698));
#24021=CARTESIAN_POINT('Ctrl Pts',(164.652888107058,3.62610123135531,0.14350607494847));
#24022=CARTESIAN_POINT('Ctrl Pts',(164.705503779024,3.23016491965784,1.20492914155103));
#24023=CARTESIAN_POINT('Ctrl Pts',(164.75811945099,2.83422860796038,2.26635220815355));
#24024=CARTESIAN_POINT('Ctrl Pts',(164.810735122956,1.86408457302983,3.11358199477318));
#24025=CARTESIAN_POINT('Ctrl Pts',(164.863350794922,0.759014859341979,3.36299213315243));
#24026=CARTESIAN_POINT('Ctrl Pts',(164.915966466888,-0.3460548543459,3.61240227153168));
#24027=CARTESIAN_POINT('Ctrl Pts',(164.968582138854,-1.58605024679109,3.26399276167052));
#24028=CARTESIAN_POINT('Ctrl Pts',(165.021197810821,-2.39950034922871,2.47552372608269));
#24029=CARTESIAN_POINT('Ctrl Pts',(165.063691722328,-3.05646576232802,1.83873373229116));
#24030=CARTESIAN_POINT('Ctrl Pts',(165.106185633836,-3.43521118804265,0.914908906409425));
#24031=CARTESIAN_POINT('Ctrl Pts',(165.148679545343,-3.44344843612552,-0.00291051544235242));
#24032=CARTESIAN_POINT('Origin',(165.,0.,0.));
#24033=CARTESIAN_POINT('',(166.293320454657,-3.44500202379557,0.00249305976498276));
#24034=CARTESIAN_POINT('',(166.148679545343,-3.44503851029087,0.00247933530702656));
#24035=CARTESIAN_POINT('',(165.,-3.442,-4.21523428266519E-16));
#24036=CARTESIAN_POINT('Ctrl Pts',(166.293320454657,-3.44500202379557,0.00249305976498276));
#24037=CARTESIAN_POINT('Ctrl Pts',(166.285739741894,-3.44633958802846,0.166036157384798));
#24038=CARTESIAN_POINT('Ctrl Pts',(166.27815902913,-3.43568802025806,0.329404290985655));
#24039=CARTESIAN_POINT('Ctrl Pts',(166.270578316367,-3.41244430662922,0.490960746862352));
#24040=CARTESIAN_POINT('Ctrl Pts',(166.217962644401,-3.25111599229308,1.61228030504036));
#24041=CARTESIAN_POINT('Ctrl Pts',(166.165346972435,-2.48317720304131,2.64632461267713));
#24042=CARTESIAN_POINT('Ctrl Pts',(166.112731300469,-1.45635127605751,3.12487752744511));
#24043=CARTESIAN_POINT('Ctrl Pts',(166.060115628503,-0.429525349073735,
3.60343044221307));
#24044=CARTESIAN_POINT('Ctrl Pts',(166.007499956536,0.856187715642067,3.52649196411227));
#24045=CARTESIAN_POINT('Ctrl Pts',(165.95488428457,1.81861594842145,2.92889990149082));
#24046=CARTESIAN_POINT('Ctrl Pts',(165.902268612604,2.78104418120086,2.33130783886936));
#24047=CARTESIAN_POINT('Ctrl Pts',(165.849652940638,3.42018758204383,1.21306219172721));
#24048=CARTESIAN_POINT('Ctrl Pts',(165.797037268672,3.44664147522546,0.0805055405637458));
#24049=CARTESIAN_POINT('Ctrl Pts',(165.744421596706,3.47309536840708,-1.05205111059968));
#24050=CARTESIAN_POINT('Ctrl Pts',(165.691805924739,2.88685975392742,-2.19891876578441));
#24051=CARTESIAN_POINT('Ctrl Pts',(165.639190252773,1.95338261682879,-2.84079477489608));
#24052=CARTESIAN_POINT('Ctrl Pts',(165.586574580807,1.01990547973014,-3.48267078400776));
#24053=CARTESIAN_POINT('Ctrl Pts',(165.533958908841,-0.260813179987495,
-3.61955514704634));
#24054=CARTESIAN_POINT('Ctrl Pts',(165.481343236875,-1.30886286348838,-3.18946650795815));
#24055=CARTESIAN_POINT('Ctrl Pts',(165.428727564909,-2.35691254698925,-2.75937786886997));
#24056=CARTESIAN_POINT('Ctrl Pts',(165.376111892942,-3.17229325427339,-1.76231622765505));
#24057=CARTESIAN_POINT('Ctrl Pts',(165.323496220976,-3.3857999073056,-0.649751943817944));
#24058=CARTESIAN_POINT('Ctrl Pts',(165.313437632203,-3.42661618015608,-0.437061956279473));
#24059=CARTESIAN_POINT('Ctrl Pts',(165.30337904343,-3.44543616051829,-0.220150770149137));
#24060=CARTESIAN_POINT('Ctrl Pts',(165.293320454657,-3.44348846335203,-0.00290342158797974));
#24061=CARTESIAN_POINT('Ctrl Pts',(165.148679545343,-3.44344843612552,-0.00291051544235242));
#24062=CARTESIAN_POINT('Ctrl Pts',(165.158801305802,-3.44541049254668,-0.221528853993161));
#24063=CARTESIAN_POINT('Ctrl Pts',(165.16892306626,-3.42635139806872,-0.43980646995822));
#24064=CARTESIAN_POINT('Ctrl Pts',(165.179044826719,-3.38502395824774,-0.653783179988487));
#24065=CARTESIAN_POINT('Ctrl Pts',(165.231660498685,-3.1701926523991,-1.76609248915746));
#24066=CARTESIAN_POINT('Ctrl Pts',(165.284276170651,-2.35362522827174,-2.7621825461809));
#24067=CARTESIAN_POINT('Ctrl Pts',(165.336891842617,-1.30506411029719,-3.19102292570286));
#24068=CARTESIAN_POINT('Ctrl Pts',(165.389507514584,-0.256502992322657,
-3.61986330522481));
#24069=CARTESIAN_POINT('Ctrl Pts',(165.44212318655,1.02405181949904,-3.48145400724529));
#24070=CARTESIAN_POINT('Ctrl Pts',(165.494738858516,1.95676401679889,-2.83846687965671));
#24071=CARTESIAN_POINT('Ctrl Pts',(165.547354530482,2.88947621409875,-2.19547975206813));
#24072=CARTESIAN_POINT('Ctrl Pts',(165.599970202448,3.47434579687675,-1.04791479487049));
#24073=CARTESIAN_POINT('Ctrl Pts',(165.652585874414,3.44654332040737,0.0846096028970402));
#24074=CARTESIAN_POINT('Ctrl Pts',(165.70520154638,3.41874084393799,1.21713400066456));
#24075=CARTESIAN_POINT('Ctrl Pts',(165.757817218347,2.77826630822123,2.334617839002));
#24076=CARTESIAN_POINT('Ctrl Pts',(165.810432890313,1.81512712798546,2.93106348508494));
#24077=CARTESIAN_POINT('Ctrl Pts',(165.863048562279,0.851987947749686,3.5275091311679));
#24078=CARTESIAN_POINT('Ctrl Pts',(165.915664234245,-0.433815877005108,
3.60291658499637));
#24079=CARTESIAN_POINT('Ctrl Pts',(165.968279906211,-1.46007128038759,3.12314128731545));
#24080=CARTESIAN_POINT('Ctrl Pts',(166.020895578177,-2.48632668377006,2.64336598963453));
#24081=CARTESIAN_POINT('Ctrl Pts',(166.073511250144,-3.25303366578022,1.60840794044424));
#24082=CARTESIAN_POINT('Ctrl Pts',(166.12612692211,-3.41302665260159,0.486897025025004));
#24083=CARTESIAN_POINT('Ctrl Pts',(166.133644463187,-3.43588588456886,0.326659512876953));
#24084=CARTESIAN_POINT('Ctrl Pts',(166.141162004265,-3.44635984905697,0.164655137910781));
#24085=CARTESIAN_POINT('Ctrl Pts',(166.148679545343,-3.44503851029087,0.00247933530702656));
#24086=CARTESIAN_POINT('Origin',(165.,0.,0.));
#24087=CARTESIAN_POINT('',(167.293320454657,-3.4366186727045,0.000377228489918668));
#24088=CARTESIAN_POINT('',(167.148679545343,-3.43662347336092,0.000399016594708752));
#24089=CARTESIAN_POINT('',(165.,-3.442,-4.21523428266519E-16));
#24090=CARTESIAN_POINT('Ctrl Pts',(167.293320454657,-3.4366186727045,0.000377228489918668));
#24091=CARTESIAN_POINT('Ctrl Pts',(167.268100440357,-3.43716028314427,0.547851542709962));
#24092=CARTESIAN_POINT('Ctrl Pts',(167.242880426057,-3.31382643177038,1.09509536773555));
#24093=CARTESIAN_POINT('Ctrl Pts',(167.217660411758,-3.0653002376201,1.5778951340479));
#24094=CARTESIAN_POINT('Ctrl Pts',(167.165044739791,-2.54680835450729,2.58514413191544));
#24095=CARTESIAN_POINT('Ctrl Pts',(167.112429067825,-1.48341578853514,3.31189984384937));
#24096=CARTESIAN_POINT('Ctrl Pts',(167.059813395859,-0.356627598376805,
3.42908666511678));
#24097=CARTESIAN_POINT('Ctrl Pts',(167.007197723893,0.770160591781512,3.5462734863842));
#24098=CARTESIAN_POINT('Ctrl Pts',(166.954582051927,1.960344406126,3.05389141698511));
#24099=CARTESIAN_POINT('Ctrl Pts',(166.901966379961,2.67500760083863,2.17489147689288));
#24100=CARTESIAN_POINT('Ctrl Pts',(166.849350707995,3.38967079555127,1.29589153680066));
#24101=CARTESIAN_POINT('Ctrl Pts',(166.796735036029,3.62881337063205,0.0302737260152738));
#24102=CARTESIAN_POINT('Ctrl Pts',(166.744119364062,3.28415136460691,-1.04888913387277));
#24103=CARTESIAN_POINT('Ctrl Pts',(166.691503692096,2.93948935858177,-2.12805199376081));
#24104=CARTESIAN_POINT('Ctrl Pts',(166.63888802013,2.01102277145072,-3.02075990275153));
#24105=CARTESIAN_POINT('Ctrl Pts',(166.586272348164,0.919162063864181,-3.32279396008219));
#24106=CARTESIAN_POINT('Ctrl Pts',(166.533656676198,-0.172698643722376,
-3.62482801741286));
#24107=CARTESIAN_POINT('Ctrl Pts',(166.481041004232,-1.42795347176443,-3.33618822308345));
#24108=CARTESIAN_POINT('Ctrl Pts',(166.428425332266,-2.27822196607518,-2.58757092155912));
#24109=CARTESIAN_POINT('Ctrl Pts',(166.383390373063,-3.00598625230122,-1.94681222034209));
#24110=CARTESIAN_POINT('Ctrl Pts',(166.33835541386,-3.43705591733564,-0.969072142503072));
#24111=CARTESIAN_POINT('Ctrl Pts',(166.293320454657,-3.44500202379557,0.00249305976498276));
#24112=CARTESIAN_POINT('Ctrl Pts',(166.148679545343,-3.44503851029087,0.00247933530702656));
#24113=CARTESIAN_POINT('Ctrl Pts',(166.193777676231,-3.43711172838111,-0.970421976048281));
#24114=CARTESIAN_POINT('Ctrl Pts',(166.23887580712,-3.00468799405711,-1.94949273537325));
#24115=CARTESIAN_POINT('Ctrl Pts',(166.283973938008,-2.27513928018629,-2.59028201169302));
#24116=CARTESIAN_POINT('Ctrl Pts',(166.336589609974,-1.42397992931704,-3.33788635134359));
#24117=CARTESIAN_POINT('Ctrl Pts',(166.38920528194,-0.168382235945959,-3.62503124899654));
#24118=CARTESIAN_POINT('Ctrl Pts',(166.441820953907,0.923118096027443,-3.32169725067378));
#24119=CARTESIAN_POINT('Ctrl Pts',(166.494436625873,2.01461842800086,-3.01836325235101));
#24120=CARTESIAN_POINT('Ctrl Pts',(166.547052297839,2.94202139857659,-2.12455035805251));
#24121=CARTESIAN_POINT('Ctrl Pts',(166.599667969805,3.28539815358547,-1.04497780682858));
#24122=CARTESIAN_POINT('Ctrl Pts',(166.652283641771,3.62877490859433,0.0345947443953297));
#24123=CARTESIAN_POINT('Ctrl Pts',(166.704899313737,3.38812544803635,1.29992695254466));
#24124=CARTESIAN_POINT('Ctrl Pts',(166.757514985703,2.6724160524118,2.17807531714557));
#24125=CARTESIAN_POINT('Ctrl Pts',(166.81013065767,1.95670665678724,3.0562236817465));
#24126=CARTESIAN_POINT('Ctrl Pts',(166.862746329636,0.765937326096089,3.547188202799));
#24127=CARTESIAN_POINT('Ctrl Pts',(166.915362001602,-0.360710573543627,
3.42865972742716));
#24128=CARTESIAN_POINT('Ctrl Pts',(166.967977673568,-1.48735847318333,3.31013125205532));
#24129=CARTESIAN_POINT('Ctrl Pts',(167.020593345534,-2.5498849417716,2.58210978025916));
#24130=CARTESIAN_POINT('Ctrl Pts',(167.0732090175,-3.06717709026766,1.57424405391421));
#24131=CARTESIAN_POINT('Ctrl Pts',(167.098365860115,-3.31450714762519,1.09235874281813));
#24132=CARTESIAN_POINT('Ctrl Pts',(167.123522702729,-3.43719497569704,0.54650018122335));
#24133=CARTESIAN_POINT('Ctrl Pts',(167.148679545343,-3.43662347336092,0.000399016594708752));
#24134=CARTESIAN_POINT('Origin',(165.,0.,0.));
#24135=CARTESIAN_POINT('',(168.293320454657,-3.44367996564435,-0.0028671194461008));
#24136=CARTESIAN_POINT('',(168.148679545343,-3.44364019544098,-0.00287502992418087));
#24137=CARTESIAN_POINT('',(165.,-3.442,-4.21523428266519E-16));
#24138=CARTESIAN_POINT('Ctrl Pts',(168.293320454657,-3.44367996564435,-0.0028671194461008));
#24139=CARTESIAN_POINT('Ctrl Pts',(168.250461138821,-3.43543047620403,0.9226836846828));
#24140=CARTESIAN_POINT('Ctrl Pts',(168.207601822984,-3.04941537922053,1.85430521201957));
#24141=CARTESIAN_POINT('Ctrl Pts',(168.164742507148,-2.38239277503066,2.49199182709186));
#24142=CARTESIAN_POINT('Ctrl Pts',(168.112126835182,-1.56353130112863,3.2748393621314));
#24143=CARTESIAN_POINT('Ctrl Pts',(168.059511163216,-0.321165651672412,
3.61469993243571));
#24144=CARTESIAN_POINT('Ctrl Pts',(168.00689549125,0.782159950179274,3.35768438259772));
#24145=CARTESIAN_POINT('Ctrl Pts',(167.954279819284,1.88548555203095,3.10066883275973));
#24146=CARTESIAN_POINT('Ctrl Pts',(167.901664147318,2.84977110627809,2.24677716277947));
#24147=CARTESIAN_POINT('Ctrl Pts',(167.849048475351,3.23838729348434,1.18265224736778));
#24148=CARTESIAN_POINT('Ctrl Pts',(167.796432803385,3.6270034806906,0.118527331956078));
#24149=CARTESIAN_POINT('Ctrl Pts',(167.743817131419,3.43995030085597,-1.15583082888706));
#24150=CARTESIAN_POINT('Ctrl Pts',(167.691201459453,2.76192559296549,-2.06339177562785));
#24151=CARTESIAN_POINT('Ctrl Pts',(167.638585787487,2.08390088507502,-2.97095272236863));
#24152=CARTESIAN_POINT('Ctrl Pts',(167.585970115521,0.914904649128732,-3.51171645500707));
#24153=CARTESIAN_POINT('Ctrl Pts',(167.533354443555,-0.215740624581454,
-3.44082469528903));
#24154=CARTESIAN_POINT('Ctrl Pts',(167.480738771588,-1.34638589829166,-3.36993293557099));
#24155=CARTESIAN_POINT('Ctrl Pts',(167.428123099622,-2.43868020976575,-2.68738568349645));
#24156=CARTESIAN_POINT('Ctrl Pts',(167.375507427656,-2.99803176537606,-1.7022409155586));
#24157=CARTESIAN_POINT('Ctrl Pts',(167.34811176999,-3.28927205862042,-1.18930080084075));
#24158=CARTESIAN_POINT('Ctrl Pts',(167.320716112323,-3.43603033940618,-0.594325800432333));
#24159=CARTESIAN_POINT('Ctrl Pts',(167.293320454657,-3.4366186727045,0.000377228489918668));
#24160=CARTESIAN_POINT('Ctrl Pts',(167.148679545343,-3.43662347336092,0.000399016594708752));
#24161=CARTESIAN_POINT('Ctrl Pts',(167.176138374695,-3.43599967547967,-0.595673349018475));
#24162=CARTESIAN_POINT('Ctrl Pts',(167.203597204047,-3.28852668101727,-1.19203474800941));
#24163=CARTESIAN_POINT('Ctrl Pts',(167.231056033399,-2.9960028145529,-1.70580971375418));
#24164=CARTESIAN_POINT('Ctrl Pts',(167.283671705365,-2.43547856193824,-2.69028777418379));
#24165=CARTESIAN_POINT('Ctrl Pts',(167.336287377331,-1.34237222830503,-3.3715339141493));
#24166=CARTESIAN_POINT('Ctrl Pts',(167.388903049297,-0.211643291605701,
-3.44107930182745));
#24167=CARTESIAN_POINT('Ctrl Pts',(167.441518721263,0.919085645093658,-3.51062468950561));
#24168=CARTESIAN_POINT('Ctrl Pts',(167.49413439323,2.08743718485917,-2.96846932489641));
#24169=CARTESIAN_POINT('Ctrl Pts',(167.546750065196,2.76438075637838,-2.06010161839459));
#24170=CARTESIAN_POINT('Ctrl Pts',(167.599365737162,3.44132432789757,-1.15173391189279));
#24171=CARTESIAN_POINT('Ctrl Pts',(167.651981409128,3.62685993117048,0.122846136501633));
#24172=CARTESIAN_POINT('Ctrl Pts',(167.704597081094,3.23697688716988,1.18650759638316));
#24173=CARTESIAN_POINT('Ctrl Pts',(167.75721275306,2.84709384316927,2.25016905626472));
#24174=CARTESIAN_POINT('Ctrl Pts',(167.809828425026,1.88179215189513,3.10291192763337));
#24175=CARTESIAN_POINT('Ctrl Pts',(167.862444096993,0.778161240495354,3.35861351276649));
#24176=CARTESIAN_POINT('Ctrl Pts',(167.915059768959,-0.325469670904378,
3.61431509789959));
#24177=CARTESIAN_POINT('Ctrl Pts',(167.967675440925,-1.56742980242973,3.27297539679721));
#24178=CARTESIAN_POINT('Ctrl Pts',(168.020291112891,-2.38535854978838,2.48915331655147));
#24179=CARTESIAN_POINT('Ctrl Pts',(168.063087257042,-3.05063935432642,1.85161393938135));
#24180=CARTESIAN_POINT('Ctrl Pts',(168.105883401192,-3.43539162467462,0.921339312272485));
#24181=CARTESIAN_POINT('Ctrl Pts',(168.148679545343,-3.44364019544098,-0.00287502992418087));
#24182=CARTESIAN_POINT('Origin',(165.,0.,0.));
#24183=CARTESIAN_POINT('',(169.293320454657,-3.44482624767651,0.00255655274150716));
#24184=CARTESIAN_POINT('',(169.148679545343,-3.4448633964524,0.00254358015426723));
#24185=CARTESIAN_POINT('',(165.,-3.442,-4.21523428266519E-16));
#24186=CARTESIAN_POINT('Ctrl Pts',(169.293320454657,-3.44482624767651,0.00255655274150716));
#24187=CARTESIAN_POINT('Ctrl Pts',(169.28543750925,-3.44624129304017,0.172642513390955));
#24188=CARTESIAN_POINT('Ctrl Pts',(169.277554563844,-3.43471905135417,0.342536135345187));
#24189=CARTESIAN_POINT('Ctrl Pts',(169.269671618437,-3.40959196657226,0.510393202924915));
#24190=CARTESIAN_POINT('Ctrl Pts',(169.217055946471,-3.24187820196086,1.63077549019679));
#24191=CARTESIAN_POINT('Ctrl Pts',(169.164440274505,-2.46806100668965,2.66042813182627));
#24192=CARTESIAN_POINT('Ctrl Pts',(169.111824602539,-1.43852546484462,3.13312353540276));
#24193=CARTESIAN_POINT('Ctrl Pts',(169.059208930573,-0.408989922999565,
3.60581893897926));
#24194=CARTESIAN_POINT('Ctrl Pts',(169.006593258607,0.876263965419336,3.52155710450275));
#24195=CARTESIAN_POINT('Ctrl Pts',(168.953977586641,1.83527214599084,2.9184918624124));
#24196=CARTESIAN_POINT('Ctrl Pts',(168.901361914674,2.7942803265623,2.31542662032207));
#24197=CARTESIAN_POINT('Ctrl Pts',(168.848746242708,3.4270427992864,1.19355797061799));
#24198=CARTESIAN_POINT('Ctrl Pts',(168.796130570742,3.44704417820427,0.0608689923961288));
#24199=CARTESIAN_POINT('Ctrl Pts',(168.743514898776,3.46704555712214,-1.07181998582578));
#24200=CARTESIAN_POINT('Ctrl Pts',(168.69089922681,2.87428584223369,-2.21532929256545));
#24201=CARTESIAN_POINT('Ctrl Pts',(168.638283554844,1.93716713675568,-2.85187694073908));
#24202=CARTESIAN_POINT('Ctrl Pts',(168.585667882878,1.0000484312777,-3.4884245889127));
#24203=CARTESIAN_POINT('Ctrl Pts',(168.533052210911,-0.281429264789832,
-3.61801057852031));
#24204=CARTESIAN_POINT('Ctrl Pts',(168.480436538945,-1.32701176028542,-3.181958263219));
#24205=CARTESIAN_POINT('Ctrl Pts',(168.427820866979,-2.37259425578103,-2.74590594791768));
#24206=CARTESIAN_POINT('Ctrl Pts',(168.375205195013,-3.1822815507047,-1.74421532770741));
#24207=CARTESIAN_POINT('Ctrl Pts',(168.322589523047,-3.38944654899261,-0.6304527677149));
#24208=CARTESIAN_POINT('Ctrl Pts',(168.312833166917,-3.42786049345878,-0.42393133078477));
#24209=CARTESIAN_POINT('Ctrl Pts',(168.303076810787,-3.44555785275709,-0.213556512994896));
#24210=CARTESIAN_POINT('Ctrl Pts',(168.293320454657,-3.44367996564435,-0.0028671194461008));
#24211=CARTESIAN_POINT('Ctrl Pts',(168.148679545343,-3.44364019544098,-0.00287502992418087));
#24212=CARTESIAN_POINT('Ctrl Pts',(168.158499073159,-3.44553282085585,-0.214934985809443));
#24213=CARTESIAN_POINT('Ctrl Pts',(168.168318600974,-3.4276037337122,-0.426675887125822));
#24214=CARTESIAN_POINT('Ctrl Pts',(168.178138128789,-3.3886935781589,-0.634488358987591));
#24215=CARTESIAN_POINT('Ctrl Pts',(168.230753800756,-3.18020249597882,-1.74800349489171));
#24216=CARTESIAN_POINT('Ctrl Pts',(168.283369472722,-2.36932296842675,-2.7487293073108));
#24217=CARTESIAN_POINT('Ctrl Pts',(168.335985144688,-1.32322193552417,-3.18353629690223));
#24218=CARTESIAN_POINT('Ctrl Pts',(168.388600816654,-0.2771209026216,-3.61834328649367));
#24219=CARTESIAN_POINT('Ctrl Pts',(168.44121648862,1.00420163563145,-3.48723145325744));
#24220=CARTESIAN_POINT('Ctrl Pts',(168.493832160586,1.94056174368239,-2.84956834683932));
#24221=CARTESIAN_POINT('Ctrl Pts',(168.546447832553,2.87692185173333,-2.21190524042119));
#24222=CARTESIAN_POINT('Ctrl Pts',(168.599063504519,3.46831952958212,-1.06769086082117));
#24223=CARTESIAN_POINT('Ctrl Pts',(168.651679176485,3.44696940550524,0.0649735473051323));
#24224=CARTESIAN_POINT('Ctrl Pts',(168.704294848451,3.42561928142836,1.19763795543145));
#24225=CARTESIAN_POINT('Ctrl Pts',(168.756910520417,2.79152135542575,2.31875239208407));
#24226=CARTESIAN_POINT('Ctrl Pts',(168.809526192383,1.83179570791246,2.92067528643946));
#24227=CARTESIAN_POINT('Ctrl Pts',(168.862141864349,0.872070060399187,3.52259818079485));
#24228=CARTESIAN_POINT('Ctrl Pts',(168.914757536316,-0.413283308624756,
3.60532953285307));
#24229=CARTESIAN_POINT('Ctrl Pts',(168.967373208282,-1.44225529998775,3.13140851599467));
#24230=CARTESIAN_POINT('Ctrl Pts',(169.019988880248,-2.47122729135076,2.65748749913626));
#24231=CARTESIAN_POINT('Ctrl Pts',(169.072604552214,-3.2438179050528,1.62691411336122));
#24232=CARTESIAN_POINT('Ctrl Pts',(169.12522022418,-3.41019745387857,0.50633286465407));
#24233=CARTESIAN_POINT('Ctrl Pts',(169.133039997901,-3.43492488536428,0.339791386166305));
#24234=CARTESIAN_POINT('Ctrl Pts',(169.140859771622,-3.44626227331867,0.171261806054121));
#24235=CARTESIAN_POINT('Ctrl Pts',(169.148679545343,-3.4448633964524,0.00254358015426723));
#24236=CARTESIAN_POINT('Origin',(165.,0.,0.));
#24237=CARTESIAN_POINT('',(170.293320454657,-3.43660005727478,0.000272750764409579));
#24238=CARTESIAN_POINT('',(170.148679545343,-3.43660359651311,0.000294614659134998));
#24239=CARTESIAN_POINT('',(165.,-3.442,-4.21523428266519E-16));
#24240=CARTESIAN_POINT('Ctrl Pts',(170.293320454657,-3.43660005727478,0.000272750764409579));
#24241=CARTESIAN_POINT('Ctrl Pts',(170.267798207714,-3.43699621854537,0.554315412873624));
#24242=CARTESIAN_POINT('Ctrl Pts',(170.242275960771,-3.31054519341703,1.10818746561827));
#24243=CARTESIAN_POINT('Ctrl Pts',(170.216753713828,-3.05626134594043,1.59533229623574));
#24244=CARTESIAN_POINT('Ctrl Pts',(170.164138041862,-2.53203965280226,2.59961113834073));
#24245=CARTESIAN_POINT('Ctrl Pts',(170.111522369896,-1.46452408676501,3.32029700118331));
#24246=CARTESIAN_POINT('Ctrl Pts',(170.05890669793,-0.337086580959713,3.43106270007475));
#24247=CARTESIAN_POINT('Ctrl Pts',(170.006291025963,0.790350924845598,3.54182839896619));
#24248=CARTESIAN_POINT('Ctrl Pts',(169.953675353997,1.97771037041895,3.04267393390648));
#24249=CARTESIAN_POINT('Ctrl Pts',(169.901059682031,2.68735437690533,2.15961687771555));
#24250=CARTESIAN_POINT('Ctrl Pts',(169.848444010065,3.39699838339171,1.27655982152463));
#24251=CARTESIAN_POINT('Ctrl Pts',(169.795828338099,3.62892695079112,0.00960017420250078));
#24252=CARTESIAN_POINT('Ctrl Pts',(169.743212666133,3.27812263219616,-1.06758166106696));
#24253=CARTESIAN_POINT('Ctrl Pts',(169.690596994167,2.9273183136012,-2.14476349633643));
#24254=CARTESIAN_POINT('Ctrl Pts',(169.6379813222,1.99378110901184,-3.03216751955324));
#24255=CARTESIAN_POINT('Ctrl Pts',(169.585365650234,0.900217456132267,-3.32797643239589));
#24256=CARTESIAN_POINT('Ctrl Pts',(169.532749978268,-0.19334619674729,-3.62378534523853));
#24257=CARTESIAN_POINT('Ctrl Pts',(169.480134306302,-1.44693629791706,-3.32799914770704));
#24258=CARTESIAN_POINT('Ctrl Pts',(169.427518634336,-2.29292618152615,-2.57455008248416));
#24259=CARTESIAN_POINT('Ctrl Pts',(169.382785907776,-3.01216880870502,-1.93398369319767));
#24260=CARTESIAN_POINT('Ctrl Pts',(169.338053181217,-3.43679640171692,-0.962616790092074));
#24261=CARTESIAN_POINT('Ctrl Pts',(169.293320454657,-3.44482624767651,0.00255655274150716));
#24262=CARTESIAN_POINT('Ctrl Pts',(169.148679545343,-3.4448633964524,0.00254358015426723));
#24263=CARTESIAN_POINT('Ctrl Pts',(169.193475443588,-3.43684987227702,-0.963965777940212));
#24264=CARTESIAN_POINT('Ctrl Pts',(169.238271341833,-3.01088069160431,-1.93666577160495));
#24265=CARTESIAN_POINT('Ctrl Pts',(169.283067240079,-2.28985899035532,-2.57727869052755));
#24266=CARTESIAN_POINT('Ctrl Pts',(169.335682912045,-1.44297249405678,-3.32971988536281));
#24267=CARTESIAN_POINT('Ctrl Pts',(169.388298584011,-0.189031017510179,
-3.62401316339407));
#24268=CARTESIAN_POINT('Ctrl Pts',(169.440914255977,0.904179671619464,-3.32690227780616));
#24269=CARTESIAN_POINT('Ctrl Pts',(169.493529927943,1.99739036074909,-3.02979139221826));
#24270=CARTESIAN_POINT('Ctrl Pts',(169.546145599909,2.92987026246178,-2.1412763430112));
#24271=CARTESIAN_POINT('Ctrl Pts',(169.598761271875,3.2793916841586,-1.0636775007116));
#24272=CARTESIAN_POINT('Ctrl Pts',(169.651376943842,3.62891310585543,0.0139213415880397));
#24273=CARTESIAN_POINT('Ctrl Pts',(169.703992615808,3.39547604753637,1.28060397698021));
#24274=CARTESIAN_POINT('Ctrl Pts',(169.756608287774,2.68478100720705,2.16281543087444));
#24275=CARTESIAN_POINT('Ctrl Pts',(169.80922395974,1.97408596687775,3.04502688476864));
#24276=CARTESIAN_POINT('Ctrl Pts',(169.861839631706,0.786132944538199,3.5427671571649));
#24277=CARTESIAN_POINT('Ctrl Pts',(169.914455303672,-0.341171919250267,
3.43065902822761));
#24278=CARTESIAN_POINT('Ctrl Pts',(169.967070975638,-1.46847678303873,3.31855089929033));
#24279=CARTESIAN_POINT('Ctrl Pts',(170.019686647605,-2.53513348827613,2.59659436901949));
#24280=CARTESIAN_POINT('Ctrl Pts',(170.072302319571,-3.05815897380138,1.59169197060008));
#24281=CARTESIAN_POINT('Ctrl Pts',(170.097761394828,-3.31123462027619,1.10545118279472));
#24282=CARTESIAN_POINT('Ctrl Pts',(170.123220470086,-3.43703049239502,0.552964592785464));
#24283=CARTESIAN_POINT('Ctrl Pts',(170.148679545343,-3.43660359651311,0.000294614659134998));
#24284=CARTESIAN_POINT('Origin',(165.,0.,0.));
#24285=CARTESIAN_POINT('',(171.293320454657,-3.44387122878711,-0.00282630271176032));
#24286=CARTESIAN_POINT('',(171.148679545343,-3.44383074993744,-0.0028355498312654));
#24287=CARTESIAN_POINT('',(165.,-3.442,-4.21523428266519E-16));
#24288=CARTESIAN_POINT('Ctrl Pts',(171.293320454657,-3.44387122878711,-0.00282630271176032));
#24289=CARTESIAN_POINT('Ctrl Pts',(171.250158906178,-3.43562450198846,0.929118171345689));
#24290=CARTESIAN_POINT('Ctrl Pts',(171.206997357698,-3.04353120649987,1.86717743073024));
#24291=CARTESIAN_POINT('Ctrl Pts',(171.163835809219,-2.36815699607087,2.50552345035264));
#24292=CARTESIAN_POINT('Ctrl Pts',(171.111220137253,-1.5448485383751,3.28369304696447));
#24293=CARTESIAN_POINT('Ctrl Pts',(171.058604465286,-0.300567776468357,
3.61647092641191));
#24294=CARTESIAN_POINT('Ctrl Pts',(171.00598879332,0.801275500324471,3.35317411112243));
#24295=CARTESIAN_POINT('Ctrl Pts',(170.953373121354,1.90311877711725,3.08987729583295));
#24296=CARTESIAN_POINT('Ctrl Pts',(170.900757449388,2.86252456879606,2.23050578580653));
#24297=CARTESIAN_POINT('Ctrl Pts',(170.848141777422,3.24507232555683,1.1641841628401));
#24298=CARTESIAN_POINT('Ctrl Pts',(170.795526105456,3.62762008231762,0.0978625398736385));
#24299=CARTESIAN_POINT('Ctrl Pts',(170.74291043349,3.43330980416037,-1.17540919603287));
#24300=CARTESIAN_POINT('Ctrl Pts',(170.690294761523,2.7501257418227,-2.07909273270173));
#24301=CARTESIAN_POINT('Ctrl Pts',(170.637679089557,2.06694167948504,-2.98277626937059));
#24302=CARTESIAN_POINT('Ctrl Pts',(170.585063417591,0.894883832966949,-3.5168716068018));
#24303=CARTESIAN_POINT('Ctrl Pts',(170.532447745625,-0.235339201293036,
-3.4395398162459));
#24304=CARTESIAN_POINT('Ctrl Pts',(170.479832073659,-1.365562235553,-3.36220802569001));
#24305=CARTESIAN_POINT('Ctrl Pts',(170.427216401693,-2.45395045755487,-2.67344910714704));
#24306=CARTESIAN_POINT('Ctrl Pts',(170.374600729727,-3.00768065843627,-1.68513373719186));
#24307=CARTESIAN_POINT('Ctrl Pts',(170.347507304703,-3.29281334077317,-1.17621980766165));
#24308=CARTESIAN_POINT('Ctrl Pts',(170.32041387968,-3.43617950787308,-0.587877397577702));
#24309=CARTESIAN_POINT('Ctrl Pts',(170.293320454657,-3.43660005727478,0.000272750764409579));
#24310=CARTESIAN_POINT('Ctrl Pts',(170.148679545343,-3.43660359651311,0.000294614659134998));
#24311=CARTESIAN_POINT('Ctrl Pts',(170.175836142052,-3.43614823671766,-0.589225450670685));
#24312=CARTESIAN_POINT('Ctrl Pts',(170.20299273876,-3.29207677469171,-1.178954174763));
#24313=CARTESIAN_POINT('Ctrl Pts',(170.230149335469,-3.00567206006267,-1.68871404224666));
#24314=CARTESIAN_POINT('Ctrl Pts',(170.282765007435,-2.45076539498559,-2.67636939010597));
#24315=CARTESIAN_POINT('Ctrl Pts',(170.335380679402,-1.36155779901833,-3.36383181925656));
#24316=CARTESIAN_POINT('Ctrl Pts',(170.387996351368,-0.231243408789148,
-3.43981774870589));
#24317=CARTESIAN_POINT('Ctrl Pts',(170.440612023334,0.899070981439999,-3.51580367815521));
#24318=CARTESIAN_POINT('Ctrl Pts',(170.4932276953,2.07049216593107,-2.98031310790332));
#24319=CARTESIAN_POINT('Ctrl Pts',(170.545843367266,2.7525996566615,-2.07581664023284));
#24320=CARTESIAN_POINT('Ctrl Pts',(170.598459039232,3.43470714739194,-1.17132017256236));
#24321=CARTESIAN_POINT('Ctrl Pts',(170.651074711198,3.62750094436174,0.102182192526675));
#24322=CARTESIAN_POINT('Ctrl Pts',(170.703690383164,3.2436838097568,1.16804753377652));
#24323=CARTESIAN_POINT('Ctrl Pts',(170.756306055131,2.85986667515186,2.23391287502634));
#24324=CARTESIAN_POINT('Ctrl Pts',(170.808921727097,1.89943860897218,3.09214119243696));
#24325=CARTESIAN_POINT('Ctrl Pts',(170.861537399063,0.797282342672176,3.35412590649805));
#24326=CARTESIAN_POINT('Ctrl Pts',(170.914153071029,-0.304873923627829,
3.61611062055913));
#24327=CARTESIAN_POINT('Ctrl Pts',(170.966768742995,-1.54875839004818,3.28185173127071));
#24328=CARTESIAN_POINT('Ctrl Pts',(171.019384414962,-2.37113928540063,2.50270208381497));
#24329=CARTESIAN_POINT('Ctrl Pts',(171.062482791755,-3.04476522937394,1.86448757794553));
#24330=CARTESIAN_POINT('Ctrl Pts',(171.105581168549,-3.43558242261714,0.927772636575842));
#24331=CARTESIAN_POINT('Ctrl Pts',(171.148679545343,-3.44383074993744,-0.0028355498312654));
#24332=CARTESIAN_POINT('Origin',(165.,0.,0.));
#24333=CARTESIAN_POINT('',(172.293320454657,-3.44466766225695,0.00262740410212479));
#24334=CARTESIAN_POINT('',(172.148679545343,-3.44468745739532,0.00260595186748766));
#24335=CARTESIAN_POINT('',(165.,-3.442,-4.21523428266519E-16));
#24336=CARTESIAN_POINT('Ctrl Pts',(172.293320454657,-3.44466766225695,0.00262740410212479));
#24337=CARTESIAN_POINT('Ctrl Pts',(172.285135276607,-3.44617626541761,0.179267317335753));
#24338=CARTESIAN_POINT('Ctrl Pts',(172.276950098558,-3.43376273876756,0.355695505307162));
#24339=CARTESIAN_POINT('Ctrl Pts',(172.268764920508,-3.40668944351872,0.52984202940742));
#24340=CARTESIAN_POINT('Ctrl Pts',(172.216149248542,-3.2326578447912,1.64928455472401));
#24341=CARTESIAN_POINT('Ctrl Pts',(172.163533576576,-2.4528655438326,2.67444576178309));
#24342=CARTESIAN_POINT('Ctrl Pts',(172.110917904609,-1.4206230354588,3.14125155492291));
#24343=CARTESIAN_POINT('Ctrl Pts',(172.058302232643,-0.388380527085031,
3.60805734806272));
#24344=CARTESIAN_POINT('Ctrl Pts',(172.005686560677,0.89631218870392,3.51650772728329));
#24345=CARTESIAN_POINT('Ctrl Pts',(171.953070888711,1.85185396723248,2.90799717118038));
#24346=CARTESIAN_POINT('Ctrl Pts',(171.900455216745,2.80739574576104,2.29948661507748));
#24347=CARTESIAN_POINT('Ctrl Pts',(171.847839544779,3.43378658702921,1.17401512365106));
#24348=CARTESIAN_POINT('Ctrl Pts',(171.795223872812,3.44734233714038,0.0412264759991943));
#24349=CARTESIAN_POINT('Ctrl Pts',(171.742608200846,3.46089808725154,-1.09156217165267));
#24350=CARTESIAN_POINT('Ctrl Pts',(171.68999252888,2.86161874620574,-2.23166797553003));
#24351=CARTESIAN_POINT('Ctrl Pts',(171.637376856914,1.92088515794683,-2.86286457252168));
#24352=CARTESIAN_POINT('Ctrl Pts',(171.584761184948,0.980151569687923,-3.49406116951333));
#24353=CARTESIAN_POINT('Ctrl Pts',(171.532145512982,-0.302036265784079,
-3.61634855961926));
#24354=CARTESIAN_POINT('Ctrl Pts',(171.479529841016,-1.34511579343341,-3.1743477253533));
#24355=CARTESIAN_POINT('Ctrl Pts',(171.426914169049,-2.38819532108274,-2.73234689108733));
#24356=CARTESIAN_POINT('Ctrl Pts',(171.374298497083,-3.19216654090938,-1.72605783244947));
#24357=CARTESIAN_POINT('Ctrl Pts',(171.321682825117,-3.39298407408037,-0.611132646242449));
#24358=CARTESIAN_POINT('Ctrl Pts',(171.31222870163,-3.42906750105106,-0.41079993176759));
#24359=CARTESIAN_POINT('Ctrl Pts',(171.302774578144,-3.44567759524667,-0.206959806975336));
#24360=CARTESIAN_POINT('Ctrl Pts',(171.293320454657,-3.44387122878711,-0.00282630271176032));
#24361=CARTESIAN_POINT('Ctrl Pts',(171.148679545343,-3.44383074993744,-0.0028355498312654));
#24362=CARTESIAN_POINT('Ctrl Pts',(171.158196840515,-3.44565220521313,-0.208339178010312));
#24363=CARTESIAN_POINT('Ctrl Pts',(171.167714135688,-3.4288178176788,-0.413545012325797));
#24364=CARTESIAN_POINT('Ctrl Pts',(171.17723143086,-3.3922533139467,-0.615172870133585));
#24365=CARTESIAN_POINT('Ctrl Pts',(171.229847102826,-3.19010912285572,-1.72985777100326));
#24366=CARTESIAN_POINT('Ctrl Pts',(171.282462774792,-2.38494341638922,-2.73518716711955));
#24367=CARTESIAN_POINT('Ctrl Pts',(171.335078446758,-1.34133662038965,-3.17594649833862));
#24368=CARTESIAN_POINT('Ctrl Pts',(171.387694118724,-0.297729824390071,
-3.61670582955769));
#24369=CARTESIAN_POINT('Ctrl Pts',(171.440309790691,0.984318061142581,-3.49289509587954));
#24370=CARTESIAN_POINT('Ctrl Pts',(171.492925462657,1.92429609530075,-2.86057702277709));
#24371=CARTESIAN_POINT('Ctrl Pts',(171.545541134623,2.86427412945893,-2.22825894967464));
#24372=CARTESIAN_POINT('Ctrl Pts',(171.598156806589,3.46218231224263,-1.08743353714789));
#24373=CARTESIAN_POINT('Ctrl Pts',(171.650772478555,3.44728441488538,0.0453347604952326));
#24374=CARTESIAN_POINT('Ctrl Pts',(171.703388150521,3.43238651752813,1.17810305813836));
#24375=CARTESIAN_POINT('Ctrl Pts',(171.756003822488,2.80468254002992,2.30281424089786));
#24376=CARTESIAN_POINT('Ctrl Pts',(171.808619494454,1.84840322753821,2.91019355475018));
#24377=CARTESIAN_POINT('Ctrl Pts',(171.86123516642,0.892123915046473,3.51757286860253));
#24378=CARTESIAN_POINT('Ctrl Pts',(171.913850838386,-0.392730732438793,
3.60762031354766));
#24379=CARTESIAN_POINT('Ctrl Pts',(171.966466510352,-1.42438925928684,3.13957157218144));
#24380=CARTESIAN_POINT('Ctrl Pts',(172.019082182318,-2.45604778613486,2.67152283081523));
#24381=CARTESIAN_POINT('Ctrl Pts',(172.071697854284,-3.23451019234567,1.6453779031377));
#24382=CARTESIAN_POINT('Ctrl Pts',(172.124313526251,-3.40726414772573,0.525757408362557));
#24383=CARTESIAN_POINT('Ctrl Pts',(172.132435532615,-3.4339312731772,0.352927442608599));
#24384=CARTESIAN_POINT('Ctrl Pts',(172.140557538979,-3.44616528464549,0.177870095822215));
#24385=CARTESIAN_POINT('Ctrl Pts',(172.148679545343,-3.44468745739532,0.00260595186748766));
#24386=CARTESIAN_POINT('Ctrl Pts',(37.5,32.4,0.));
#24387=CARTESIAN_POINT('Ctrl Pts',(37.5,32.4,32.4));
#24388=CARTESIAN_POINT('Ctrl Pts',(37.5,0.,32.4));
#24389=CARTESIAN_POINT('Ctrl Pts',(37.5,-32.4,32.4));
#24390=CARTESIAN_POINT('Ctrl Pts',(37.5,-32.4,0.));
#24391=CARTESIAN_POINT('Ctrl Pts',(37.5,-32.4,-32.4));
#24392=CARTESIAN_POINT('Ctrl Pts',(37.5,0.,-32.4));
#24393=CARTESIAN_POINT('Ctrl Pts',(37.5,32.4,-32.4));
#24394=CARTESIAN_POINT('Ctrl Pts',(37.5,32.4,0.));
#24395=CARTESIAN_POINT('Ctrl Pts',(37.3389083940589,32.2580145365138,0.));
#24396=CARTESIAN_POINT('Ctrl Pts',(37.3389083940589,32.2580145365137,32.2580145365137));
#24397=CARTESIAN_POINT('Ctrl Pts',(37.3389083940589,0.,32.2580145365138));
#24398=CARTESIAN_POINT('Ctrl Pts',(37.3389083940589,-32.2580145365137,32.2580145365137));
#24399=CARTESIAN_POINT('Ctrl Pts',(37.3389083940589,-32.2580145365138,0.));
#24400=CARTESIAN_POINT('Ctrl Pts',(37.3389083940589,-32.2580145365137,-32.2580145365137));
#24401=CARTESIAN_POINT('Ctrl Pts',(37.3389083940589,0.,-32.2580145365138));
#24402=CARTESIAN_POINT('Ctrl Pts',(37.3389083940589,32.2580145365137,-32.2580145365137));
#24403=CARTESIAN_POINT('Ctrl Pts',(37.3389083940589,32.2580145365138,0.));
#24404=CARTESIAN_POINT('Ctrl Pts',(37.0144855040189,31.9658168899962,0.));
#24405=CARTESIAN_POINT('Ctrl Pts',(37.0144855040189,31.9658168899962,31.9658168899962));
#24406=CARTESIAN_POINT('Ctrl Pts',(37.0144855040189,0.,31.9658168899962));
#24407=CARTESIAN_POINT('Ctrl Pts',(37.0144855040189,-31.9658168899962,31.9658168899962));
#24408=CARTESIAN_POINT('Ctrl Pts',(37.0144855040189,-31.9658168899962,0.));
#24409=CARTESIAN_POINT('Ctrl Pts',(37.0144855040189,-31.9658168899962,-31.9658168899962));
#24410=CARTESIAN_POINT('Ctrl Pts',(37.0144855040189,0.,-31.9658168899962));
#24411=CARTESIAN_POINT('Ctrl Pts',(37.0144855040189,31.9658168899962,-31.9658168899962));
#24412=CARTESIAN_POINT('Ctrl Pts',(37.0144855040189,31.9658168899962,0.));
#24413=CARTESIAN_POINT('Ctrl Pts',(36.5211322358012,31.5028400616267,0.));
#24414=CARTESIAN_POINT('Ctrl Pts',(36.5211322358012,31.5028400616266,31.5028400616266));
#24415=CARTESIAN_POINT('Ctrl Pts',(36.5211322358012,0.,31.5028400616267));
#24416=CARTESIAN_POINT('Ctrl Pts',(36.5211322358012,-31.5028400616266,31.5028400616266));
#24417=CARTESIAN_POINT('Ctrl Pts',(36.5211322358012,-31.5028400616267,0.));
#24418=CARTESIAN_POINT('Ctrl Pts',(36.5211322358012,-31.5028400616266,-31.5028400616266));
#24419=CARTESIAN_POINT('Ctrl Pts',(36.5211322358012,0.,-31.5028400616267));
#24420=CARTESIAN_POINT('Ctrl Pts',(36.5211322358012,31.5028400616266,-31.5028400616266));
#24421=CARTESIAN_POINT('Ctrl Pts',(36.5211322358012,31.5028400616267,0.));
#24422=CARTESIAN_POINT('Ctrl Pts',(35.849854090057,30.8360498427659,0.));
#24423=CARTESIAN_POINT('Ctrl Pts',(35.849854090057,30.8360498427659,30.8360498427659));
#24424=CARTESIAN_POINT('Ctrl Pts',(35.849854090057,0.,30.8360498427659));
#24425=CARTESIAN_POINT('Ctrl Pts',(35.849854090057,-30.8360498427659,30.8360498427659));
#24426=CARTESIAN_POINT('Ctrl Pts',(35.849854090057,-30.8360498427659,0.));
#24427=CARTESIAN_POINT('Ctrl Pts',(35.849854090057,-30.8360498427659,-30.8360498427659));
#24428=CARTESIAN_POINT('Ctrl Pts',(35.849854090057,0.,-30.8360498427659));
#24429=CARTESIAN_POINT('Ctrl Pts',(35.849854090057,30.8360498427659,-30.8360498427659));
#24430=CARTESIAN_POINT('Ctrl Pts',(35.849854090057,30.8360498427659,0.));
#24431=CARTESIAN_POINT('Ctrl Pts',(34.987601126175,29.9204750609072,0.));
#24432=CARTESIAN_POINT('Ctrl Pts',(34.987601126175,29.9204750609072,29.9204750609072));
#24433=CARTESIAN_POINT('Ctrl Pts',(34.987601126175,0.,29.9204750609072));
#24434=CARTESIAN_POINT('Ctrl Pts',(34.987601126175,-29.9204750609072,29.9204750609072));
#24435=CARTESIAN_POINT('Ctrl Pts',(34.987601126175,-29.9204750609072,0.));
#24436=CARTESIAN_POINT('Ctrl Pts',(34.987601126175,-29.9204750609072,-29.9204750609072));
#24437=CARTESIAN_POINT('Ctrl Pts',(34.987601126175,0.,-29.9204750609072));
#24438=CARTESIAN_POINT('Ctrl Pts',(34.987601126175,29.9204750609072,-29.9204750609072));
#24439=CARTESIAN_POINT('Ctrl Pts',(34.987601126175,29.9204750609072,0.));
#24440=CARTESIAN_POINT('Ctrl Pts',(34.1004337719427,28.9253475198501,0.));
#24441=CARTESIAN_POINT('Ctrl Pts',(34.1004337719427,28.9253475198501,28.9253475198501));
#24442=CARTESIAN_POINT('Ctrl Pts',(34.1004337719427,0.,28.9253475198501));
#24443=CARTESIAN_POINT('Ctrl Pts',(34.1004337719427,-28.9253475198501,28.9253475198501));
#24444=CARTESIAN_POINT('Ctrl Pts',(34.1004337719427,-28.9253475198501,0.));
#24445=CARTESIAN_POINT('Ctrl Pts',(34.1004337719427,-28.9253475198501,-28.9253475198501));
#24446=CARTESIAN_POINT('Ctrl Pts',(34.1004337719427,0.,-28.9253475198501));
#24447=CARTESIAN_POINT('Ctrl Pts',(34.1004337719427,28.9253475198501,-28.9253475198501));
#24448=CARTESIAN_POINT('Ctrl Pts',(34.1004337719427,28.9253475198501,0.));
#24449=CARTESIAN_POINT('Ctrl Pts',(33.1851263782876,27.8567138854442,0.));
#24450=CARTESIAN_POINT('Ctrl Pts',(33.1851263782876,27.8567138854442,27.8567138854442));
#24451=CARTESIAN_POINT('Ctrl Pts',(33.1851263782876,0.,27.8567138854442));
#24452=CARTESIAN_POINT('Ctrl Pts',(33.1851263782876,-27.8567138854442,27.8567138854442));
#24453=CARTESIAN_POINT('Ctrl Pts',(33.1851263782876,-27.8567138854442,0.));
#24454=CARTESIAN_POINT('Ctrl Pts',(33.1851263782876,-27.8567138854442,-27.8567138854442));
#24455=CARTESIAN_POINT('Ctrl Pts',(33.1851263782876,0.,-27.8567138854442));
#24456=CARTESIAN_POINT('Ctrl Pts',(33.1851263782876,27.8567138854442,-27.8567138854442));
#24457=CARTESIAN_POINT('Ctrl Pts',(33.1851263782876,27.8567138854442,0.));
#24458=CARTESIAN_POINT('Ctrl Pts',(32.2364640041498,26.7258152226803,0.));
#24459=CARTESIAN_POINT('Ctrl Pts',(32.2364640041498,26.7258152226803,26.7258152226803));
#24460=CARTESIAN_POINT('Ctrl Pts',(32.2364640041498,0.,26.7258152226803));
#24461=CARTESIAN_POINT('Ctrl Pts',(32.2364640041498,-26.7258152226803,26.7258152226803));
#24462=CARTESIAN_POINT('Ctrl Pts',(32.2364640041498,-26.7258152226803,0.));
#24463=CARTESIAN_POINT('Ctrl Pts',(32.2364640041498,-26.7258152226803,-26.7258152226803));
#24464=CARTESIAN_POINT('Ctrl Pts',(32.2364640041498,0.,-26.7258152226803));
#24465=CARTESIAN_POINT('Ctrl Pts',(32.2364640041498,26.7258152226803,-26.7258152226803));
#24466=CARTESIAN_POINT('Ctrl Pts',(32.2364640041498,26.7258152226803,0.));
#24467=CARTESIAN_POINT('Ctrl Pts',(31.2480536381088,25.5477500100038,0.));
#24468=CARTESIAN_POINT('Ctrl Pts',(31.2480536381088,25.5477500100038,25.5477500100038));
#24469=CARTESIAN_POINT('Ctrl Pts',(31.2480536381088,0.,25.5477500100038));
#24470=CARTESIAN_POINT('Ctrl Pts',(31.2480536381087,-25.5477500100038,25.5477500100038));
#24471=CARTESIAN_POINT('Ctrl Pts',(31.2480536381087,-25.5477500100038,0.));
#24472=CARTESIAN_POINT('Ctrl Pts',(31.2480536381087,-25.5477500100038,-25.5477500100038));
#24473=CARTESIAN_POINT('Ctrl Pts',(31.2480536381088,0.,-25.5477500100038));
#24474=CARTESIAN_POINT('Ctrl Pts',(31.2480536381088,25.5477500100038,-25.5477500100038));
#24475=CARTESIAN_POINT('Ctrl Pts',(31.2480536381088,25.5477500100038,0.));
#24476=CARTESIAN_POINT('Ctrl Pts',(30.2132710279087,24.339870673897,0.));
#24477=CARTESIAN_POINT('Ctrl Pts',(30.2132710279087,24.339870673897,24.339870673897));
#24478=CARTESIAN_POINT('Ctrl Pts',(30.2132710279087,0.,24.339870673897));
#24479=CARTESIAN_POINT('Ctrl Pts',(30.2132710279087,-24.339870673897,24.339870673897));
#24480=CARTESIAN_POINT('Ctrl Pts',(30.2132710279087,-24.339870673897,0.));
#24481=CARTESIAN_POINT('Ctrl Pts',(30.2132710279087,-24.339870673897,-24.339870673897));
#24482=CARTESIAN_POINT('Ctrl Pts',(30.2132710279087,0.,-24.339870673897));
#24483=CARTESIAN_POINT('Ctrl Pts',(30.2132710279087,24.339870673897,-24.339870673897));
#24484=CARTESIAN_POINT('Ctrl Pts',(30.2132710279087,24.339870673897,0.));
#24485=CARTESIAN_POINT('Ctrl Pts',(29.1261855002599,23.1203063432132,0.));
#24486=CARTESIAN_POINT('Ctrl Pts',(29.1261855002599,23.1203063432132,23.1203063432132));
#24487=CARTESIAN_POINT('Ctrl Pts',(29.1261855002599,0.,23.1203063432132));
#24488=CARTESIAN_POINT('Ctrl Pts',(29.1261855002599,-23.1203063432132,23.1203063432132));
#24489=CARTESIAN_POINT('Ctrl Pts',(29.1261855002599,-23.1203063432132,0.));
#24490=CARTESIAN_POINT('Ctrl Pts',(29.1261855002599,-23.1203063432132,-23.1203063432132));
#24491=CARTESIAN_POINT('Ctrl Pts',(29.1261855002599,0.,-23.1203063432132));
#24492=CARTESIAN_POINT('Ctrl Pts',(29.1261855002599,23.1203063432132,-23.1203063432132));
#24493=CARTESIAN_POINT('Ctrl Pts',(29.1261855002599,23.1203063432132,0.));
#24494=CARTESIAN_POINT('Ctrl Pts',(27.9824847998069,21.9065059385018,0.));
#24495=CARTESIAN_POINT('Ctrl Pts',(27.9824847998069,21.9065059385018,21.9065059385018));
#24496=CARTESIAN_POINT('Ctrl Pts',(27.9824847998069,0.,21.9065059385018));
#24497=CARTESIAN_POINT('Ctrl Pts',(27.9824847998069,-21.9065059385018,21.9065059385018));
#24498=CARTESIAN_POINT('Ctrl Pts',(27.9824847998069,-21.9065059385018,0.));
#24499=CARTESIAN_POINT('Ctrl Pts',(27.9824847998069,-21.9065059385018,-21.9065059385018));
#24500=CARTESIAN_POINT('Ctrl Pts',(27.9824847998069,0.,-21.9065059385018));
#24501=CARTESIAN_POINT('Ctrl Pts',(27.9824847998069,21.9065059385018,-21.9065059385018));
#24502=CARTESIAN_POINT('Ctrl Pts',(27.9824847998069,21.9065059385018,0.));
#24503=CARTESIAN_POINT('Ctrl Pts',(26.780529153894,20.7136594976185,0.));
#24504=CARTESIAN_POINT('Ctrl Pts',(26.780529153894,20.7136594976185,20.7136594976185));
#24505=CARTESIAN_POINT('Ctrl Pts',(26.780529153894,0.,20.7136594976185));
#24506=CARTESIAN_POINT('Ctrl Pts',(26.780529153894,-20.7136594976185,20.7136594976185));
#24507=CARTESIAN_POINT('Ctrl Pts',(26.780529153894,-20.7136594976185,0.));
#24508=CARTESIAN_POINT('Ctrl Pts',(26.780529153894,-20.7136594976185,-20.7136594976185));
#24509=CARTESIAN_POINT('Ctrl Pts',(26.780529153894,0.,-20.7136594976185));
#24510=CARTESIAN_POINT('Ctrl Pts',(26.780529153894,20.7136594976185,-20.7136594976185));
#24511=CARTESIAN_POINT('Ctrl Pts',(26.780529153894,20.7136594976185,0.));
#24512=CARTESIAN_POINT('Ctrl Pts',(25.5210824112439,19.5548484421686,0.));
#24513=CARTESIAN_POINT('Ctrl Pts',(25.5210824112439,19.5548484421686,19.5548484421686));
#24514=CARTESIAN_POINT('Ctrl Pts',(25.5210824112439,0.,19.5548484421686));
#24515=CARTESIAN_POINT('Ctrl Pts',(25.5210824112439,-19.5548484421686,19.5548484421686));
#24516=CARTESIAN_POINT('Ctrl Pts',(25.5210824112439,-19.5548484421686,0.));
#24517=CARTESIAN_POINT('Ctrl Pts',(25.5210824112439,-19.5548484421686,-19.5548484421686));
#24518=CARTESIAN_POINT('Ctrl Pts',(25.5210824112439,0.,-19.5548484421686));
#24519=CARTESIAN_POINT('Ctrl Pts',(25.5210824112439,19.5548484421686,-19.5548484421686));
#24520=CARTESIAN_POINT('Ctrl Pts',(25.5210824112439,19.5548484421686,0.));
#24521=CARTESIAN_POINT('Ctrl Pts',(24.2069345847179,18.4413554671298,0.));
#24522=CARTESIAN_POINT('Ctrl Pts',(24.2069345847179,18.4413554671298,18.4413554671298));
#24523=CARTESIAN_POINT('Ctrl Pts',(24.2069345847179,0.,18.4413554671298));
#24524=CARTESIAN_POINT('Ctrl Pts',(24.2069345847179,-18.4413554671298,18.4413554671298));
#24525=CARTESIAN_POINT('Ctrl Pts',(24.2069345847179,-18.4413554671298,0.));
#24526=CARTESIAN_POINT('Ctrl Pts',(24.2069345847179,-18.4413554671298,-18.4413554671298));
#24527=CARTESIAN_POINT('Ctrl Pts',(24.2069345847179,0.,-18.4413554671298));
#24528=CARTESIAN_POINT('Ctrl Pts',(24.2069345847179,18.4413554671298,-18.4413554671298));
#24529=CARTESIAN_POINT('Ctrl Pts',(24.2069345847179,18.4413554671298,0.));
#24530=CARTESIAN_POINT('Ctrl Pts',(22.8426190791586,17.3828861014748,0.));
#24531=CARTESIAN_POINT('Ctrl Pts',(22.8426190791586,17.3828861014748,17.3828861014748));
#24532=CARTESIAN_POINT('Ctrl Pts',(22.8426190791586,0.,17.3828861014748));
#24533=CARTESIAN_POINT('Ctrl Pts',(22.8426190791586,-17.3828861014748,17.3828861014748));
#24534=CARTESIAN_POINT('Ctrl Pts',(22.8426190791586,-17.3828861014748,0.));
#24535=CARTESIAN_POINT('Ctrl Pts',(22.8426190791586,-17.3828861014748,-17.3828861014748));
#24536=CARTESIAN_POINT('Ctrl Pts',(22.8426190791586,0.,-17.3828861014748));
#24537=CARTESIAN_POINT('Ctrl Pts',(22.8426190791586,17.3828861014748,-17.3828861014748));
#24538=CARTESIAN_POINT('Ctrl Pts',(22.8426190791586,17.3828861014748,0.));
#24539=CARTESIAN_POINT('Ctrl Pts',(21.4341168715413,16.3877853586665,0.));
#24540=CARTESIAN_POINT('Ctrl Pts',(21.4341168715413,16.3877853586665,16.3877853586665));
#24541=CARTESIAN_POINT('Ctrl Pts',(21.4341168715413,0.,16.3877853586665));
#24542=CARTESIAN_POINT('Ctrl Pts',(21.4341168715413,-16.3877853586665,16.3877853586665));
#24543=CARTESIAN_POINT('Ctrl Pts',(21.4341168715413,-16.3877853586665,0.));
#24544=CARTESIAN_POINT('Ctrl Pts',(21.4341168715413,-16.3877853586665,-16.3877853586665));
#24545=CARTESIAN_POINT('Ctrl Pts',(21.4341168715413,0.,-16.3877853586665));
#24546=CARTESIAN_POINT('Ctrl Pts',(21.4341168715413,16.3877853586665,-16.3877853586665));
#24547=CARTESIAN_POINT('Ctrl Pts',(21.4341168715413,16.3877853586665,0.));
#24548=CARTESIAN_POINT('Ctrl Pts',(19.9886520715334,15.4632288398589,0.));
#24549=CARTESIAN_POINT('Ctrl Pts',(19.9886520715334,15.4632288398589,15.4632288398589));
#24550=CARTESIAN_POINT('Ctrl Pts',(19.9886520715334,0.,15.4632288398589));
#24551=CARTESIAN_POINT('Ctrl Pts',(19.9886520715334,-15.4632288398589,15.4632288398589));
#24552=CARTESIAN_POINT('Ctrl Pts',(19.9886520715334,-15.4632288398589,0.));
#24553=CARTESIAN_POINT('Ctrl Pts',(19.9886520715334,-15.4632288398589,-15.4632288398589));
#24554=CARTESIAN_POINT('Ctrl Pts',(19.9886520715334,0.,-15.4632288398589));
#24555=CARTESIAN_POINT('Ctrl Pts',(19.9886520715334,15.4632288398589,-15.4632288398589));
#24556=CARTESIAN_POINT('Ctrl Pts',(19.9886520715334,15.4632288398589,0.));
#24557=CARTESIAN_POINT('Ctrl Pts',(18.514323186272,14.6153405598521,0.));
#24558=CARTESIAN_POINT('Ctrl Pts',(18.514323186272,14.6153405598521,14.6153405598521));
#24559=CARTESIAN_POINT('Ctrl Pts',(18.514323186272,0.,14.6153405598521));
#24560=CARTESIAN_POINT('Ctrl Pts',(18.514323186272,-14.6153405598521,14.6153405598521));
#24561=CARTESIAN_POINT('Ctrl Pts',(18.514323186272,-14.6153405598521,0.));
#24562=CARTESIAN_POINT('Ctrl Pts',(18.514323186272,-14.6153405598521,-14.6153405598521));
#24563=CARTESIAN_POINT('Ctrl Pts',(18.514323186272,0.,-14.6153405598521));
#24564=CARTESIAN_POINT('Ctrl Pts',(18.514323186272,14.6153405598521,-14.6153405598521));
#24565=CARTESIAN_POINT('Ctrl Pts',(18.514323186272,14.6153405598521,0.));
#24566=CARTESIAN_POINT('Ctrl Pts',(17.0194794456568,13.8492044429491,0.));
#24567=CARTESIAN_POINT('Ctrl Pts',(17.0194794456568,13.8492044429491,13.8492044429491));
#24568=CARTESIAN_POINT('Ctrl Pts',(17.0194794456568,0.,13.8492044429491));
#24569=CARTESIAN_POINT('Ctrl Pts',(17.0194794456568,-13.8492044429491,13.8492044429491));
#24570=CARTESIAN_POINT('Ctrl Pts',(17.0194794456568,-13.8492044429491,0.));
#24571=CARTESIAN_POINT('Ctrl Pts',(17.0194794456568,-13.8492044429491,-13.8492044429491));
#24572=CARTESIAN_POINT('Ctrl Pts',(17.0194794456568,0.,-13.8492044429491));
#24573=CARTESIAN_POINT('Ctrl Pts',(17.0194794456568,13.8492044429491,-13.8492044429491));
#24574=CARTESIAN_POINT('Ctrl Pts',(17.0194794456568,13.8492044429491,0.));
#24575=CARTESIAN_POINT('Ctrl Pts',(15.5121733229441,13.1688616684146,0.));
#24576=CARTESIAN_POINT('Ctrl Pts',(15.5121733229441,13.1688616684146,13.1688616684146));
#24577=CARTESIAN_POINT('Ctrl Pts',(15.5121733229441,0.,13.1688616684146));
#24578=CARTESIAN_POINT('Ctrl Pts',(15.5121733229441,-13.1688616684146,13.1688616684146));
#24579=CARTESIAN_POINT('Ctrl Pts',(15.5121733229441,-13.1688616684146,0.));
#24580=CARTESIAN_POINT('Ctrl Pts',(15.5121733229441,-13.1688616684146,-13.1688616684146));
#24581=CARTESIAN_POINT('Ctrl Pts',(15.5121733229441,0.,-13.1688616684146));
#24582=CARTESIAN_POINT('Ctrl Pts',(15.5121733229441,13.1688616684146,-13.1688616684146));
#24583=CARTESIAN_POINT('Ctrl Pts',(15.5121733229441,13.1688616684146,0.));
#24584=CARTESIAN_POINT('Ctrl Pts',(13.9995910956154,12.5772662595197,0.));
#24585=CARTESIAN_POINT('Ctrl Pts',(13.9995910956154,12.5772662595197,12.5772662595197));
#24586=CARTESIAN_POINT('Ctrl Pts',(13.9995910956154,0.,12.5772662595197));
#24587=CARTESIAN_POINT('Ctrl Pts',(13.9995910956154,-12.5772662595197,12.5772662595197));
#24588=CARTESIAN_POINT('Ctrl Pts',(13.9995910956154,-12.5772662595197,0.));
#24589=CARTESIAN_POINT('Ctrl Pts',(13.9995910956154,-12.5772662595197,-12.5772662595197));
#24590=CARTESIAN_POINT('Ctrl Pts',(13.9995910956154,0.,-12.5772662595197));
#24591=CARTESIAN_POINT('Ctrl Pts',(13.9995910956154,12.5772662595197,-12.5772662595197));
#24592=CARTESIAN_POINT('Ctrl Pts',(13.9995910956154,12.5772662595197,0.));
#24593=CARTESIAN_POINT('Ctrl Pts',(12.4874918670977,12.076207951456,0.));
#24594=CARTESIAN_POINT('Ctrl Pts',(12.4874918670977,12.076207951456,12.076207951456));
#24595=CARTESIAN_POINT('Ctrl Pts',(12.4874918670977,0.,12.076207951456));
#24596=CARTESIAN_POINT('Ctrl Pts',(12.4874918670977,-12.076207951456,12.076207951456));
#24597=CARTESIAN_POINT('Ctrl Pts',(12.4874918670977,-12.076207951456,0.));
#24598=CARTESIAN_POINT('Ctrl Pts',(12.4874918670977,-12.076207951456,-12.076207951456));
#24599=CARTESIAN_POINT('Ctrl Pts',(12.4874918670977,0.,-12.076207951456));
#24600=CARTESIAN_POINT('Ctrl Pts',(12.4874918670977,12.076207951456,-12.076207951456));
#24601=CARTESIAN_POINT('Ctrl Pts',(12.4874918670977,12.076207951456,0.));
#24602=CARTESIAN_POINT('Ctrl Pts',(10.979632440052,11.6661962584503,0.));
#24603=CARTESIAN_POINT('Ctrl Pts',(10.979632440052,11.6661962584503,11.6661962584503));
#24604=CARTESIAN_POINT('Ctrl Pts',(10.979632440052,0.,11.6661962584503));
#24605=CARTESIAN_POINT('Ctrl Pts',(10.979632440052,-11.6661962584503,11.6661962584503));
#24606=CARTESIAN_POINT('Ctrl Pts',(10.979632440052,-11.6661962584503,0.));
#24607=CARTESIAN_POINT('Ctrl Pts',(10.979632440052,-11.6661962584503,-11.6661962584503));
#24608=CARTESIAN_POINT('Ctrl Pts',(10.979632440052,0.,-11.6661962584503));
#24609=CARTESIAN_POINT('Ctrl Pts',(10.979632440052,11.6661962584503,-11.6661962584503));
#24610=CARTESIAN_POINT('Ctrl Pts',(10.979632440052,11.6661962584503,0.));
#24611=CARTESIAN_POINT('Ctrl Pts',(9.4782023240472,11.3469207764071,0.));
#24612=CARTESIAN_POINT('Ctrl Pts',(9.4782023240472,11.3469207764071,11.3469207764071));
#24613=CARTESIAN_POINT('Ctrl Pts',(9.4782023240472,0.,11.3469207764071));
#24614=CARTESIAN_POINT('Ctrl Pts',(9.47820232404719,-11.3469207764071,11.3469207764071));
#24615=CARTESIAN_POINT('Ctrl Pts',(9.47820232404719,-11.3469207764071,0.));
#24616=CARTESIAN_POINT('Ctrl Pts',(9.47820232404719,-11.3469207764071,-11.3469207764071));
#24617=CARTESIAN_POINT('Ctrl Pts',(9.4782023240472,0.,-11.3469207764071));
#24618=CARTESIAN_POINT('Ctrl Pts',(9.4782023240472,11.3469207764071,-11.3469207764071));
#24619=CARTESIAN_POINT('Ctrl Pts',(9.4782023240472,11.3469207764071,0.));
#24620=CARTESIAN_POINT('Ctrl Pts',(8.28303567503975,11.1635245405655,0.));
#24621=CARTESIAN_POINT('Ctrl Pts',(8.28303567503975,11.1635245405655,11.1635245405655));
#24622=CARTESIAN_POINT('Ctrl Pts',(8.28303567503976,0.,11.1635245405655));
#24623=CARTESIAN_POINT('Ctrl Pts',(8.28303567503978,-11.1635245405655,11.1635245405655));
#24624=CARTESIAN_POINT('Ctrl Pts',(8.28303567503978,-11.1635245405655,0.));
#24625=CARTESIAN_POINT('Ctrl Pts',(8.28303567503978,-11.1635245405655,-11.1635245405655));
#24626=CARTESIAN_POINT('Ctrl Pts',(8.28303567503976,0.,-11.1635245405655));
#24627=CARTESIAN_POINT('Ctrl Pts',(8.28303567503975,11.1635245405655,-11.1635245405655));
#24628=CARTESIAN_POINT('Ctrl Pts',(8.28303567503975,11.1635245405655,0.));
#24629=CARTESIAN_POINT('Ctrl Pts',(7.39016039139644,11.0661718180104,0.));
#24630=CARTESIAN_POINT('Ctrl Pts',(7.39016039139644,11.0661718180104,11.0661718180104));
#24631=CARTESIAN_POINT('Ctrl Pts',(7.39016039139642,0.,11.0661718180104));
#24632=CARTESIAN_POINT('Ctrl Pts',(7.3901603913964,-11.0661718180104,11.0661718180104));
#24633=CARTESIAN_POINT('Ctrl Pts',(7.3901603913964,-11.0661718180104,0.));
#24634=CARTESIAN_POINT('Ctrl Pts',(7.3901603913964,-11.0661718180104,-11.0661718180104));
#24635=CARTESIAN_POINT('Ctrl Pts',(7.39016039139642,0.,-11.0661718180104));
#24636=CARTESIAN_POINT('Ctrl Pts',(7.39016039139644,11.0661718180104,-11.0661718180104));
#24637=CARTESIAN_POINT('Ctrl Pts',(7.39016039139644,11.0661718180104,0.));
#24638=CARTESIAN_POINT('Ctrl Pts',(6.79646156908522,11.0190876606754,0.));
#24639=CARTESIAN_POINT('Ctrl Pts',(6.79646156908522,11.0190876606754,11.0190876606754));
#24640=CARTESIAN_POINT('Ctrl Pts',(6.79646156908522,0.,11.0190876606754));
#24641=CARTESIAN_POINT('Ctrl Pts',(6.79646156908521,-11.0190876606754,11.0190876606754));
#24642=CARTESIAN_POINT('Ctrl Pts',(6.79646156908521,-11.0190876606754,0.));
#24643=CARTESIAN_POINT('Ctrl Pts',(6.79646156908521,-11.0190876606754,-11.0190876606754));
#24644=CARTESIAN_POINT('Ctrl Pts',(6.79646156908522,0.,-11.0190876606754));
#24645=CARTESIAN_POINT('Ctrl Pts',(6.79646156908522,11.0190876606754,-11.0190876606754));
#24646=CARTESIAN_POINT('Ctrl Pts',(6.79646156908522,11.0190876606754,0.));
#24647=CARTESIAN_POINT('Ctrl Pts',(6.5,11.,0.));
#24648=CARTESIAN_POINT('Ctrl Pts',(6.5,11.,11.));
#24649=CARTESIAN_POINT('Ctrl Pts',(6.49999999999999,0.,11.));
#24650=CARTESIAN_POINT('Ctrl Pts',(6.49999999999997,-11.,11.));
#24651=CARTESIAN_POINT('Ctrl Pts',(6.49999999999997,-11.,0.));
#24652=CARTESIAN_POINT('Ctrl Pts',(6.49999999999997,-11.,-11.));
#24653=CARTESIAN_POINT('Ctrl Pts',(6.49999999999999,0.,-11.));
#24654=CARTESIAN_POINT('Ctrl Pts',(6.5,11.,-11.));
#24655=CARTESIAN_POINT('Ctrl Pts',(6.5,11.,0.));
#24656=CARTESIAN_POINT('',(12.7552064848291,12.1808231353727,0.));
#24657=CARTESIAN_POINT('',(20.644698628669,15.8947820241755,0.));
#24658=CARTESIAN_POINT('Ctrl Pts',(12.7552064848291,12.1808231353727,0.));
#24659=CARTESIAN_POINT('Ctrl Pts',(13.0039389302743,12.2584833095898,0.));
#24660=CARTESIAN_POINT('Ctrl Pts',(13.5550060380175,12.4372815016706,0.));
#24661=CARTESIAN_POINT('Ctrl Pts',(14.4089440713075,12.7375124365726,0.));
#24662=CARTESIAN_POINT('Ctrl Pts',(15.5654093565171,13.1928904640524,0.));
#24663=CARTESIAN_POINT('Ctrl Pts',(17.0194794456568,13.8492044429491,0.));
#24664=CARTESIAN_POINT('Ctrl Pts',(18.3518881687479,14.532089494745,0.));
#24665=CARTESIAN_POINT('Ctrl Pts',(19.3730718999235,15.110588732192,0.));
#24666=CARTESIAN_POINT('Ctrl Pts',(20.0905786930687,15.5451447711833,0.));
#24667=CARTESIAN_POINT('Ctrl Pts',(20.5126995086046,15.8107444141161,0.));
#24668=CARTESIAN_POINT('Ctrl Pts',(20.644698628669,15.8947820241755,0.));
#24669=CARTESIAN_POINT('',(6.9,10.3676856018661,3.76156693666918));
#24670=CARTESIAN_POINT('Ctrl Pts',(12.7552064848291,12.1808231353727,6.59194920871187E-16));
#24671=CARTESIAN_POINT('Ctrl Pts',(12.4248760810931,12.0776861414938,0.209258199173966));
#24672=CARTESIAN_POINT('Ctrl Pts',(12.0982104932216,11.9767199532399,0.41544547449944));
#24673=CARTESIAN_POINT('Ctrl Pts',(11.7781027672104,11.8786008701973,0.615504762505627));
#24674=CARTESIAN_POINT('Ctrl Pts',(10.6475684461636,11.5320706807779,1.32206031539251));
#24675=CARTESIAN_POINT('Ctrl Pts',(9.62260979259592,11.2216626837413,1.98990731305582));
#24676=CARTESIAN_POINT('Ctrl Pts',(8.83596486703766,10.9799837756658,2.49396533620343));
#24677=CARTESIAN_POINT('Ctrl Pts',(8.38139303840122,10.8403268356446,2.78524106922678));
#24678=CARTESIAN_POINT('Ctrl Pts',(7.99983674904323,10.7217571528206,3.03224089473385));
#24679=CARTESIAN_POINT('Ctrl Pts',(7.59399878797648,10.5924943041424,3.29947542405694));
#24680=CARTESIAN_POINT('Ctrl Pts',(7.36159608752553,10.5184720637837,3.45250700864596));
#24681=CARTESIAN_POINT('Ctrl Pts',(7.13011481847682,10.4436463911284,3.6065023681803));
#24682=CARTESIAN_POINT('Ctrl Pts',(6.9,10.3676856018661,3.76156693666918));
#24683=CARTESIAN_POINT('',(6.9,11.02768739857,0.168526548660245));
#24684=CARTESIAN_POINT('Ctrl Pts',(6.90000000000001,10.3676856018661,3.76156693666918));
#24685=CARTESIAN_POINT('Ctrl Pts',(6.90000000000001,10.5551707158657,3.24481773355661));
#24686=CARTESIAN_POINT('Ctrl Pts',(6.90000000000001,10.7040448708755,2.71398840242746));
#24687=CARTESIAN_POINT('Ctrl Pts',(6.90000000000001,10.9457448952802,1.51153848953113));
#24688=CARTESIAN_POINT('Ctrl Pts',(6.90000000000001,11.0174195217678,0.840414370027655));
#24689=CARTESIAN_POINT('Ctrl Pts',(6.90000000000001,11.02768739857,0.168526548660246));
#24690=CARTESIAN_POINT('',(7.15673001668648,11.0509590216245,0.));
#24691=CARTESIAN_POINT('Ctrl Pts',(6.9,11.02768739857,0.168526548660244));
#24692=CARTESIAN_POINT('Ctrl Pts',(6.98321811561625,11.0352247901797,0.113609938717567));
#24693=CARTESIAN_POINT('Ctrl Pts',(7.06875995041873,11.0429732858603,0.0574496110044951));
#24694=CARTESIAN_POINT('Ctrl Pts',(7.15673001668648,11.0509590216245,5.89805981832114E-16));
#24695=CARTESIAN_POINT('',(6.5,11.,0.));
#24696=CARTESIAN_POINT('Ctrl Pts',(6.5,11.,0.));
#24697=CARTESIAN_POINT('Ctrl Pts',(6.63119408856029,11.0084469236697,0.));
#24698=CARTESIAN_POINT('Ctrl Pts',(6.76246413041996,11.0177661811298,0.));
#24699=CARTESIAN_POINT('Ctrl Pts',(6.89381012554657,11.0279577720712,0.));
#24700=CARTESIAN_POINT('Ctrl Pts',(7.02523209337025,11.0390219194522,0.));
#24701=CARTESIAN_POINT('Ctrl Pts',(7.15673001668648,11.0509590216245,0.));
#24702=CARTESIAN_POINT('Origin',(6.49999999999999,0.,0.));
#24703=CARTESIAN_POINT('',(37.5,27.2791366260183,-17.4816676818611));
#24704=CARTESIAN_POINT('Ctrl Pts',(7.15673001668648,11.0509590216245,-9.37018525099673E-16));
#24705=CARTESIAN_POINT('Ctrl Pts',(7.1627757905312,11.0515078441327,-0.00394824478753294));
#24706=CARTESIAN_POINT('Ctrl Pts',(7.1688330327612,11.0520577886114,-0.00790257982403587));
#24707=CARTESIAN_POINT('Ctrl Pts',(7.17490177695966,11.0526088641831,-0.0118630202121361));
#24708=CARTESIAN_POINT('Ctrl Pts',(7.97363370710642,11.1251381454716,-0.533112572338659));
#24709=CARTESIAN_POINT('Ctrl Pts',(8.96287699192994,11.2096234568595,-1.17519935778271));
#24710=CARTESIAN_POINT('Ctrl Pts',(10.2403166389167,11.35643287004,-1.93497252663744));
#24711=CARTESIAN_POINT('Ctrl Pts',(10.4394308581993,11.3793160189682,-2.05339819293429));
#24712=CARTESIAN_POINT('Ctrl Pts',(10.6449414398479,11.4036124907892,-2.17569004699468));
#24713=CARTESIAN_POINT('Ctrl Pts',(10.8572312781278,11.4296465357576,-2.30181054310029));
#24714=CARTESIAN_POINT('Ctrl Pts',(11.0079313537829,11.4481275548123,-2.39134082141595));
#24715=CARTESIAN_POINT('Ctrl Pts',(11.2445785601825,11.4774507093007,-2.53195589857672));
#24716=CARTESIAN_POINT('Ctrl Pts',(11.5512317955498,11.5182357344436,-2.71303157158667));
#24717=CARTESIAN_POINT('Ctrl Pts',(12.0044708154773,11.5785167381687,-2.98066468646132));
#24718=CARTESIAN_POINT('Ctrl Pts',(12.6082499220052,11.6630669066833,-3.33560663936012));
#24719=CARTESIAN_POINT('Ctrl Pts',(13.3027146141536,11.7808809827897,-3.73133446864291));
#24720=CARTESIAN_POINT('Ctrl Pts',(14.2466220417637,11.9410123512684,-4.26920261600178));
#24721=CARTESIAN_POINT('Ctrl Pts',(15.3788107201965,12.1625996834205,-4.92664534658129));
#24722=CARTESIAN_POINT('Ctrl Pts',(16.3720853361384,12.4089023460099,-5.48881820879722));
#24723=CARTESIAN_POINT('Ctrl Pts',(17.5300464833452,12.6960423867947,-6.14420023710243));
#24724=CARTESIAN_POINT('Ctrl Pts',(18.5522571217465,13.0002012582107,-6.74248287738912));
#24725=CARTESIAN_POINT('Ctrl Pts',(19.459740928474,13.3207494833101,-7.26206394073252));
#24726=CARTESIAN_POINT('Ctrl Pts',(20.7212139011992,13.7663364121569,-7.98432197298446));
#24727=CARTESIAN_POINT('Ctrl Pts',(21.7483180915102,14.2134327156149,-8.59417302928553));
#24728=CARTESIAN_POINT('Ctrl Pts',(22.5801692622301,14.6264461342272,-9.07708247839831));
#24729=CARTESIAN_POINT('Ctrl Pts',(23.3330995247457,15.0002753871561,-9.51417645757393));
#24730=CARTESIAN_POINT('Ctrl Pts',(23.9217876539353,15.3300824095171,-9.86132841188702));
#24731=CARTESIAN_POINT('Ctrl Pts',(24.4822919858724,15.6683207380631,-10.1904384385981));
#24732=CARTESIAN_POINT('Ctrl Pts',(24.941879286597,15.9456603259318,-10.4602932464902));
#24733=CARTESIAN_POINT('Ctrl Pts',(25.362627650419,16.2195872238312,-10.7067050298478));
#24734=CARTESIAN_POINT('Ctrl Pts',(25.7525302890143,16.489196921628,-10.9324873590558));
#24735=CARTESIAN_POINT('Ctrl Pts',(26.1776080055426,16.7831294661889,-11.1786386476902));
#24736=CARTESIAN_POINT('Ctrl Pts',(26.5661459570144,17.0742513036038,-11.3970084746332));
#24737=CARTESIAN_POINT('Ctrl Pts',(26.9267016829611,17.3573257272023,-11.599025816134));
#24738=CARTESIAN_POINT('Ctrl Pts',(27.1778854595225,17.5545315892941,-11.7397626707099));
#24739=CARTESIAN_POINT('Ctrl Pts',(27.4155006347892,17.7480067679896,-11.8724116206432));
#24740=CARTESIAN_POINT('Ctrl Pts',(27.6422489803864,17.9373681845498,-11.9995864201782));
#24741=CARTESIAN_POINT('Ctrl Pts',(27.8555706599492,18.1155167629601,-12.1192306970236));
#24742=CARTESIAN_POINT('Ctrl Pts',(28.1190985482968,18.3396168643745,-12.2669566516514));
#24743=CARTESIAN_POINT('Ctrl Pts',(28.4603120647768,18.6410520014603,-12.4627251930521));
#24744=CARTESIAN_POINT('Ctrl Pts',(28.6017780250843,18.7660259813254,-12.5438901626961));
#24745=CARTESIAN_POINT('Ctrl Pts',(28.7540312887841,18.9021185408524,-12.6319528845987));
#24746=CARTESIAN_POINT('Ctrl Pts',(28.9157341130969,19.0484400367167,-12.7269375546994));
#24747=CARTESIAN_POINT('Ctrl Pts',(29.4787137469301,19.5578685053511,-13.0576332925161));
#24748=CARTESIAN_POINT('Ctrl Pts',(30.1711677436348,20.2292610528631,-13.4573416990291));
#24749=CARTESIAN_POINT('Ctrl Pts',(30.8055547543663,20.8740009526386,-13.8222365905983));
#24750=CARTESIAN_POINT('Ctrl Pts',(31.1893125644353,21.2640215044727,-14.0429713504927));
#24751=CARTESIAN_POINT('Ctrl Pts',(31.5650207098983,21.6546118380209,-14.2588547919359));
#24752=CARTESIAN_POINT('Ctrl Pts',(31.9311744366493,22.036212583627,-14.4706295271113));
#24753=CARTESIAN_POINT('Ctrl Pts',(32.1142513000247,22.22701295643,-14.5765168946991));
#24754=CARTESIAN_POINT('Ctrl Pts',(32.2949430642597,22.4155611447437,-14.6813807665083));
#24755=CARTESIAN_POINT('Ctrl Pts',(32.4730466959716,22.6006686536293,-14.7853297275554));
#24756=CARTESIAN_POINT('Ctrl Pts',(32.5932788659621,22.7256289212046,-14.8555024075554));
#24757=CARTESIAN_POINT('Ctrl Pts',(32.7123311760698,22.8490214255785,-14.9252583804635));
#24758=CARTESIAN_POINT('Ctrl Pts',(32.8301302693162,22.9704904553367,-14.9946314854392));
#24759=CARTESIAN_POINT('Ctrl Pts',(32.8868306159552,23.0289572559155,-15.0280229062995));
#24760=CARTESIAN_POINT('Ctrl Pts',(32.9387123022521,23.0823367414253,-15.0586441387564));
#24761=CARTESIAN_POINT('Ctrl Pts',(33.,23.1451817466334,-15.0949277194305));
#24762=CARTESIAN_POINT('Ctrl Pts',(33.0955022515318,23.2431106902134,-15.1514670213678));
#24763=CARTESIAN_POINT('Ctrl Pts',(33.2417478451795,23.3926999986789,-15.2378324488783));
#24764=CARTESIAN_POINT('Ctrl Pts',(33.3688392456214,23.5219737265912,-15.3124686704877));
#24765=CARTESIAN_POINT('Ctrl Pts',(34.2661932188016,24.4347364545705,-15.8394524771927));
#24766=CARTESIAN_POINT('Ctrl Pts',(35.2319960543294,25.3874835189992,-16.3895212513103));
#24767=CARTESIAN_POINT('Ctrl Pts',(36.3004607334072,26.3047571717506,-16.9191094416468));
#24768=CARTESIAN_POINT('Ctrl Pts',(36.6891719087509,26.6384645246042,-17.1117754716474));
#24769=CARTESIAN_POINT('Ctrl Pts',(37.0893059759317,26.9653128027505,-17.3004814130194));
#24770=CARTESIAN_POINT('Ctrl Pts',(37.5,27.2791366260183,-17.4816676818611));
#24771=CARTESIAN_POINT('',(37.5,25.9430157904516,-19.4092743732572));
#24772=CARTESIAN_POINT('Origin',(37.5,0.,0.));
#24773=CARTESIAN_POINT('',(36.8,24.9564959511929,-19.6435328718186));
#24774=CARTESIAN_POINT('Ctrl Pts',(37.5,25.9430157904516,-19.4092743732572));
#24775=CARTESIAN_POINT('Ctrl Pts',(37.2470086540957,25.6235740187167,-19.4640189486865));
#24776=CARTESIAN_POINT('Ctrl Pts',(37.0122659037829,25.2931530107001,-19.5406617074869));
#24777=CARTESIAN_POINT('Ctrl Pts',(36.8,24.9564959511929,-19.6435328718186));
#24778=CARTESIAN_POINT('',(36.8,19.6435328718186,-24.956495951193));
#24779=CARTESIAN_POINT('Ctrl Pts',(36.8,24.9564959511929,-19.6435328718186));
#24780=CARTESIAN_POINT('Ctrl Pts',(36.8,24.4957748831848,-20.2288646216318));
#24781=CARTESIAN_POINT('Ctrl Pts',(36.8,24.0141222843113,-20.7984186457787));
#24782=CARTESIAN_POINT('Ctrl Pts',(36.8,22.3234241559746,-22.6602579716864));
#24783=CARTESIAN_POINT('Ctrl Pts',(36.8,21.029056769996,-23.8659348286794));
#24784=CARTESIAN_POINT('Ctrl Pts',(36.8,19.6435328718186,-24.956495951193));
#24785=CARTESIAN_POINT('',(37.5,19.4092743732571,-25.9430157904517));
#24786=CARTESIAN_POINT('Ctrl Pts',(36.8,19.6435328718186,-24.9564959511929));
#24787=CARTESIAN_POINT('Ctrl Pts',(37.0122659037829,19.5406617074868,-25.2931530107001));
#24788=CARTESIAN_POINT('Ctrl Pts',(37.2470086540956,19.4640189486865,-25.6235740187166));
#24789=CARTESIAN_POINT('Ctrl Pts',(37.5,19.4092743732571,-25.9430157904517));
#24790=CARTESIAN_POINT('',(37.5,17.4816676818611,-27.2791366260183));
#24791=CARTESIAN_POINT('Origin',(37.5,0.,0.));
#24792=CARTESIAN_POINT('',(6.9,10.8594625780008,-1.92623027574191));
#24793=CARTESIAN_POINT('Ctrl Pts',(37.5,17.4816676818611,-27.2791366260183));
#24794=CARTESIAN_POINT('Ctrl Pts',(36.6490696321361,17.1062619312001,-26.6289147924198));
#24795=CARTESIAN_POINT('Ctrl Pts',(35.8406537800854,16.6974222041734,-25.920783613057));
#24796=CARTESIAN_POINT('Ctrl Pts',(35.0774452370496,16.2828706254179,-25.2027592162947));
#24797=CARTESIAN_POINT('Ctrl Pts',(34.6958409655316,16.0755948360402,-24.8437470179135));
#24798=CARTESIAN_POINT('Ctrl Pts',(34.3255255041561,15.866901215486,-24.4822790638982));
#24799=CARTESIAN_POINT('Ctrl Pts',(33.966681063517,15.6603259087598,-24.1244801370593));
#24800=CARTESIAN_POINT('Ctrl Pts',(33.7186145566451,15.5175219275854,-23.8771363861421));
#24801=CARTESIAN_POINT('Ctrl Pts',(33.4671024168887,15.3704773316442,-23.6224476749935));
#24802=CARTESIAN_POINT('Ctrl Pts',(33.2400985609687,15.2367408626649,-23.3908093158965));
#24803=CARTESIAN_POINT('Ctrl Pts',(33.1387264796141,15.1770187748682,-23.2873676254985));
#24804=CARTESIAN_POINT('Ctrl Pts',(33.0532004124033,15.1264234604399,-23.1997339702838));
#24805=CARTESIAN_POINT('Ctrl Pts',(33.,15.0949277194305,-23.1451817466334));
#24806=CARTESIAN_POINT('Ctrl Pts',(32.9185691496266,15.0467189770979,-23.0616817555444));
#24807=CARTESIAN_POINT('Ctrl Pts',(32.851682063341,15.0068117561527,-22.993092707295));
#24808=CARTESIAN_POINT('Ctrl Pts',(32.7777321456029,14.9624828491712,-22.917277339216));
#24809=CARTESIAN_POINT('Ctrl Pts',(32.1788699540295,14.6034979145429,-22.3033083332787));
#24810=CARTESIAN_POINT('Ctrl Pts',(31.5692879871724,14.2222611802151,-21.6797224976956));
#24811=CARTESIAN_POINT('Ctrl Pts',(30.9513498040902,13.8532805894451,-21.057417903561));
#24812=CARTESIAN_POINT('Ctrl Pts',(30.6423807125491,13.6687902940601,-20.7462656064936));
#24813=CARTESIAN_POINT('Ctrl Pts',(30.3347880607216,13.4893931931417,-20.438831527849));
#24814=CARTESIAN_POINT('Ctrl Pts',(30.0249306372018,13.3164737289158,-20.1317191404522));
#24815=CARTESIAN_POINT('Ctrl Pts',(29.8700019254419,13.2300139968029,-19.9781629467538));
#24816=CARTESIAN_POINT('Ctrl Pts',(29.7145097313597,13.1451740097154,-19.8246838084796));
#24817=CARTESIAN_POINT('Ctrl Pts',(29.5580100720529,13.0621556215307,-19.6708282829286));
#24818=CARTESIAN_POINT('Ctrl Pts',(29.4797602423995,13.0206464274383,-19.5939005201531));
#24819=CARTESIAN_POINT('Ctrl Pts',(29.4012586241266,12.9795931491564,-19.5168782891895));
#24820=CARTESIAN_POINT('Ctrl Pts',(29.3224502420539,12.9390249501939,-19.4397024434204));
#24821=CARTESIAN_POINT('Ctrl Pts',(29.2736528206195,12.9139054965325,-19.3919158733691));
#24822=CARTESIAN_POINT('Ctrl Pts',(29.2247377937366,12.888972078638,-19.3440703736513));
#24823=CARTESIAN_POINT('Ctrl Pts',(29.1756921969699,12.8642322645676,-19.2961515487725));
#24824=CARTESIAN_POINT('Ctrl Pts',(29.145528605723,12.8490170018663,-19.2666809348548));
#24825=CARTESIAN_POINT('Ctrl Pts',(29.1181490968401,12.8352852879351,-19.2399471036097));
#24826=CARTESIAN_POINT('Ctrl Pts',(29.0849408699094,12.8187535959654,-19.2075463476651));
#24827=CARTESIAN_POINT('Ctrl Pts',(29.0475462331541,12.8001378289312,-19.171060976083));
#24828=CARTESIAN_POINT('Ctrl Pts',(28.9599837408533,12.7566467272304,-19.085912836999));
#24829=CARTESIAN_POINT('Ctrl Pts',(28.8924081848686,12.723282629515,-19.0206341515183));
#24830=CARTESIAN_POINT('Ctrl Pts',(28.4410807636346,12.5004486185436,-18.5846471980972));
#24831=CARTESIAN_POINT('Ctrl Pts',(27.9936088568923,12.2860610268384,-18.1669902803128));
#24832=CARTESIAN_POINT('Ctrl Pts',(27.5122543097622,12.0773485866518,-17.7276863429211));
#24833=CARTESIAN_POINT('Ctrl Pts',(27.1397294107683,11.9158240281682,-17.3877048139625));
#24834=CARTESIAN_POINT('Ctrl Pts',(26.7276341641932,11.7479547990202,-17.0180715474313));
#24835=CARTESIAN_POINT('Ctrl Pts',(26.2530417505368,11.5897211649258,-16.593147989986));
#24836=CARTESIAN_POINT('Ctrl Pts',(25.8694949138879,11.461842993969,-16.2497415604139));
#24837=CARTESIAN_POINT('Ctrl Pts',(25.4447383161179,11.3368019000543,-15.8721943512539));
#24838=CARTESIAN_POINT('Ctrl Pts',(24.9635886608488,11.2164808476641,-15.4528606650932));
#24839=CARTESIAN_POINT('Ctrl Pts',(24.6119820458997,11.1285546120849,-15.1464269052216));
#24840=CARTESIAN_POINT('Ctrl Pts',(24.2873626784893,11.0505455233575,-14.8634583858277));
#24841=CARTESIAN_POINT('Ctrl Pts',(23.642661641557,10.9290047499035,-14.322314359714));
#24842=CARTESIAN_POINT('Ctrl Pts',(23.576053321007,10.9164475701654,-14.2664051976524));
#24843=CARTESIAN_POINT('Ctrl Pts',(23.5065967304414,10.903616097419,-14.2082779526344));
#24844=CARTESIAN_POINT('Ctrl Pts',(23.4342591639586,10.8905593535264,-14.1479547088373));
#24845=CARTESIAN_POINT('Ctrl Pts',(22.7443384436268,10.7660304456639,-13.5726207871031));
#24846=CARTESIAN_POINT('Ctrl Pts',(21.7987837593176,10.6409180002013,-12.7862027918382));
#24847=CARTESIAN_POINT('Ctrl Pts',(20.5610365528855,10.544989531356,-11.8220942510713));
#24848=CARTESIAN_POINT('Ctrl Pts',(19.7234582214113,10.480075139743,-11.1696860543579));
#24849=CARTESIAN_POINT('Ctrl Pts',(18.7603809281633,10.4499377288461,-10.4236916548838));
#24850=CARTESIAN_POINT('Ctrl Pts',(17.6514222906382,10.4358767824859,-9.60745933070834));
#24851=CARTESIAN_POINT('Ctrl Pts',(16.7565277906389,10.4245300440805,-8.94878569500228));
#24852=CARTESIAN_POINT('Ctrl Pts',(15.7613807992389,10.4463397170533,-8.21650708627012));
#24853=CARTESIAN_POINT('Ctrl Pts',(14.7199652846762,10.4731931404427,-7.48053645516582));
#24854=CARTESIAN_POINT('Ctrl Pts',(13.7316067501733,10.4986784628874,-6.78206130838355));
#24855=CARTESIAN_POINT('Ctrl Pts',(12.7260968661244,10.5503343111255,-6.06464296565695));
#24856=CARTESIAN_POINT('Ctrl Pts',(11.7781012037546,10.5949225697956,-5.40625658879284));
#24857=CARTESIAN_POINT('Ctrl Pts',(10.6475718363526,10.6480961631663,-4.62109990117507));
#24858=CARTESIAN_POINT('Ctrl Pts',(9.62260863652897,10.713198677066,-3.88752023758455));
#24859=CARTESIAN_POINT('Ctrl Pts',(8.83596460437641,10.7559275652365,-3.33015436441791));
#24860=CARTESIAN_POINT('Ctrl Pts',(8.38131550044803,10.7806231707767,-3.00801895826468));
#24861=CARTESIAN_POINT('Ctrl Pts',(7.9996968849037,10.8014421627467,-2.73478088895419));
#24862=CARTESIAN_POINT('Ctrl Pts',(7.59379043301474,10.8231179952784,-2.43866561789793));
#24863=CARTESIAN_POINT('Ctrl Pts',(7.36145773430791,10.8355248063683,-2.26917518547774));
#24864=CARTESIAN_POINT('Ctrl Pts',(7.13004605045641,10.8477177778402,-2.09844904428941));
#24865=CARTESIAN_POINT('Ctrl Pts',(6.9,10.8594625780007,-1.92623027574191));
#24866=CARTESIAN_POINT('',(6.9,9.63452070648529,-5.36789542693313));
#24867=CARTESIAN_POINT('Ctrl Pts',(6.90000000000001,10.8594625780008,-1.92623027574191));
#24868=CARTESIAN_POINT('Ctrl Pts',(6.90000000000001,10.7829659225815,-2.35749364924905));
#24869=CARTESIAN_POINT('Ctrl Pts',(6.90000000000001,10.6806923192591,-2.78469328079874));
#24870=CARTESIAN_POINT('Ctrl Pts',(6.90000000000001,10.3240838050858,-3.95869001001801));
#24871=CARTESIAN_POINT('Ctrl Pts',(6.90000000000001,10.0158641401962,-4.6834444613023));
#24872=CARTESIAN_POINT('Ctrl Pts',(6.90000000000001,9.63452070648529,-5.36789542693313));
#24873=CARTESIAN_POINT('',(37.5,14.8835914705078,-28.7791366260183));
#24874=CARTESIAN_POINT('Ctrl Pts',(6.9,9.63452070648529,-5.36789542693313));
#24875=CARTESIAN_POINT('Ctrl Pts',(6.98893730997611,9.61215150215923,-5.42275082836604));
#24876=CARTESIAN_POINT('Ctrl Pts',(7.080528923883,9.58928076274039,-5.47895708413964));
#24877=CARTESIAN_POINT('Ctrl Pts',(7.17490192378011,9.56590850800827,-5.5365781986047));
#24878=CARTESIAN_POINT('Ctrl Pts',(7.97363347623888,9.36809602639803,-6.02425796147394));
#24879=CARTESIAN_POINT('Ctrl Pts',(8.96286060506815,9.12022229066503,-6.62255487684896));
#24880=CARTESIAN_POINT('Ctrl Pts',(10.2403127965964,8.8674738587251,-7.35394959882413));
#24881=CARTESIAN_POINT('Ctrl Pts',(10.4394276407776,8.82807828292467,-7.4679511615181));
#24882=CARTESIAN_POINT('Ctrl Pts',(10.6449386760845,8.78797362786098,-7.58600750915109));
#24883=CARTESIAN_POINT('Ctrl Pts',(10.8572270226684,8.74745979681899,-7.70824722252714));
#24884=CARTESIAN_POINT('Ctrl Pts',(11.0079272577466,8.71869965072432,-7.79502331663734));
#24885=CARTESIAN_POINT('Ctrl Pts',(11.2445718662815,8.67378718135597,-7.93145962014351));
#24886=CARTESIAN_POINT('Ctrl Pts',(11.5512244267323,8.61857029386601,-8.10866787119591));
#24887=CARTESIAN_POINT('Ctrl Pts',(12.0044642696576,8.53695840914545,-8.37058591862391));
#24888=CARTESIAN_POINT('Ctrl Pts',(12.6082461583963,8.43270942691138,-8.72025136351868));
#24889=CARTESIAN_POINT('Ctrl Pts',(13.3027146141536,8.3368749757354,-9.12187093125612));
#24890=CARTESIAN_POINT('Ctrl Pts',(14.2466220416827,8.20661873511246,-9.6677440949479));
#24891=CARTESIAN_POINT('Ctrl Pts',(15.3788107201281,8.06979762861672,-10.347899867244));
#24892=CARTESIAN_POINT('Ctrl Pts',(16.3720853361384,8.00201556032624,-10.9579071785779));
#24893=CARTESIAN_POINT('Ctrl Pts',(17.530046483338,7.92299511593749,-11.6690546846619));
#24894=CARTESIAN_POINT('Ctrl Pts',(18.5522571217484,7.88726310522635,-12.3392620855072));
#24895=CARTESIAN_POINT('Ctrl Pts',(19.459740928474,7.90507547962869,-12.9495065982363));
#24896=CARTESIAN_POINT('Ctrl Pts',(20.7212139012673,7.92983606347967,-13.7977938667231));
#24897=CARTESIAN_POINT('Ctrl Pts',(21.7483180915983,8.0121072920729,-14.5494885257539));
#24898=CARTESIAN_POINT('Ctrl Pts',(22.5801692622301,8.12833268012626,-15.1742070856531));
#24899=CARTESIAN_POINT('Ctrl Pts',(23.3330995245126,8.23353132022012,-15.7396562017498));
#24900=CARTESIAN_POINT('Ctrl Pts',(23.9217876533125,8.34557660269292,-16.2052021240247));
#24901=CARTESIAN_POINT('Ctrl Pts',(24.4822919849709,8.47394457429969,-16.6593389318286));
#24902=CARTESIAN_POINT('Ctrl Pts',(24.9418792860364,8.57920029897796,-17.0317098449944));
#24903=CARTESIAN_POINT('Ctrl Pts',(25.3626276501528,8.69322205972909,-17.3820721583649));
#24904=CARTESIAN_POINT('Ctrl Pts',(25.7525302890143,8.8138197426061,-17.7124102403086));
#24905=CARTESIAN_POINT('Ctrl Pts',(26.1776080054479,8.94529714884838,-18.0725497816404));
#24906=CARTESIAN_POINT('Ctrl Pts',(26.5661459568577,9.08823114214577,-18.4072245178454));
#24907=CARTESIAN_POINT('Ctrl Pts',(26.9267016827717,9.2323721133757,-18.7237138793584));
#24908=CARTESIAN_POINT('Ctrl Pts',(27.1778777838254,9.33278590395925,-18.9441917642909));
#24909=CARTESIAN_POINT('Ctrl Pts',(27.4154861114682,9.43401273563673,-19.1558005175256));
#24910=CARTESIAN_POINT('Ctrl Pts',(27.6422281937235,9.5344141104218,-19.3606119908812));
#24911=CARTESIAN_POINT('Ctrl Pts',(27.855555992985,9.6288756418353,-19.5533066174801));
#24912=CARTESIAN_POINT('Ctrl Pts',(28.119083718991,9.74908875996703,-19.7932907120163));
#24913=CARTESIAN_POINT('Ctrl Pts',(28.4603051775176,9.91225869656093,-20.1135561540163));
#24914=CARTESIAN_POINT('Ctrl Pts',(28.6017730832022,9.97990775151866,-20.2463358494625));
#24915=CARTESIAN_POINT('Ctrl Pts',(28.7540286646177,10.0537371137215,-20.3906488456919));
#24916=CARTESIAN_POINT('Ctrl Pts',(28.9157341130969,10.1329641969115,-20.5460712531062));
#24917=CARTESIAN_POINT('Ctrl Pts',(29.4787137469273,10.4087943232502,-21.0871763972933));
#24918=CARTESIAN_POINT('Ctrl Pts',(30.1711677436288,10.7903831220487,-21.7690303051924));
#24919=CARTESIAN_POINT('Ctrl Pts',(30.805554754357,11.1662968083009,-22.4074085008868));
#24920=CARTESIAN_POINT('Ctrl Pts',(31.1893125644278,11.393697134241,-22.7935806863724));
#24921=CARTESIAN_POINT('Ctrl Pts',(31.5650207098923,11.6240165648458,-23.1758363976944));
#24922=CARTESIAN_POINT('Ctrl Pts',(31.9311744366447,11.8486051370568,-23.5500390710405));
#24923=CARTESIAN_POINT('Ctrl Pts',(32.1142513000209,11.9608994231623,-23.7371404077135));
#24924=CARTESIAN_POINT('Ctrl Pts',(32.2949430642566,12.0717550081754,-23.9222292787971));
#24925=CARTESIAN_POINT('Ctrl Pts',(32.4730466959692,12.1800883327784,-24.1048054742044));
#24926=CARTESIAN_POINT('Ctrl Pts',(32.5932788659337,12.2532207589465,-24.228056931497));
#24927=CARTESIAN_POINT('Ctrl Pts',(32.7123311760158,12.3252038159015,-24.3501636282619));
#24928=CARTESIAN_POINT('Ctrl Pts',(32.8301302692372,12.3957125289427,-24.4709770143638));
#24929=CARTESIAN_POINT('Ctrl Pts',(32.8868306159027,12.4296505531077,-24.5291282334138));
#24930=CARTESIAN_POINT('Ctrl Pts',(32.9387123022199,12.460567927384,-24.5823367413923));
#24931=CARTESIAN_POINT('Ctrl Pts',(33.,12.4968515080772,-24.6451817466334));
#24932=CARTESIAN_POINT('Ctrl Pts',(33.0955022515025,12.5533908099972,-24.7431106901834));
#24933=CARTESIAN_POINT('Ctrl Pts',(33.2417478451207,12.6397562374902,-24.8926999986187));
#24934=CARTESIAN_POINT('Ctrl Pts',(33.3688392455332,12.7143924590826,-25.0219737265016));
#24935=CARTESIAN_POINT('Ctrl Pts',(34.266193218727,13.2413762657968,-25.9347364544968));
#24936=CARTESIAN_POINT('Ctrl Pts',(35.2319960542628,13.7914450399216,-26.887483518938));
#24937=CARTESIAN_POINT('Ctrl Pts',(36.3004607333556,14.3210332302679,-27.8047571717062));
#24938=CARTESIAN_POINT('Ctrl Pts',(36.6891719087154,14.5136992602774,-28.1384645245753));
#24939=CARTESIAN_POINT('Ctrl Pts',(37.0893059759135,14.702405201658,-28.4653128027367));
#24940=CARTESIAN_POINT('Ctrl Pts',(37.5,14.8835914705078,-28.7791366260183));
#24941=CARTESIAN_POINT('',(37.5,12.7626735386834,-29.7804325714888));
#24942=CARTESIAN_POINT('Origin',(37.5,0.,0.));
#24943=CARTESIAN_POINT('',(36.8,11.7911930472673,-29.4900464626661));
#24944=CARTESIAN_POINT('Ctrl Pts',(37.5,12.7626735386834,-29.7804325714888));
#24945=CARTESIAN_POINT('Ctrl Pts',(37.2470086540957,12.4586565616163,-29.6681218786625));
#24946=CARTESIAN_POINT('Ctrl Pts',(37.0122659037829,12.1341821953298,-29.5692859507915));
#24947=CARTESIAN_POINT('Ctrl Pts',(36.8,11.7911930472673,-29.4900464626661));
#24948=CARTESIAN_POINT('',(36.8,4.53355051147313,-31.4347259190859));
#24949=CARTESIAN_POINT('Ctrl Pts',(36.8,11.7911930472673,-29.4900464626661));
#24950=CARTESIAN_POINT('Ctrl Pts',(36.8,9.45611053488411,-30.4236973716148));
#24951=CARTESIAN_POINT('Ctrl Pts',(36.8,7.01967470941751,-31.0761743714062));
#24952=CARTESIAN_POINT('Ctrl Pts',(36.8,4.53355051147313,-31.4347259190859));
#24953=CARTESIAN_POINT('',(37.5,3.83741678103714,-32.1719479119405));
#24954=CARTESIAN_POINT('Ctrl Pts',(36.8,4.53355051147313,-31.4347259190859));
#24955=CARTESIAN_POINT('Ctrl Pts',(37.012265903783,4.27613294009133,-31.6748439028166));
#24956=CARTESIAN_POINT('Ctrl Pts',(37.2470086540957,4.04454785994585,-31.9226755103028));
#24957=CARTESIAN_POINT('Ctrl Pts',(37.5,3.83741678103715,-32.1719479119405));
#24958=CARTESIAN_POINT('',(37.5,1.5,-32.3652591523689));
#24959=CARTESIAN_POINT('Origin',(37.5,0.,0.));
#24960=CARTESIAN_POINT('',(6.9,8.44145532612415,-7.09789564133157));
#24961=CARTESIAN_POINT('Ctrl Pts',(37.5,1.5,-32.3652591523689));
#24962=CARTESIAN_POINT('Ctrl Pts',(36.6490696321407,1.5,-31.6144476510508));
#24963=CARTESIAN_POINT('Ctrl Pts',(35.8406537800942,1.49999999999999,-30.7967681970023));
#24964=CARTESIAN_POINT('Ctrl Pts',(35.0774452370622,1.49999999999999,-29.9676650394963));
#24965=CARTESIAN_POINT('Ctrl Pts',(34.6958409655462,1.49999999999999,-29.5531134607433));
#24966=CARTESIAN_POINT('Ctrl Pts',(34.3255255041725,1.49999999999999,-29.1357262196373));
#24967=CARTESIAN_POINT('Ctrl Pts',(33.9666810635352,1.49999999999999,-28.7225756061873));
#24968=CARTESIAN_POINT('Ctrl Pts',(33.7186145566422,1.49999999999999,-28.4369676438145));
#24969=CARTESIAN_POINT('Ctrl Pts',(33.4671024168586,1.49999999999999,-28.1428784518998));
#24970=CARTESIAN_POINT('Ctrl Pts',(33.2400985609282,1.49999999999999,-27.8754055139288));
#24971=CARTESIAN_POINT('Ctrl Pts',(33.1387264795984,1.49999999999999,-27.7559613383644));
#24972=CARTESIAN_POINT('Ctrl Pts',(33.0532004124087,1.49999999999999,-27.6547707095329));
#24973=CARTESIAN_POINT('Ctrl Pts',(33.,1.49999999999999,-27.5917792275077));
#24974=CARTESIAN_POINT('Ctrl Pts',(32.9185691494976,1.49999999999999,-27.4953617426897));
#24975=CARTESIAN_POINT('Ctrl Pts',(32.8516820633063,1.49973385699142,-27.4160082741233));
#24976=CARTESIAN_POINT('Ctrl Pts',(32.7777321456263,1.49925158146344,-27.3281857859478));
#24977=CARTESIAN_POINT('Ctrl Pts',(32.17886995405,1.49534601146838,-26.6169805623525));
#24978=CARTESIAN_POINT('Ctrl Pts',(31.5692879871895,1.47697823247614,-25.8863210201293));
#24979=CARTESIAN_POINT('Ctrl Pts',(30.9513498041028,1.46858396443303,-25.1628991373263));
#24980=CARTESIAN_POINT('Ctrl Pts',(30.6423807125594,1.46438683041148,-24.8011881959248));
#24981=CARTESIAN_POINT('Ctrl Pts',(30.3347880607298,1.46274142297308,-24.4452439233677));
#24982=CARTESIAN_POINT('Ctrl Pts',(30.024930637208,1.46654496784305,-24.09281706195));
#24983=CARTESIAN_POINT('Ctrl Pts',(29.8700019254471,1.46844674027804,-23.9166036312412));
#24984=CARTESIAN_POINT('Ctrl Pts',(29.7145097313639,1.47171272534061,-23.7412668049999));
#24985=CARTESIAN_POINT('Ctrl Pts',(29.5580100720561,1.47674445496688,-23.5665148172665));
#24986=CARTESIAN_POINT('Ctrl Pts',(29.4797602424023,1.47926031978001,-23.4791388233998));
#24987=CARTESIAN_POINT('Ctrl Pts',(29.4012586241288,1.48221825336111,-23.3919089755878));
#24988=CARTESIAN_POINT('Ctrl Pts',(29.3224502420556,1.48567308535834,-23.3047886331113));
#24989=CARTESIAN_POINT('Ctrl Pts',(29.2736528205877,1.48781228538547,-23.2508445226193));
#24990=CARTESIAN_POINT('Ctrl Pts',(29.224737793671,1.49014206194626,-23.1969423954228));
#24991=CARTESIAN_POINT('Ctrl Pts',(29.1756921968704,1.4926761669178,-23.143073568686));
#24992=CARTESIAN_POINT('Ctrl Pts',(29.1455286056567,1.4942346698506,-23.1099436370539));
#24993=CARTESIAN_POINT('Ctrl Pts',(29.1181490968019,1.49570957236975,-23.0799256031206));
#24994=CARTESIAN_POINT('Ctrl Pts',(29.0849408699094,1.4975930851266,-23.0435998794277));
#24995=CARTESIAN_POINT('Ctrl Pts',(29.0475462330949,1.4997140437585,-23.0026947371893));
#24996=CARTESIAN_POINT('Ctrl Pts',(28.959983740694,1.50462371439458,-22.9072087346982));
#24997=CARTESIAN_POINT('Ctrl Pts',(28.8924081846116,1.50836890094434,-22.8339936857838));
#24998=CARTESIAN_POINT('Ctrl Pts',(28.4410807633312,1.53338246332861,-22.3450009028729));
#24999=CARTESIAN_POINT('Ctrl Pts',(27.9936088565663,1.55654582154998,-21.876105606136));
#25000=CARTESIAN_POINT('Ctrl Pts',(27.5122543093545,1.59544751497299,-21.3913010162073));
#25001=CARTESIAN_POINT('Ctrl Pts',(27.139729410468,1.62555390846788,-21.0161060961865));
#25002=CARTESIAN_POINT('Ctrl Pts',(26.7276341640204,1.66499152477457,-20.612059682844));
#25003=CARTESIAN_POINT('Ctrl Pts',(26.2530417505368,1.74041895661093,-20.1649482705455));
#25004=CARTESIAN_POINT('Ctrl Pts',(25.8694949138893,1.80137642675868,-19.803610493236));
#25005=CARTESIAN_POINT('Ctrl Pts',(25.4447383161208,1.88186126749126,-19.4141244720195));
#25006=CARTESIAN_POINT('Ctrl Pts',(24.9635886608536,1.98732702259108,-18.9908103209483));
#25007=CARTESIAN_POINT('Ctrl Pts',(24.6119820458962,2.06439754885796,-18.6814677825253));
#25008=CARTESIAN_POINT('Ctrl Pts',(24.2873626784783,2.13832395599249,-18.3974053118883));
#25009=CARTESIAN_POINT('Ctrl Pts',(23.6426616415203,2.30363857164967,-17.8679904514206));
#25010=CARTESIAN_POINT('Ctrl Pts',(23.5760533209815,2.32071831602454,-17.8132931069111));
#25011=CARTESIAN_POINT('Ctrl Pts',(23.5065967304281,2.33866955716406,-17.7565376997104));
#25012=CARTESIAN_POINT('Ctrl Pts',(23.4342591639586,2.35752370715749,-17.697767866208));
#25013=CARTESIAN_POINT('Ctrl Pts',(22.7443384436274,2.53734547031001,-17.1372496203964));
#25014=CARTESIAN_POINT('Ctrl Pts',(21.7987837593181,2.82220391184217,-16.3936354357724));
#25015=CARTESIAN_POINT('Ctrl Pts',(20.5610365528855,3.2211816912596,-15.5107287130397));
#25016=CARTESIAN_POINT('Ctrl Pts',(19.7234582214114,3.49116827740818,-14.9132694452422));
#25017=CARTESIAN_POINT('Ctrl Pts',(18.7603809281634,3.83806571370429,-14.2521506387683));
#25018=CARTESIAN_POINT('Ctrl Pts',(17.6514222906382,4.23400473904287,-13.5382422374622));
#25019=CARTESIAN_POINT('Ctrl Pts',(16.7565277906389,4.55351499318665,-12.962140766935));
#25020=CARTESIAN_POINT('Ctrl Pts',(15.7613807992389,4.93854202839548,-12.3388737256115));
#25021=CARTESIAN_POINT('Ctrl Pts',(14.7199652846762,5.32978309078144,-11.7149311743306));
#25022=CARTESIAN_POINT('Ctrl Pts',(13.7316067501733,5.70109160083332,-11.1227766145274));
#25023=CARTESIAN_POINT('Ctrl Pts',(12.7260968661244,6.1045360490248,-10.5273020287043));
#25024=CARTESIAN_POINT('Ctrl Pts',(11.7781012037546,6.47234380217571,-9.97941683016941));
#25025=CARTESIAN_POINT('Ctrl Pts',(10.6475718363527,6.91097182865409,-9.32603798942655));
#25026=CARTESIAN_POINT('Ctrl Pts',(9.62260863652904,7.33414209133672,-8.72329062200738));
#25027=CARTESIAN_POINT('Ctrl Pts',(8.83596460437641,7.64982933055117,-8.26196206072778));
#25028=CARTESIAN_POINT('Ctrl Pts',(8.38131550044628,7.83228405538812,-7.99533241830972));
#25029=CARTESIAN_POINT('Ctrl Pts',(7.99969688490065,7.98693286597114,-7.76911080499006));
#25030=CARTESIAN_POINT('Ctrl Pts',(7.59379043301065,8.15376232312029,-7.52350537407199));
#25031=CARTESIAN_POINT('Ctrl Pts',(7.36145773430516,8.24925215291372,-7.38292575944348));
#25032=CARTESIAN_POINT('Ctrl Pts',(7.13004605045505,8.34517464654957,-7.24116906982106));
#25033=CARTESIAN_POINT('Ctrl Pts',(6.9,8.44145532612415,-7.09789564133157));
#25034=CARTESIAN_POINT('',(6.9,5.6597919716369,-9.46599415782505));
#25035=CARTESIAN_POINT('Ctrl Pts',(6.90000000000001,8.44145532612415,-7.09789564133157));
#25036=CARTESIAN_POINT('Ctrl Pts',(6.90000000000001,8.09681826844945,-7.5077690000137));
#25037=CARTESIAN_POINT('Ctrl Pts',(6.89999999999998,7.72210951819363,-7.89280389060836));
#25038=CARTESIAN_POINT('Ctrl Pts',(6.89999999999998,6.80464666682922,-8.70687723936702));
#25039=CARTESIAN_POINT('Ctrl Pts',(6.90000000000001,6.24868352466685,-9.11389129061079));
#25040=CARTESIAN_POINT('Ctrl Pts',(6.90000000000001,5.6597919716369,-9.46599415782505));
#25041=CARTESIAN_POINT('',(37.5,-1.50000000000001,-32.3652591523689));
#25042=CARTESIAN_POINT('Ctrl Pts',(6.9,5.6597919716369,-9.46599415782505));
#25043=CARTESIAN_POINT('Ctrl Pts',(6.98893730997641,5.61299197171148,-9.50231572683784));
#25044=CARTESIAN_POINT('Ctrl Pts',(7.08052892388333,5.56508220248461,-9.53955640247996));
#25045=CARTESIAN_POINT('Ctrl Pts',(7.17490192378012,5.51603067891051,-9.57777162403489));
#25046=CARTESIAN_POINT('Ctrl Pts',(7.97363347626345,5.10088016320301,-9.90120844679605));
#25047=CARTESIAN_POINT('Ctrl Pts',(8.96286060510633,4.58706675343506,-10.2954119066554));
#25048=CARTESIAN_POINT('Ctrl Pts',(10.2403127965964,4.00248282963831,-10.8024441000946));
#25049=CARTESIAN_POINT('Ctrl Pts',(10.4394276407757,3.91136447885229,-10.8814745615578));
#25050=CARTESIAN_POINT('Ctrl Pts',(10.6449386760798,3.81760465494192,-10.963662030153));
#25051=CARTESIAN_POINT('Ctrl Pts',(10.8572270226597,3.72139879136867,-11.0492678117653));
#25052=CARTESIAN_POINT('Ctrl Pts',(11.0079272578272,3.65310372713856,-11.1100380406946));
#25053=CARTESIAN_POINT('Ctrl Pts',(11.2445718663453,3.54599023597307,-11.2057391108383));
#25054=CARTESIAN_POINT('Ctrl Pts',(11.5512244269296,3.40956688310414,-11.3315975143204));
#25055=CARTESIAN_POINT('Ctrl Pts',(12.0044642698092,3.20792989399308,-11.5176192547245));
#25056=CARTESIAN_POINT('Ctrl Pts',(12.6082461584696,2.94281490464851,-11.7683139216804));
#25057=CARTESIAN_POINT('Ctrl Pts',(13.3027146141536,2.65901005153358,-12.0682094443783));
#25058=CARTESIAN_POINT('Ctrl Pts',(14.2466220416228,2.27326825633123,-12.4758213510422));
#25059=CARTESIAN_POINT('Ctrl Pts',(15.3788107200775,1.81469981617802,-12.9964429751341));
#25060=CARTESIAN_POINT('Ctrl Pts',(16.3720853361384,1.45099516743195,-13.4908337691235));
#25061=CARTESIAN_POINT('Ctrl Pts',(17.5300464833328,1.02698770213283,-14.0671953530332));
#25062=CARTESIAN_POINT('Ctrl Pts',(18.55225712175,0.660939172703652,-14.6297459826175));
#25063=CARTESIAN_POINT('Ctrl Pts',(19.459740928474,0.371242885073749,-15.1671394203612));
#25064=CARTESIAN_POINT('Ctrl Pts',(20.7212139013182,-0.0314574545583951,
-15.9141580365333));
#25065=CARTESIAN_POINT('Ctrl Pts',(21.748318091664,-0.336055810111993,-16.6062803214569));
#25066=CARTESIAN_POINT('Ctrl Pts',(22.5801692622301,-0.547760951425959,
-17.2054151585246));
#25067=CARTESIAN_POINT('Ctrl Pts',(23.3330995243319,-0.739380814663484,
-17.7477077775286));
#25068=CARTESIAN_POINT('Ctrl Pts',(23.9217876528372,-0.87511971474023,-18.2069050138462));
#25069=CARTESIAN_POINT('Ctrl Pts',(24.4822919842876,-0.991018194168117,
-18.6643830118107));
#25070=CARTESIAN_POINT('Ctrl Pts',(24.9418792856086,-1.08604951934922,-19.0394935447735));
#25071=CARTESIAN_POINT('Ctrl Pts',(25.3626276499481,-1.16248493468587,-19.3999270892409));
#25072=CARTESIAN_POINT('Ctrl Pts',(25.7525302890144,-1.22321331868058,-19.7463071016619));
#25073=CARTESIAN_POINT('Ctrl Pts',(26.1776080053149,-1.28942031549629,-20.1239357963656));
#25074=CARTESIAN_POINT('Ctrl Pts',(26.5661459566312,-1.33297321433427,-20.4852396164797));
#25075=CARTESIAN_POINT('Ctrl Pts',(26.9267016824847,-1.36638815227823,-20.831397929128));
#25076=CARTESIAN_POINT('Ctrl Pts',(27.1778777834673,-1.38966620120527,-21.0725442736714));
#25077=CARTESIAN_POINT('Ctrl Pts',(27.4154861110583,-1.40780557004487,-21.3064162454173));
#25078=CARTESIAN_POINT('Ctrl Pts',(27.6422281932782,-1.42326116558415,-21.5339888716807));
#25079=CARTESIAN_POINT('Ctrl Pts',(27.8555559926927,-1.43780239301204,-21.7480980793427));
#25080=CARTESIAN_POINT('Ctrl Pts',(28.1190837187058,-1.45368682611151,-22.0160369607817));
#25081=CARTESIAN_POINT('Ctrl Pts',(28.4603051774444,-1.4725102368991,-22.3749799380264));
#25082=CARTESIAN_POINT('Ctrl Pts',(28.6017730831488,-1.48031428448795,-22.5237950548888));
#25083=CARTESIAN_POINT('Ctrl Pts',(28.754028664589,-1.48853267939111,-22.6856884568469));
#25084=CARTESIAN_POINT('Ctrl Pts',(28.9157341130969,-1.49763121638955,-22.8599017516109));
#25085=CARTESIAN_POINT('Ctrl Pts',(29.4787137469139,-1.52930789194394,-23.4664276157502));
#25086=CARTESIAN_POINT('Ctrl Pts',(30.1711677436051,-1.53976925233501,-24.2477248210474));
#25087=CARTESIAN_POINT('Ctrl Pts',(30.8055547543247,-1.53340754825804,-24.9885333988561));
#25088=CARTESIAN_POINT('Ctrl Pts',(31.1893125644012,-1.52955918190804,-25.4366684846978));
#25089=CARTESIAN_POINT('Ctrl Pts',(31.5650207098714,-1.52122455968006,-25.8828713567533));
#25090=CARTESIAN_POINT('Ctrl Pts',(31.9311744366292,-1.51382648741854,-26.319234664147));
#25091=CARTESIAN_POINT('Ctrl Pts',(32.1142513000081,-1.51012745128778,-26.5374163178438));
#25092=CARTESIAN_POINT('Ctrl Pts',(32.2949430642463,-1.50666813405683,-26.7531357746696));
#25093=CARTESIAN_POINT('Ctrl Pts',(32.4730466959614,-1.50413682057774,-26.9654180603231));
#25094=CARTESIAN_POINT('Ctrl Pts',(32.5932788659635,-1.50242801032152,-27.1087231665209));
#25095=CARTESIAN_POINT('Ctrl Pts',(32.7123311760826,-1.50114220273856,-27.2504621964129));
#25096=CARTESIAN_POINT('Ctrl Pts',(32.8301302693401,-1.50048655910789,-27.3903440144575));
#25097=CARTESIAN_POINT('Ctrl Pts',(32.8868306159707,-1.50017097755206,-27.4576734594568));
#25098=CARTESIAN_POINT('Ctrl Pts',(32.938712302257,-1.5,-27.5192120661652));
#25099=CARTESIAN_POINT('Ctrl Pts',(33.,-1.5,-27.5917792275077));
#25100=CARTESIAN_POINT('Ctrl Pts',(33.0955022515476,-1.5,-27.704857831401));
#25101=CARTESIAN_POINT('Ctrl Pts',(33.2417478452125,-1.5,-27.8775886864422));
#25102=CARTESIAN_POINT('Ctrl Pts',(33.3688392456709,-1.5,-28.0268611296802));
#25103=CARTESIAN_POINT('Ctrl Pts',(34.2661932188112,-1.5,-29.0808287430421));
#25104=CARTESIAN_POINT('Ctrl Pts',(35.2319960542962,-1.50000000000001,-30.1809662912266));
#25105=CARTESIAN_POINT('Ctrl Pts',(36.300460733321,-1.50000000000001,-31.2401426718548));
#25106=CARTESIAN_POINT('Ctrl Pts',(36.6891719086917,-1.50000000000001,-31.6254747318857));
#25107=CARTESIAN_POINT('Ctrl Pts',(37.0893059759013,-1.50000000000001,-32.0028866146587));
#25108=CARTESIAN_POINT('Ctrl Pts',(37.5,-1.50000000000001,-32.3652591523689));
#25109=CARTESIAN_POINT('',(37.5,-3.83741678103716,-32.1719479119405));
#25110=CARTESIAN_POINT('Origin',(37.5,0.,0.));
#25111=CARTESIAN_POINT('',(36.8,-4.53355051147318,-31.4347259190859));
#25112=CARTESIAN_POINT('Ctrl Pts',(37.5,-3.83741678103719,-32.1719479119405));
#25113=CARTESIAN_POINT('Ctrl Pts',(37.2470086540957,-4.04454785994588,-31.9226755103028));
#25114=CARTESIAN_POINT('Ctrl Pts',(37.012265903783,-4.27613294009135,-31.6748439028166));
#25115=CARTESIAN_POINT('Ctrl Pts',(36.8,-4.53355051147316,-31.4347259190859));
#25116=CARTESIAN_POINT('',(36.8,-11.7911930472673,-29.4900464626661));
#25117=CARTESIAN_POINT('Ctrl Pts',(36.8,-4.53355051147318,-31.4347259190859));
#25118=CARTESIAN_POINT('Ctrl Pts',(36.8,-6.18280168905534,-31.1968691126063));
#25119=CARTESIAN_POINT('Ctrl Pts',(36.8,-7.81258162569767,-30.8293258095436));
#25120=CARTESIAN_POINT('Ctrl Pts',(36.8,-10.2137688485759,-30.0846548283827));
#25121=CARTESIAN_POINT('Ctrl Pts',(36.8,-11.0089139056503,-29.8028301128151));
#25122=CARTESIAN_POINT('Ctrl Pts',(36.8,-11.7911930472673,-29.4900464626661));
#25123=CARTESIAN_POINT('',(37.5,-12.7626735386834,-29.7804325714888));
#25124=CARTESIAN_POINT('Ctrl Pts',(36.8,-11.7911930472673,-29.4900464626661));
#25125=CARTESIAN_POINT('Ctrl Pts',(37.0122659037829,-12.1341821953297,-29.5692859507915));
#25126=CARTESIAN_POINT('Ctrl Pts',(37.2470086540956,-12.4586565616162,-29.6681218786625));
#25127=CARTESIAN_POINT('Ctrl Pts',(37.5,-12.7626735386834,-29.7804325714888));
#25128=CARTESIAN_POINT('',(37.5,-14.8835914705078,-28.7791366260183));
#25129=CARTESIAN_POINT('Origin',(37.5,0.,0.));
#25130=CARTESIAN_POINT('',(6.9,3.76156693666918,-10.3676856018661));
#25131=CARTESIAN_POINT('Ctrl Pts',(37.5,-14.8835914705078,-28.7791366260183));
#25132=CARTESIAN_POINT('Ctrl Pts',(36.649069632135,-14.5081857198463,-28.128914792419));
#25133=CARTESIAN_POINT('Ctrl Pts',(35.8406537800833,-14.099345992819,-27.4207836130551));
#25134=CARTESIAN_POINT('Ctrl Pts',(35.0774452370464,-13.6847944140629,-26.7027592162917));
#25135=CARTESIAN_POINT('Ctrl Pts',(34.695840965528,-13.4775186246849,-26.34374701791));
#25136=CARTESIAN_POINT('Ctrl Pts',(34.3255255041519,-13.2688250041304,-25.9822790638941));
#25137=CARTESIAN_POINT('Ctrl Pts',(33.9666810635124,-13.0622496974039,-25.6244801370547));
#25138=CARTESIAN_POINT('Ctrl Pts',(33.7186145566387,-12.9194457162284,-25.3771363861357));
#25139=CARTESIAN_POINT('Ctrl Pts',(33.4671024168778,-12.7724011202845,-25.1224476749824));
#25140=CARTESIAN_POINT('Ctrl Pts',(33.2400985609596,-12.6386646513062,-24.8908093158872));
#25141=CARTESIAN_POINT('Ctrl Pts',(33.1387264796076,-12.578942563511,-24.7873676254918));
#25142=CARTESIAN_POINT('Ctrl Pts',(33.0532004124016,-12.5283472490856,-24.699733970282));
#25143=CARTESIAN_POINT('Ctrl Pts',(33.,-12.4968515080772,-24.6451817466334));
#25144=CARTESIAN_POINT('Ctrl Pts',(32.9185691496442,-12.448642765755,-24.5616817555624));
#25145=CARTESIAN_POINT('Ctrl Pts',(32.8516820633331,-12.4091965180072,-24.4928265642786));
#25146=CARTESIAN_POINT('Ctrl Pts',(32.7777321455747,-12.3657029367323,-24.4165289206501));
#25147=CARTESIAN_POINT('Ctrl Pts',(32.1788699540041,-12.0134826477704,-23.79865434472));
#25148=CARTESIAN_POINT('Ctrl Pts',(31.5692879871508,-11.6640598398815,-23.1567007301491));
#25149=CARTESIAN_POINT('Ctrl Pts',(30.9513498040742,-11.3096185478573,-22.5260018679775));
#25150=CARTESIAN_POINT('Ctrl Pts',(30.6423807125359,-11.1323979018452,-22.2106524368916));
#25151=CARTESIAN_POINT('Ctrl Pts',(30.3347880607108,-10.9558507302104,-21.9015729508113));
#25152=CARTESIAN_POINT('Ctrl Pts',(30.0249306371935,-10.7763433330223,-21.5982641082872));
#25153=CARTESIAN_POINT('Ctrl Pts',(29.8700019254348,-10.6865896344282,-21.4466096870251));
#25154=CARTESIAN_POINT('Ctrl Pts',(29.7145097313539,-10.5960927952763,-21.2963965338147));
#25155=CARTESIAN_POINT('Ctrl Pts',(29.5580100720483,-10.5043591957296,-21.1475727378912));
#25156=CARTESIAN_POINT('Ctrl Pts',(29.4797602423956,-10.4584923959562,-21.0731608399294));
#25157=CARTESIAN_POINT('Ctrl Pts',(29.4012586241233,-10.4123158264269,-20.9990965425476));
#25158=CARTESIAN_POINT('Ctrl Pts',(29.3224502420513,-10.365763682914,-20.9253755287763));
#25159=CARTESIAN_POINT('Ctrl Pts',(29.2736528206688,-10.3369390261512,-20.8797281587992));
#25160=CARTESIAN_POINT('Ctrl Pts',(29.224737793838,-10.3079703169171,-20.8342124356888));
#25161=CARTESIAN_POINT('Ctrl Pts',(29.1756921971237,-10.278841304319,-20.7888277158275));
#25162=CARTESIAN_POINT('Ctrl Pts',(29.1455286058255,-10.2609266353214,-20.7609156047963));
#25163=CARTESIAN_POINT('Ctrl Pts',(29.1181490968943,-10.2446403152596,-20.7356566760271));
#25164=CARTESIAN_POINT('Ctrl Pts',(29.0849408699094,-10.2248462834623,-20.7051394327917));
#25165=CARTESIAN_POINT('Ctrl Pts',(29.0475462332377,-10.2025569083726,-20.670775019915));
#25166=CARTESIAN_POINT('Ctrl Pts',(28.9599837409744,-10.1505620077132,-20.5905365514954));
#25167=CARTESIAN_POINT('Ctrl Pts',(28.8924081850374,-10.1107110566468,-20.5290030526021));
#25168=CARTESIAN_POINT('Ctrl Pts',(28.4410807638263,-9.84455228476247,-20.1180296615806));
#25169=CARTESIAN_POINT('Ctrl Pts',(27.9936088570971,-9.59004457975323,-19.7235361020228));
#25170=CARTESIAN_POINT('Ctrl Pts',(27.5122543100131,-9.3139524301101,-19.3231338580698));
#25171=CARTESIAN_POINT('Ctrl Pts',(27.1397294109546,-9.10028206841989,-19.0132587225486));
#25172=CARTESIAN_POINT('Ctrl Pts',(26.727634164301,-8.86410488405222,-18.6830630722578));
#25173=CARTESIAN_POINT('Ctrl Pts',(26.2530417505368,-8.57522710561968,-18.3335669465969));
#25174=CARTESIAN_POINT('Ctrl Pts',(25.8694949138895,-8.34176749926666,-18.0511179871739));
#25175=CARTESIAN_POINT('Ctrl Pts',(25.4447383161208,-8.07732257196432,-17.7540556187476));
#25176=CARTESIAN_POINT('Ctrl Pts',(24.9635886608529,-7.77432947328252,-17.440187687688));
#25177=CARTESIAN_POINT('Ctrl Pts',(24.6119820458988,-7.552913170443,-17.2108244540782));
#25178=CARTESIAN_POINT('Ctrl Pts',(24.287362678484,-7.34685978853744,-17.0017823418141));
#25179=CARTESIAN_POINT('Ctrl Pts',(23.6426616415357,-6.93898570153371,-16.6259529313418));
#25180=CARTESIAN_POINT('Ctrl Pts',(23.5760533209921,-6.89684553675724,-16.5871235136617));
#25181=CARTESIAN_POINT('Ctrl Pts',(23.5065967304336,-6.85292160229735,-16.5469475097905));
#25182=CARTESIAN_POINT('Ctrl Pts',(23.4342591639586,-6.80720851268155,-16.5054784159948));
#25183=CARTESIAN_POINT('Ctrl Pts',(22.7443384436271,-6.37121917473222,-16.1099662574134));
#25184=CARTESIAN_POINT('Ctrl Pts',(21.7987837593179,-5.75271743557089,-15.6084067036806));
#25185=CARTESIAN_POINT('Ctrl Pts',(20.5610365528855,-4.96573918168374,-15.0432759423309));
#25186=CARTESIAN_POINT('Ctrl Pts',(19.7234582214113,-4.43319430549925,-14.6608543317661));
#25187=CARTESIAN_POINT('Ctrl Pts',(18.7603809281633,-3.80221290992216,-14.2617573685881));
#25188=CARTESIAN_POINT('Ctrl Pts',(17.6514222906382,-3.10236545497629,-13.8414640697512));
#25189=CARTESIAN_POINT('Ctrl Pts',(16.7565277906389,-2.53761072285453,-13.5023006881889));
#25190=CARTESIAN_POINT('Ctrl Pts',(15.7613807992389,-1.89253400855811,-13.1550491146656));
#25191=CARTESIAN_POINT('Ctrl Pts',(14.7199652846762,-1.24173803388781,-12.8103195459473));
#25192=CARTESIAN_POINT('Ctrl Pts',(13.7316067501733,-0.624098151639956,
-12.4831529092169));
#25193=CARTESIAN_POINT('Ctrl Pts',(12.7260968661244,0.0230322824212332,
-12.1691790146817));
#25194=CARTESIAN_POINT('Ctrl Pts',(11.7781012037546,0.61550573962622,-11.8786003909685));
#25195=CARTESIAN_POINT('Ctrl Pts',(10.6475718363526,1.3220581737398,-11.5320717298292));
#25196=CARTESIAN_POINT('Ctrl Pts',(9.62260863652895,1.9899080550587,-11.2216623289213));
#25197=CARTESIAN_POINT('Ctrl Pts',(8.83596460437641,2.49396550450873,-10.9799836949691));
#25198=CARTESIAN_POINT('Ctrl Pts',(8.38131550044784,2.78529075246604,-10.840303013652));
#25199=CARTESIAN_POINT('Ctrl Pts',(7.99969688490338,3.03233135775506,-10.721713754924));
#25200=CARTESIAN_POINT('Ctrl Pts',(7.59379043301429,3.2996126212042,-10.5924279410164));
#25201=CARTESIAN_POINT('Ctrl Pts',(7.36145773430761,3.45259904692339,-10.5184273383902));
#25202=CARTESIAN_POINT('Ctrl Pts',(7.13004605045626,3.60654870801841,-10.4436236908384));
#25203=CARTESIAN_POINT('Ctrl Pts',(6.9,3.76156693666918,-10.3676856018661));
#25204=CARTESIAN_POINT('',(6.9,0.168526548660245,-11.02768739857));
#25205=CARTESIAN_POINT('Ctrl Pts',(6.90000000000001,3.76156693666918,-10.3676856018661));
#25206=CARTESIAN_POINT('Ctrl Pts',(6.90000000000001,3.24481773355662,-10.5551707158657));
#25207=CARTESIAN_POINT('Ctrl Pts',(6.90000000000001,2.71398840242747,-10.7040448708755));
#25208=CARTESIAN_POINT('Ctrl Pts',(6.90000000000001,1.51153848953113,-10.9457448952802));
#25209=CARTESIAN_POINT('Ctrl Pts',(6.90000000000001,0.840414370027659,-11.0174195217678));
#25210=CARTESIAN_POINT('Ctrl Pts',(6.90000000000001,0.168526548660246,-11.02768739857));
#25211=CARTESIAN_POINT('',(37.5,-17.4816676818611,-27.2791366260183));
#25212=CARTESIAN_POINT('Ctrl Pts',(6.9,0.168526548660245,-11.02768739857));
#25213=CARTESIAN_POINT('Ctrl Pts',(6.98893730997555,0.109835775321892,-11.0357428000776));
#25214=CARTESIAN_POINT('Ctrl Pts',(7.08052892388239,0.0497243602609525,
-11.0440392866244));
#25215=CARTESIAN_POINT('Ctrl Pts',(7.17490192378011,-0.01186311602662,-11.0526088775152));
#25216=CARTESIAN_POINT('Ctrl Pts',(7.97363347619349,-0.533112420358449,
-11.1251381246856));
#25217=CARTESIAN_POINT('Ctrl Pts',(8.96286060499838,-1.17518961593372,-11.2096216302935));
#25218=CARTESIAN_POINT('Ctrl Pts',(10.2403127965964,-1.93497024136951,-11.3564324284624));
#25219=CARTESIAN_POINT('Ctrl Pts',(10.4394276407766,-2.05339627863323,-11.3793156403694));
#25220=CARTESIAN_POINT('Ctrl Pts',(10.644938676084,-2.17568840229354,-11.4036121640908));
#25221=CARTESIAN_POINT('Ctrl Pts',(10.85722702267,-2.30180801495081,-11.4296460138921));
#25222=CARTESIAN_POINT('Ctrl Pts',(11.0079272575846,-2.39133838984157,-11.4481270437926));
#25223=CARTESIAN_POINT('Ctrl Pts',(11.2445718661462,-2.53195192937604,-11.4774498561298));
#25224=CARTESIAN_POINT('Ctrl Pts',(11.5512244263538,-2.71302722014986,-11.5182347543375));
#25225=CARTESIAN_POINT('Ctrl Pts',(12.0044642693653,-2.98066084534451,-11.5785158126414));
#25226=CARTESIAN_POINT('Ctrl Pts',(12.6082461582541,-3.33560449465634,-11.663066268173));
#25227=CARTESIAN_POINT('Ctrl Pts',(13.3027146141536,-3.73133446864291,-11.7808809827897));
#25228=CARTESIAN_POINT('Ctrl Pts',(14.2466220417942,-4.26920261601918,-11.9410123512736));
#25229=CARTESIAN_POINT('Ctrl Pts',(15.3788107202222,-4.92664534659587,-12.1625996834269));
#25230=CARTESIAN_POINT('Ctrl Pts',(16.3720853361384,-5.48881820879722,-12.4089023460099));
#25231=CARTESIAN_POINT('Ctrl Pts',(17.5300464833481,-6.14420023710404,-12.6960423867954));
#25232=CARTESIAN_POINT('Ctrl Pts',(18.552257121746,-6.74248287738884,-13.0002012582105));
#25233=CARTESIAN_POINT('Ctrl Pts',(19.459740928474,-7.26206394073252,-13.3207494833101));
#25234=CARTESIAN_POINT('Ctrl Pts',(20.7212139011751,-7.98432197297066,-13.7663364121484));
#25235=CARTESIAN_POINT('Ctrl Pts',(21.7483180914788,-8.5941730292673,-14.2134327155993));
#25236=CARTESIAN_POINT('Ctrl Pts',(22.5801692622301,-9.0770824783983,-14.6264461342272));
#25237=CARTESIAN_POINT('Ctrl Pts',(23.3330995248265,-9.51417645762082,-15.0002753871962));
#25238=CARTESIAN_POINT('Ctrl Pts',(23.9217876541561,-9.86132841201693,-15.330082409639));
#25239=CARTESIAN_POINT('Ctrl Pts',(24.4822919861918,-10.1904384387857,-15.6683207382559));
#25240=CARTESIAN_POINT('Ctrl Pts',(24.9418792867968,-10.4602932466073,-15.9456603260617));
#25241=CARTESIAN_POINT('Ctrl Pts',(25.3626276505146,-10.7067050299032,-16.2195872238973));
#25242=CARTESIAN_POINT('Ctrl Pts',(25.7525302890144,-10.9324873590558,-16.489196921628));
#25243=CARTESIAN_POINT('Ctrl Pts',(26.177608005596,-11.1786386477211,-16.7831294662259));
#25244=CARTESIAN_POINT('Ctrl Pts',(26.5661459571043,-11.3970084746838,-17.0742513036714));
#25245=CARTESIAN_POINT('Ctrl Pts',(26.926701683073,-11.5990258161967,-17.3573257272902));
#25246=CARTESIAN_POINT('Ctrl Pts',(27.1778777841921,-11.7397583702653,-17.5545255633491));
#25247=CARTESIAN_POINT('Ctrl Pts',(27.4154861118762,-11.872403510414,-17.7479949477845));
#25248=CARTESIAN_POINT('Ctrl Pts',(27.6422281941509,-11.9995747619455,-17.9373508256236));
#25249=CARTESIAN_POINT('Ctrl Pts',(27.8555559932678,-12.1192224379658,-18.1155042246928));
#25250=CARTESIAN_POINT('Ctrl Pts',(28.1190837192525,-12.2669482012627,-18.339603886119));
#25251=CARTESIAN_POINT('Ctrl Pts',(28.4603051775732,-12.4627212415744,-18.6410459171623));
#25252=CARTESIAN_POINT('Ctrl Pts',(28.6017730832424,-12.5438873034501,-18.7660215650076));
#25253=CARTESIAN_POINT('Ctrl Pts',(28.7540286646392,-12.631951343169,-18.9021161663187));
#25254=CARTESIAN_POINT('Ctrl Pts',(28.9157341130969,-12.7269375546994,-19.0484400367167));
#25255=CARTESIAN_POINT('Ctrl Pts',(29.4787137469345,-13.0576332925187,-19.557868505355));
#25256=CARTESIAN_POINT('Ctrl Pts',(30.1711677436418,-13.4573416990331,-20.2292610528701));
#25257=CARTESIAN_POINT('Ctrl Pts',(30.8055547543756,-13.8222365906036,-20.874000952648));
#25258=CARTESIAN_POINT('Ctrl Pts',(31.189312564443,-14.0429713504971,-21.2640215044806));
#25259=CARTESIAN_POINT('Ctrl Pts',(31.5650207099043,-14.2588547919394,-21.6546118380272));
#25260=CARTESIAN_POINT('Ctrl Pts',(31.9311744366537,-14.4706295271139,-22.0362125836316));
#25261=CARTESIAN_POINT('Ctrl Pts',(32.1142513000284,-14.5765168947012,-22.2270129564337));
#25262=CARTESIAN_POINT('Ctrl Pts',(32.2949430642625,-14.68138076651,-22.4155611447466));
#25263=CARTESIAN_POINT('Ctrl Pts',(32.4730466959737,-14.7853297275566,-22.6006686536314));
#25264=CARTESIAN_POINT('Ctrl Pts',(32.5932788659582,-14.8555024075531,-22.7256289212004));
#25265=CARTESIAN_POINT('Ctrl Pts',(32.7123311760599,-14.9252583804577,-22.8490214255682));
#25266=CARTESIAN_POINT('Ctrl Pts',(32.8301302693005,-14.99463148543,-22.9704904553205));
#25267=CARTESIAN_POINT('Ctrl Pts',(32.8868306159448,-15.0280229062934,-23.0289572559047));
#25268=CARTESIAN_POINT('Ctrl Pts',(32.9387123022458,-15.0586441387526,-23.0823367414188));
#25269=CARTESIAN_POINT('Ctrl Pts',(33.,-15.0949277194305,-23.1451817466334));
#25270=CARTESIAN_POINT('Ctrl Pts',(33.0955022515125,-15.1514670213565,-23.2431106901936));
#25271=CARTESIAN_POINT('Ctrl Pts',(33.2417478451615,-15.2378324488677,-23.3926999986605));
#25272=CARTESIAN_POINT('Ctrl Pts',(33.3688392455996,-15.3124686704749,-23.5219737265691));
#25273=CARTESIAN_POINT('Ctrl Pts',(34.2661932188049,-15.8394524771949,-24.4347364545743));
#25274=CARTESIAN_POINT('Ctrl Pts',(35.2319960543609,-16.3895212513289,-25.3874835190315));
#25275=CARTESIAN_POINT('Ctrl Pts',(36.3004607334728,-16.9191094416793,-26.3047571718069));
#25276=CARTESIAN_POINT('Ctrl Pts',(36.6891719087959,-17.1117754716687,-26.638464524641));
#25277=CARTESIAN_POINT('Ctrl Pts',(37.0893059759547,-17.3004814130296,-26.9653128027682));
#25278=CARTESIAN_POINT('Ctrl Pts',(37.5,-17.4816676818611,-27.2791366260183));
#25279=CARTESIAN_POINT('',(37.5,-19.4092743732572,-25.9430157904516));
#25280=CARTESIAN_POINT('Origin',(37.5,0.,0.));
#25281=CARTESIAN_POINT('',(36.8,-19.6435328718186,-24.9564959511929));
#25282=CARTESIAN_POINT('Ctrl Pts',(37.5,-19.4092743732572,-25.9430157904516));
#25283=CARTESIAN_POINT('Ctrl Pts',(37.2470086540957,-19.4640189486865,-25.6235740187167));
#25284=CARTESIAN_POINT('Ctrl Pts',(37.0122659037829,-19.5406617074869,-25.2931530107001));
#25285=CARTESIAN_POINT('Ctrl Pts',(36.8,-19.6435328718186,-24.9564959511929));
#25286=CARTESIAN_POINT('',(36.8,-24.9564959511929,-19.6435328718186));
#25287=CARTESIAN_POINT('Ctrl Pts',(36.8,-19.6435328718186,-24.9564959511929));
#25288=CARTESIAN_POINT('Ctrl Pts',(36.8,-20.2288646216318,-24.4957748831848));
#25289=CARTESIAN_POINT('Ctrl Pts',(36.8,-20.7984186457787,-24.0141222843114));
#25290=CARTESIAN_POINT('Ctrl Pts',(36.8,-22.6602579716864,-22.3234241559746));
#25291=CARTESIAN_POINT('Ctrl Pts',(36.8,-23.8659348286794,-21.029056769996));
#25292=CARTESIAN_POINT('Ctrl Pts',(36.8,-24.9564959511929,-19.6435328718186));
#25293=CARTESIAN_POINT('',(37.5,-25.9430157904517,-19.4092743732571));
#25294=CARTESIAN_POINT('Ctrl Pts',(36.8,-24.9564959511929,-19.6435328718186));
#25295=CARTESIAN_POINT('Ctrl Pts',(37.0122659037829,-25.2931530107001,-19.5406617074869));
#25296=CARTESIAN_POINT('Ctrl Pts',(37.2470086540956,-25.6235740187166,-19.4640189486865));
#25297=CARTESIAN_POINT('Ctrl Pts',(37.5,-25.9430157904516,-19.4092743732572));
#25298=CARTESIAN_POINT('',(37.5,-27.2791366260183,-17.4816676818611));
#25299=CARTESIAN_POINT('Origin',(37.5,0.,0.));
#25300=CARTESIAN_POINT('',(6.9,-1.92623027574191,-10.8594625780008));
#25301=CARTESIAN_POINT('Ctrl Pts',(37.5,-27.2791366260183,-17.4816676818611));
#25302=CARTESIAN_POINT('Ctrl Pts',(36.6490696321363,-26.62891479242,-17.1062619312002));
#25303=CARTESIAN_POINT('Ctrl Pts',(35.840653780086,-25.9207836130574,-16.6974222041736));
#25304=CARTESIAN_POINT('Ctrl Pts',(35.0774452370509,-25.2027592162959,-16.2828706254186));
#25305=CARTESIAN_POINT('Ctrl Pts',(34.6958409655333,-24.8437470179151,-16.0755948360411));
#25306=CARTESIAN_POINT('Ctrl Pts',(34.3255255041583,-24.4822790639003,-15.8669012154872));
#25307=CARTESIAN_POINT('Ctrl Pts',(33.9666810635198,-24.1244801370621,-15.6603259087614));
#25308=CARTESIAN_POINT('Ctrl Pts',(33.7186145566397,-23.8771363861367,-15.5175219275823));
#25309=CARTESIAN_POINT('Ctrl Pts',(33.4671024168716,-23.6224476749761,-15.3704773316342));
#25310=CARTESIAN_POINT('Ctrl Pts',(33.240098560949,-23.3908093158764,-15.2367408626533));
#25311=CARTESIAN_POINT('Ctrl Pts',(33.1387264796047,-23.2873676254888,-15.1770187748626));
#25312=CARTESIAN_POINT('Ctrl Pts',(33.0532004124041,-23.1997339702846,-15.1264234604404));
#25313=CARTESIAN_POINT('Ctrl Pts',(33.,-23.1451817466334,-15.0949277194305));
#25314=CARTESIAN_POINT('Ctrl Pts',(32.9185691495912,-23.0616817555081,-15.0467189770769));
#25315=CARTESIAN_POINT('Ctrl Pts',(32.8516820633262,-22.9930927072798,-15.0068117561438));
#25316=CARTESIAN_POINT('Ctrl Pts',(32.7777321455979,-22.9172773392108,-14.9624828491682));
#25317=CARTESIAN_POINT('Ctrl Pts',(32.178869954022,-22.303308333271,-14.6034979145383));
#25318=CARTESIAN_POINT('Ctrl Pts',(31.5692879871635,-21.6797224976866,-14.2222611802097));
#25319=CARTESIAN_POINT('Ctrl Pts',(30.9513498040836,-21.0574179035543,-13.8532805894412));
#25320=CARTESIAN_POINT('Ctrl Pts',(30.6423807125436,-20.7462656064881,-13.6687902940569));
#25321=CARTESIAN_POINT('Ctrl Pts',(30.3347880607171,-20.4388315278445,-13.4893931931391));
#25322=CARTESIAN_POINT('Ctrl Pts',(30.0249306371985,-20.1317191404489,-13.316473728914));
#25323=CARTESIAN_POINT('Ctrl Pts',(29.8700019254392,-19.9781629467512,-13.2300139968015));
#25324=CARTESIAN_POINT('Ctrl Pts',(29.7145097313576,-19.8246838084775,-13.1451740097143));
#25325=CARTESIAN_POINT('Ctrl Pts',(29.5580100720514,-19.6708282829271,-13.0621556215299));
#25326=CARTESIAN_POINT('Ctrl Pts',(29.4797602423983,-19.5939005201519,-13.0206464274377));
#25327=CARTESIAN_POINT('Ctrl Pts',(29.4012586241258,-19.5168782891887,-12.979593149156));
#25328=CARTESIAN_POINT('Ctrl Pts',(29.3224502420534,-19.4397024434199,-12.9390249501936));
#25329=CARTESIAN_POINT('Ctrl Pts',(29.2736528205548,-19.3919158733057,-12.9139054964992));
#25330=CARTESIAN_POINT('Ctrl Pts',(29.2247377936074,-19.3440703735249,-12.8889720785721));
#25331=CARTESIAN_POINT('Ctrl Pts',(29.1756921967758,-19.2961515485829,-12.8642322644697));
#25332=CARTESIAN_POINT('Ctrl Pts',(29.1455286055936,-19.2666809347284,-12.8490170018014));
#25333=CARTESIAN_POINT('Ctrl Pts',(29.1181490967682,-19.2399471035395,-12.8352852878993));
#25334=CARTESIAN_POINT('Ctrl Pts',(29.0849408699094,-19.2075463476651,-12.8187535959654));
#25335=CARTESIAN_POINT('Ctrl Pts',(29.0475462330809,-19.1710609760116,-12.8001378288948));
#25336=CARTESIAN_POINT('Ctrl Pts',(28.9599837407005,-19.0859128368506,-12.7566467271546));
#25337=CARTESIAN_POINT('Ctrl Pts',(28.8924081846425,-19.0206341513,-12.7232826294034));
#25338=CARTESIAN_POINT('Ctrl Pts',(28.4410807633615,-18.5846471978384,-12.5004486184112));
#25339=CARTESIAN_POINT('Ctrl Pts',(27.9936088565974,-18.1669902800388,-12.2860610266994));
#25340=CARTESIAN_POINT('Ctrl Pts',(27.5122543093923,-17.7276863425835,-12.0773485864914));
#25341=CARTESIAN_POINT('Ctrl Pts',(27.1397294104949,-17.3877048137166,-11.9158240280583));
#25342=CARTESIAN_POINT('Ctrl Pts',(26.7276341640354,-17.0180715472901,-11.7479547989676));
#25343=CARTESIAN_POINT('Ctrl Pts',(26.2530417505368,-16.593147989986,-11.5897211649258));
#25344=CARTESIAN_POINT('Ctrl Pts',(25.8694949138867,-16.2497415604127,-11.4618429939686));
#25345=CARTESIAN_POINT('Ctrl Pts',(25.4447383161154,-15.8721943512516,-11.3368019000536));
#25346=CARTESIAN_POINT('Ctrl Pts',(24.9635886608448,-15.4528606650898,-11.2164808476631));
#25347=CARTESIAN_POINT('Ctrl Pts',(24.6119820459015,-15.1464269052232,-11.1285546120855));
#25348=CARTESIAN_POINT('Ctrl Pts',(24.2873626784964,-14.8634583858341,-11.0505455233595));
#25349=CARTESIAN_POINT('Ctrl Pts',(23.642661641582,-14.3223143597349,-10.9290047499082));
#25350=CARTESIAN_POINT('Ctrl Pts',(23.5760533210243,-14.2664051976669,-10.9164475701686));
#25351=CARTESIAN_POINT('Ctrl Pts',(23.5065967304504,-14.2082779526419,-10.9036160974206));
#25352=CARTESIAN_POINT('Ctrl Pts',(23.4342591639586,-14.1479547088373,-10.8905593535264));
#25353=CARTESIAN_POINT('Ctrl Pts',(22.7443384436266,-13.5726207871028,-10.7660304456639));
#25354=CARTESIAN_POINT('Ctrl Pts',(21.7987837593173,-12.7862027918379,-10.6409180002012));
#25355=CARTESIAN_POINT('Ctrl Pts',(20.5610365528854,-11.8220942510713,-10.544989531356));
#25356=CARTESIAN_POINT('Ctrl Pts',(19.7234582214112,-11.1696860543578,-10.480075139743));
#25357=CARTESIAN_POINT('Ctrl Pts',(18.7603809281633,-10.4236916548837,-10.4499377288461));
#25358=CARTESIAN_POINT('Ctrl Pts',(17.6514222906382,-9.60745933070834,-10.435876782486));
#25359=CARTESIAN_POINT('Ctrl Pts',(16.7565277906389,-8.94878569500228,-10.4245300440805));
#25360=CARTESIAN_POINT('Ctrl Pts',(15.7613807992389,-8.21650708627012,-10.4463397170534));
#25361=CARTESIAN_POINT('Ctrl Pts',(14.7199652846762,-7.48053645516581,-10.4731931404428));
#25362=CARTESIAN_POINT('Ctrl Pts',(13.7316067501733,-6.78206130838354,-10.4986784628874));
#25363=CARTESIAN_POINT('Ctrl Pts',(12.7260968661244,-6.06464296565695,-10.5503343111255));
#25364=CARTESIAN_POINT('Ctrl Pts',(11.7781012037546,-5.40625658879283,-10.5949225697956));
#25365=CARTESIAN_POINT('Ctrl Pts',(10.6475718363526,-4.62109990117505,-10.6480961631663));
#25366=CARTESIAN_POINT('Ctrl Pts',(9.62260863652896,-3.88752023758453,-10.713198677066));
#25367=CARTESIAN_POINT('Ctrl Pts',(8.83596460437642,-3.33015436441791,-10.7559275652365));
#25368=CARTESIAN_POINT('Ctrl Pts',(8.38131550044705,-3.00801895826399,-10.7806231707767));
#25369=CARTESIAN_POINT('Ctrl Pts',(7.99969688490205,-2.734780888953,-10.8014421627468));
#25370=CARTESIAN_POINT('Ctrl Pts',(7.59379043301258,-2.43866561789635,-10.8231179952785));
#25371=CARTESIAN_POINT('Ctrl Pts',(7.36145773430645,-2.26917518547666,-10.8355248063684));
#25372=CARTESIAN_POINT('Ctrl Pts',(7.13004605045568,-2.09844904428886,-10.8477177778403));
#25373=CARTESIAN_POINT('Ctrl Pts',(6.9,-1.9262302757419,-10.8594625780008));
#25374=CARTESIAN_POINT('',(6.9,-5.36789542693312,-9.6345207064853));
#25375=CARTESIAN_POINT('Ctrl Pts',(6.90000000000001,-1.92623027574191,-10.8594625780008));
#25376=CARTESIAN_POINT('Ctrl Pts',(6.90000000000001,-2.35749364924904,-10.7829659225815));
#25377=CARTESIAN_POINT('Ctrl Pts',(6.90000000000001,-2.78469328079872,-10.6806923192591));
#25378=CARTESIAN_POINT('Ctrl Pts',(6.90000000000001,-3.958690010018,-10.3240838050858));
#25379=CARTESIAN_POINT('Ctrl Pts',(6.90000000000001,-4.68344446130229,-10.0158641401962));
#25380=CARTESIAN_POINT('Ctrl Pts',(6.90000000000001,-5.36789542693313,-9.6345207064853));
#25381=CARTESIAN_POINT('',(37.5,-28.7791366260183,-14.8835914705078));
#25382=CARTESIAN_POINT('Ctrl Pts',(6.9,-5.36789542693312,-9.6345207064853));
#25383=CARTESIAN_POINT('Ctrl Pts',(6.98893730997566,-5.42275082836576,-9.61215150215935));
#25384=CARTESIAN_POINT('Ctrl Pts',(7.08052892388251,-5.47895708413934,-9.58928076274051));
#25385=CARTESIAN_POINT('Ctrl Pts',(7.17490192378012,-5.5365781986047,-9.56590850800827));
#25386=CARTESIAN_POINT('Ctrl Pts',(7.97363347620185,-6.02425796145133,-9.36809602640721));
#25387=CARTESIAN_POINT('Ctrl Pts',(8.9628606050108,-6.62255487681613,-9.12022229067638));
#25388=CARTESIAN_POINT('Ctrl Pts',(10.2403127965964,-7.35394959882411,-8.86747385872511));
#25389=CARTESIAN_POINT('Ctrl Pts',(10.4394276407787,-7.46795116151874,-8.82807828292446));
#25390=CARTESIAN_POINT('Ctrl Pts',(10.6449386760882,-7.58600750915316,-8.78797362786027));
#25391=CARTESIAN_POINT('Ctrl Pts',(10.8572270226761,-7.70824722253153,-8.74745979681753));
#25392=CARTESIAN_POINT('Ctrl Pts',(11.0079272576205,-7.7950233165647,-8.71869965074842));
#25393=CARTESIAN_POINT('Ctrl Pts',(11.2445718661789,-7.93145962008442,-8.67378718137609));
#25394=CARTESIAN_POINT('Ctrl Pts',(11.5512244264302,-8.10866787102136,-8.61857029392041));
#25395=CARTESIAN_POINT('Ctrl Pts',(12.004464269425,-8.37058591848924,-8.5369584091849));
#25396=CARTESIAN_POINT('Ctrl Pts',(12.6082461582835,-8.72025136345347,-8.43270942692696));
#25397=CARTESIAN_POINT('Ctrl Pts',(13.3027146141536,-9.12187093125612,-8.33687497573541));
#25398=CARTESIAN_POINT('Ctrl Pts',(14.2466220417731,-9.66774409500015,-8.20661873509998));
#25399=CARTESIAN_POINT('Ctrl Pts',(15.3788107202044,-10.3478998672909,-8.06979762861151));
#25400=CARTESIAN_POINT('Ctrl Pts',(16.3720853361384,-10.9579071785779,-8.00201556032625));
#25401=CARTESIAN_POINT('Ctrl Pts',(17.5300464833461,-11.6690546846669,-7.92299511593695));
#25402=CARTESIAN_POINT('Ctrl Pts',(18.5522571217463,-12.3392620855058,-7.88726310522631));
#25403=CARTESIAN_POINT('Ctrl Pts',(19.459740928474,-12.9495065982363,-7.9050754796287));
#25404=CARTESIAN_POINT('Ctrl Pts',(20.7212139011916,-13.7977938666722,-7.92983606347819));
#25405=CARTESIAN_POINT('Ctrl Pts',(21.7483180915005,-14.5494885256804,-8.01210729205923));
#25406=CARTESIAN_POINT('Ctrl Pts',(22.5801692622301,-15.1742070856531,-8.12833268012627));
#25407=CARTESIAN_POINT('Ctrl Pts',(23.3330995247701,-15.7396562019433,-8.23353132025611));
#25408=CARTESIAN_POINT('Ctrl Pts',(23.9217876540031,-16.2052021245672,-8.34557660281974));
#25409=CARTESIAN_POINT('Ctrl Pts',(24.4822919859706,-16.6593389326385,-8.47394457452865));
#25410=CARTESIAN_POINT('Ctrl Pts',(24.9418792866585,-17.0317098455124,-8.57920029914614));
#25411=CARTESIAN_POINT('Ctrl Pts',(25.3626276504486,-17.3820721586154,-8.69322205982058));
#25412=CARTESIAN_POINT('Ctrl Pts',(25.7525302890143,-17.7124102403086,-8.81381974260611));
#25413=CARTESIAN_POINT('Ctrl Pts',(26.1776080055599,-18.0725497817353,-8.94529714888304));
#25414=CARTESIAN_POINT('Ctrl Pts',(26.5661459570434,-18.4072245180059,-9.08823114221459));
#25415=CARTESIAN_POINT('Ctrl Pts',(26.9267016829969,-18.7237138795562,-9.23237211346577));
#25416=CARTESIAN_POINT('Ctrl Pts',(27.1778777840957,-18.94419176453,-9.33278590407112));
#25417=CARTESIAN_POINT('Ctrl Pts',(27.4154861117651,-19.1558005177911,-9.43401273576453));
#25418=CARTESIAN_POINT('Ctrl Pts',(27.6422281940302,-19.3606119911582,-9.5344141105576));
#25419=CARTESIAN_POINT('Ctrl Pts',(27.8555559931903,-19.5533066176682,-9.62887564192972));
#25420=CARTESIAN_POINT('Ctrl Pts',(28.1190837191777,-19.7932907121909,-9.74908876005587));
#25421=CARTESIAN_POINT('Ctrl Pts',(28.4603051775583,-20.1135561540545,-9.91225869658039));
#25422=CARTESIAN_POINT('Ctrl Pts',(28.6017730832314,-20.2463358494903,-9.97990775153286));
#25423=CARTESIAN_POINT('Ctrl Pts',(28.7540286646333,-20.3906488457069,-10.0537371137291));
#25424=CARTESIAN_POINT('Ctrl Pts',(28.9157341130969,-20.5460712531062,-10.1329641969115));
#25425=CARTESIAN_POINT('Ctrl Pts',(29.4787137469313,-21.0871763972971,-10.4087943232522));
#25426=CARTESIAN_POINT('Ctrl Pts',(30.171167743637,-21.7690303052006,-10.7903831220533));
#25427=CARTESIAN_POINT('Ctrl Pts',(30.8055547543696,-22.4074085008994,-11.1662968083083));
#25428=CARTESIAN_POINT('Ctrl Pts',(31.1893125644379,-22.7935806863826,-11.3936971342472));
#25429=CARTESIAN_POINT('Ctrl Pts',(31.5650207099002,-23.1758363977024,-11.6240165648506));
#25430=CARTESIAN_POINT('Ctrl Pts',(31.9311744366506,-23.5500390710465,-11.8486051370604));
#25431=CARTESIAN_POINT('Ctrl Pts',(32.1142513000258,-23.7371404077185,-11.9608994231653));
#25432=CARTESIAN_POINT('Ctrl Pts',(32.2949430642605,-23.9222292788011,-12.0717550081777));
#25433=CARTESIAN_POINT('Ctrl Pts',(32.4730466959721,-24.1048054742075,-12.1800883327802));
#25434=CARTESIAN_POINT('Ctrl Pts',(32.593278865964,-24.2280569315281,-12.253220758965));
#25435=CARTESIAN_POINT('Ctrl Pts',(32.712331176073,-24.3501636283205,-12.3252038159361));
#25436=CARTESIAN_POINT('Ctrl Pts',(32.8301302693206,-24.4709770144493,-12.3957125289926));
#25437=CARTESIAN_POINT('Ctrl Pts',(32.8868306159582,-24.5291282334706,-12.4296505531408));
#25438=CARTESIAN_POINT('Ctrl Pts',(32.9387123022532,-24.5823367414265,-12.4605679274037));
#25439=CARTESIAN_POINT('Ctrl Pts',(33.,-24.6451817466334,-12.4968515080772));
#25440=CARTESIAN_POINT('Ctrl Pts',(33.0955022515533,-24.7431106902355,-12.5533908100273));
#25441=CARTESIAN_POINT('Ctrl Pts',(33.2417478451922,-24.8926999986918,-12.6397562375324));
#25442=CARTESIAN_POINT('Ctrl Pts',(33.3688392456331,-25.0219737266032,-12.7143924591412));
#25443=CARTESIAN_POINT('Ctrl Pts',(34.266193218824,-25.934736454593,-13.2413762658524));
#25444=CARTESIAN_POINT('Ctrl Pts',(35.231996054366,-26.8874835190347,-13.7914450399775));
#25445=CARTESIAN_POINT('Ctrl Pts',(36.3004607334594,-27.8047571717954,-14.3210332303193));
#25446=CARTESIAN_POINT('Ctrl Pts',(36.6891719087867,-28.1384645246335,-14.513699260311));
#25447=CARTESIAN_POINT('Ctrl Pts',(37.08930597595,-28.4653128027646,-14.7024052016742));
#25448=CARTESIAN_POINT('Ctrl Pts',(37.5,-28.7791366260183,-14.8835914705078));
#25449=CARTESIAN_POINT('',(37.5,-29.7804325714888,-12.7626735386834));
#25450=CARTESIAN_POINT('Origin',(37.5,0.,0.));
#25451=CARTESIAN_POINT('',(36.8,-29.4900464626661,-11.7911930472673));
#25452=CARTESIAN_POINT('Ctrl Pts',(37.5,-29.7804325714888,-12.7626735386834));
#25453=CARTESIAN_POINT('Ctrl Pts',(37.2470086540956,-29.6681218786625,-12.4586565616162));
#25454=CARTESIAN_POINT('Ctrl Pts',(37.0122659037829,-29.5692859507915,-12.1341821953297));
#25455=CARTESIAN_POINT('Ctrl Pts',(36.8,-29.4900464626661,-11.7911930472673));
#25456=CARTESIAN_POINT('',(36.8,-31.4347259190859,-4.53355051147314));
#25457=CARTESIAN_POINT('Ctrl Pts',(36.8,-29.4900464626661,-11.7911930472673));
#25458=CARTESIAN_POINT('Ctrl Pts',(36.8,-30.4236973716148,-9.45611053488413));
#25459=CARTESIAN_POINT('Ctrl Pts',(36.8,-31.0761743714062,-7.01967470941752));
#25460=CARTESIAN_POINT('Ctrl Pts',(36.8,-31.4347259190859,-4.53355051147314));
#25461=CARTESIAN_POINT('',(37.5,-32.1719479119405,-3.83741678103714));
#25462=CARTESIAN_POINT('Ctrl Pts',(36.8,-31.4347259190859,-4.53355051147314));
#25463=CARTESIAN_POINT('Ctrl Pts',(37.0122659037829,-31.6748439028166,-4.27613294009137));
#25464=CARTESIAN_POINT('Ctrl Pts',(37.2470086540956,-31.9226755103028,-4.04454785994591));
#25465=CARTESIAN_POINT('Ctrl Pts',(37.5,-32.1719479119405,-3.83741678103716));
#25466=CARTESIAN_POINT('',(37.5,-32.3652591523689,-1.5));
#25467=CARTESIAN_POINT('Origin',(37.5,0.,0.));
#25468=CARTESIAN_POINT('',(6.9,-7.09789564133157,-8.44145532612415));
#25469=CARTESIAN_POINT('Ctrl Pts',(37.5,-32.3652591523689,-1.5));
#25470=CARTESIAN_POINT('Ctrl Pts',(36.6490696321457,-31.6144476510553,-1.5));
#25471=CARTESIAN_POINT('Ctrl Pts',(35.8406537801031,-30.7967681970114,-1.49999999999999));
#25472=CARTESIAN_POINT('Ctrl Pts',(35.0774452370724,-29.9676650395074,-1.49999999999999));
#25473=CARTESIAN_POINT('Ctrl Pts',(34.6958409655571,-29.5531134607554,-1.49999999999999));
#25474=CARTESIAN_POINT('Ctrl Pts',(34.3255255041835,-29.1357262196498,-1.5));
#25475=CARTESIAN_POINT('Ctrl Pts',(33.9666810635455,-28.7225756061991,-1.5));
#25476=CARTESIAN_POINT('Ctrl Pts',(33.7186145566592,-28.4369676438341,-1.5));
#25477=CARTESIAN_POINT('Ctrl Pts',(33.4671024168883,-28.1428784519347,-1.5));
#25478=CARTESIAN_POINT('Ctrl Pts',(33.2400985609549,-27.8754055139602,-1.5));
#25479=CARTESIAN_POINT('Ctrl Pts',(33.1387264796142,-27.7559613383832,-1.5));
#25480=CARTESIAN_POINT('Ctrl Pts',(33.0532004124121,-27.6547707095369,-1.5));
#25481=CARTESIAN_POINT('Ctrl Pts',(33.,-27.5917792275077,-1.5));
#25482=CARTESIAN_POINT('Ctrl Pts',(32.9185691495509,-27.4953617427528,-1.5));
#25483=CARTESIAN_POINT('Ctrl Pts',(32.8516820632998,-27.4160082741156,-1.49973385699148));
#25484=CARTESIAN_POINT('Ctrl Pts',(32.7777321455762,-27.3281857858883,-1.49925158146312));
#25485=CARTESIAN_POINT('Ctrl Pts',(32.1788699540068,-26.6169805623009,-1.49534601146731));
#25486=CARTESIAN_POINT('Ctrl Pts',(31.5692879871545,-25.8863210200878,-1.47697823247537));
#25487=CARTESIAN_POINT('Ctrl Pts',(30.9513498040757,-25.1628991372947,-1.46858396443267));
#25488=CARTESIAN_POINT('Ctrl Pts',(30.6423807125364,-24.8011881958981,-1.46438683041132));
#25489=CARTESIAN_POINT('Ctrl Pts',(30.3347880607112,-24.4452439233464,-1.46274142297315));
#25490=CARTESIAN_POINT('Ctrl Pts',(30.024930637194,-24.0928170619341,-1.46654496784322));
#25491=CARTESIAN_POINT('Ctrl Pts',(29.8700019254354,-23.916603631228,-1.46844674027826));
#25492=CARTESIAN_POINT('Ctrl Pts',(29.7145097313546,-23.7412668049894,-1.47171272534086));
#25493=CARTESIAN_POINT('Ctrl Pts',(29.5580100720492,-23.5665148172587,-1.47674445496711));
#25494=CARTESIAN_POINT('Ctrl Pts',(29.4797602423965,-23.4791388233934,-1.47926031978023));
#25495=CARTESIAN_POINT('Ctrl Pts',(29.4012586241243,-23.3919089755827,-1.4822182533613));
#25496=CARTESIAN_POINT('Ctrl Pts',(29.3224502420522,-23.3047886331076,-1.48567308535849));
#25497=CARTESIAN_POINT('Ctrl Pts',(29.2736528206287,-23.2508445226647,-1.48781228538369));
#25498=CARTESIAN_POINT('Ctrl Pts',(29.2247377937566,-23.196942395517,-1.49014206194219));
#25499=CARTESIAN_POINT('Ctrl Pts',(29.1756921970008,-23.1430735688292,-1.49267616691107));
#25500=CARTESIAN_POINT('Ctrl Pts',(29.1455286057438,-23.1099436371495,-1.49423466984589));
#25501=CARTESIAN_POINT('Ctrl Pts',(29.1181490968576,-23.0799256031815,-1.49570957236661));
#25502=CARTESIAN_POINT('Ctrl Pts',(29.0849408699095,-23.0435998794277,-1.49759308512661));
#25503=CARTESIAN_POINT('Ctrl Pts',(29.04754623316,-23.0026947372604,-1.49971404375482));
#25504=CARTESIAN_POINT('Ctrl Pts',(28.9599837408029,-22.9072087348169,-1.50462371438851));
#25505=CARTESIAN_POINT('Ctrl Pts',(28.892408184771,-22.8339936859565,-1.50836890093551));
#25506=CARTESIAN_POINT('Ctrl Pts',(28.4410807635607,-22.3450009031177,-1.53338246331615));
#25507=CARTESIAN_POINT('Ctrl Pts',(27.9936088568423,-21.876105606424,-1.55654582153512));
#25508=CARTESIAN_POINT('Ctrl Pts',(27.5122543097379,-21.3913010165935,-1.595447514942));
#25509=CARTESIAN_POINT('Ctrl Pts',(27.1397294107505,-21.0161060964632,-1.62555390843929));
#25510=CARTESIAN_POINT('Ctrl Pts',(26.727634164183,-20.6120596829972,-1.66499152474874));
#25511=CARTESIAN_POINT('Ctrl Pts',(26.2530417505368,-20.1649482705455,-1.74041895661093));
#25512=CARTESIAN_POINT('Ctrl Pts',(25.8694949138871,-19.8036104932339,-1.80137642675904));
#25513=CARTESIAN_POINT('Ctrl Pts',(25.444738316116,-19.4141244720151,-1.88186126749218));
#25514=CARTESIAN_POINT('Ctrl Pts',(24.9635886608454,-18.9908103209411,-1.98732702259288));
#25515=CARTESIAN_POINT('Ctrl Pts',(24.61198204591,-18.6814677825376,-2.06439754885504));
#25516=CARTESIAN_POINT('Ctrl Pts',(24.2873626785129,-18.3974053119194,-2.13832395598498));
#25517=CARTESIAN_POINT('Ctrl Pts',(23.6426616416205,-17.8679904515028,-2.30363857162399));
#25518=CARTESIAN_POINT('Ctrl Pts',(23.5760533210511,-17.813293106968,-2.32071831600655));
#25519=CARTESIAN_POINT('Ctrl Pts',(23.5065967304643,-17.7565376997399,-2.33866955715462));
#25520=CARTESIAN_POINT('Ctrl Pts',(23.4342591639586,-17.697767866208,-2.35752370715749));
#25521=CARTESIAN_POINT('Ctrl Pts',(22.7443384436261,-17.1372496203954,-2.53734547031035));
#25522=CARTESIAN_POINT('Ctrl Pts',(21.7987837593168,-16.3936354357714,-2.82220391184259));
#25523=CARTESIAN_POINT('Ctrl Pts',(20.5610365528854,-15.5107287130397,-3.2211816912596));
#25524=CARTESIAN_POINT('Ctrl Pts',(19.7234582214111,-14.913269445242,-3.49116827740827));
#25525=CARTESIAN_POINT('Ctrl Pts',(18.7603809281631,-14.2521506387681,-3.83806571370439));
#25526=CARTESIAN_POINT('Ctrl Pts',(17.6514222906382,-13.5382422374622,-4.23400473904287));
#25527=CARTESIAN_POINT('Ctrl Pts',(16.7565277906389,-12.962140766935,-4.55351499318666));
#25528=CARTESIAN_POINT('Ctrl Pts',(15.7613807992389,-12.3388737256115,-4.93854202839547));
#25529=CARTESIAN_POINT('Ctrl Pts',(14.7199652846762,-11.7149311743306,-5.32978309078144));
#25530=CARTESIAN_POINT('Ctrl Pts',(13.7316067501733,-11.1227766145274,-5.70109160083331));
#25531=CARTESIAN_POINT('Ctrl Pts',(12.7260968661244,-10.5273020287043,-6.1045360490248));
#25532=CARTESIAN_POINT('Ctrl Pts',(11.7781012037546,-9.97941683016941,-6.47234380217571));
#25533=CARTESIAN_POINT('Ctrl Pts',(10.6475718363527,-9.32603798942654,-6.91097182865409));
#25534=CARTESIAN_POINT('Ctrl Pts',(9.62260863652901,-8.72329062200737,-7.33414209133674));
#25535=CARTESIAN_POINT('Ctrl Pts',(8.83596460437641,-8.26196206072778,-7.64982933055117));
#25536=CARTESIAN_POINT('Ctrl Pts',(8.381315500447,-7.99533241831015,-7.83228405538782));
#25537=CARTESIAN_POINT('Ctrl Pts',(7.99969688490193,-7.76911080499082,-7.98693286597062));
#25538=CARTESIAN_POINT('Ctrl Pts',(7.5937904330124,-7.52350537407305,-8.15376232311957));
#25539=CARTESIAN_POINT('Ctrl Pts',(7.36145773430633,-7.3829257594442,-8.24925215291324));
#25540=CARTESIAN_POINT('Ctrl Pts',(7.13004605045563,-7.24116906982142,-8.34517464654933));
#25541=CARTESIAN_POINT('Ctrl Pts',(6.9,-7.09789564133157,-8.44145532612415));
#25542=CARTESIAN_POINT('',(6.9,-9.46599415782505,-5.6597919716369));
#25543=CARTESIAN_POINT('Ctrl Pts',(6.90000000000001,-7.09789564133157,-8.44145532612415));
#25544=CARTESIAN_POINT('Ctrl Pts',(6.90000000000001,-7.5077690000137,-8.09681826844945));
#25545=CARTESIAN_POINT('Ctrl Pts',(6.89999999999998,-7.89280389060837,-7.72210951819363));
#25546=CARTESIAN_POINT('Ctrl Pts',(6.89999999999998,-8.70687723936702,-6.80464666682922));
#25547=CARTESIAN_POINT('Ctrl Pts',(6.90000000000001,-9.11389129061078,-6.24868352466685));
#25548=CARTESIAN_POINT('Ctrl Pts',(6.90000000000001,-9.46599415782505,-5.6597919716369));
#25549=CARTESIAN_POINT('',(37.5,-32.3652591523689,1.50000000000001));
#25550=CARTESIAN_POINT('Ctrl Pts',(6.9,-9.46599415782505,-5.6597919716369));
#25551=CARTESIAN_POINT('Ctrl Pts',(6.98893730997541,-9.50231572683743,-5.61299197171201));
#25552=CARTESIAN_POINT('Ctrl Pts',(7.08052892388224,-9.53955640247953,-5.56508220248518));
#25553=CARTESIAN_POINT('Ctrl Pts',(7.17490192378012,-9.57777162403489,-5.51603067891051));
#25554=CARTESIAN_POINT('Ctrl Pts',(7.97363347618197,-9.90120844676305,-5.10088016324537));
#25555=CARTESIAN_POINT('Ctrl Pts',(8.96286060498076,-10.2954119066056,-4.58706675349253));
#25556=CARTESIAN_POINT('Ctrl Pts',(10.2403127965964,-10.8024441000946,-4.00248282963831));
#25557=CARTESIAN_POINT('Ctrl Pts',(10.4394276407756,-10.8814745615577,-3.91136447885237));
#25558=CARTESIAN_POINT('Ctrl Pts',(10.6449386760823,-10.9636620301539,-3.8176046549408));
#25559=CARTESIAN_POINT('Ctrl Pts',(10.857227022668,-11.0492678117687,-3.72139879136494));
#25560=CARTESIAN_POINT('Ctrl Pts',(11.0079272575414,-11.1100380405794,-3.65310372726809));
#25561=CARTESIAN_POINT('Ctrl Pts',(11.244571866109,-11.2057391107435,-3.54599023608119));
#25562=CARTESIAN_POINT('Ctrl Pts',(11.5512244262558,-11.3315975140438,-3.40956688340392));
#25563=CARTESIAN_POINT('Ctrl Pts',(12.0044642692893,-11.5176192545079,-3.20792989421993));
#25564=CARTESIAN_POINT('Ctrl Pts',(12.608246158217,-11.7683139215713,-2.94281490475174));
#25565=CARTESIAN_POINT('Ctrl Pts',(13.3027146141536,-12.0682094443783,-2.65901005153359));
#25566=CARTESIAN_POINT('Ctrl Pts',(14.2466220418226,-12.4758213511285,-2.27326825624961));
#25567=CARTESIAN_POINT('Ctrl Pts',(15.3788107202461,-12.9964429752181,-1.81469981611628));
#25568=CARTESIAN_POINT('Ctrl Pts',(16.3720853361384,-13.4908337691235,-1.45099516743195));
#25569=CARTESIAN_POINT('Ctrl Pts',(17.5300464833505,-14.067195353042,-1.02698770212637));
#25570=CARTESIAN_POINT('Ctrl Pts',(18.5522571217452,-14.6297459826146,-0.660939172705208));
#25571=CARTESIAN_POINT('Ctrl Pts',(19.459740928474,-15.1671394203612,-0.37124288507375));
#25572=CARTESIAN_POINT('Ctrl Pts',(20.7212139011503,-15.9141580364338,0.0314574545047842));
#25573=CARTESIAN_POINT('Ctrl Pts',(21.748318091447,-16.6062803213006,0.336055810056771));
#25574=CARTESIAN_POINT('Ctrl Pts',(22.5801692622301,-17.2054151585246,0.547760951425958));
#25575=CARTESIAN_POINT('Ctrl Pts',(23.3330995249136,-17.7477077779475,0.739380814811507));
#25576=CARTESIAN_POINT('Ctrl Pts',(23.9217876543842,-18.206905015041,0.875119715101746));
#25577=CARTESIAN_POINT('Ctrl Pts',(24.4822919865211,-18.6643830136337,0.991018194629963));
#25578=CARTESIAN_POINT('Ctrl Pts',(24.9418792870016,-19.0394935459661,1.08604951960313));
#25579=CARTESIAN_POINT('Ctrl Pts',(25.3626276506119,-19.3999270898306,1.16248493478925));
#25580=CARTESIAN_POINT('Ctrl Pts',(25.7525302890144,-19.7463071016619,1.22321331868058));
#25581=CARTESIAN_POINT('Ctrl Pts',(26.1776080056337,-20.1239357966488,1.28942031554593));
#25582=CARTESIAN_POINT('Ctrl Pts',(26.5661459571672,-20.4852396169796,1.33297321439401));
#25583=CARTESIAN_POINT('Ctrl Pts',(26.9267016831501,-20.8313979297669,1.3663881523399));
#25584=CARTESIAN_POINT('Ctrl Pts',(27.1778777842841,-21.0725442744658,1.38966620127396));
#25585=CARTESIAN_POINT('Ctrl Pts',(27.4154861119772,-21.3064162463263,1.40780557011332));
#25586=CARTESIAN_POINT('Ctrl Pts',(27.6422281942556,-21.5339888726617,1.42326116565077));
#25587=CARTESIAN_POINT('Ctrl Pts',(27.8555559933378,-21.7480980800028,1.43780239305054));
#25588=CARTESIAN_POINT('Ctrl Pts',(28.1190837193167,-22.0160369614215,1.45368682614544));
#25589=CARTESIAN_POINT('Ctrl Pts',(28.4603051775879,-22.3749799381774,1.47251023690701));
#25590=CARTESIAN_POINT('Ctrl Pts',(28.601773083253,-22.5237950549995,1.4803142844936));
#25591=CARTESIAN_POINT('Ctrl Pts',(28.7540286646448,-22.6856884569071,1.48853267939426));
#25592=CARTESIAN_POINT('Ctrl Pts',(28.9157341130969,-22.8599017516109,1.49763121638955));
#25593=CARTESIAN_POINT('Ctrl Pts',(29.4787137469354,-23.4664276157734,1.52930789194515));
#25594=CARTESIAN_POINT('Ctrl Pts',(30.1711677436439,-24.2477248210915,1.53976925233531));
#25595=CARTESIAN_POINT('Ctrl Pts',(30.8055547543787,-24.9885333989192,1.53340754825749));
#25596=CARTESIAN_POINT('Ctrl Pts',(31.1893125644455,-25.4366684847504,1.52955918190716));
#25597=CARTESIAN_POINT('Ctrl Pts',(31.5650207099063,-25.8828713567949,1.52122455967932));
#25598=CARTESIAN_POINT('Ctrl Pts',(31.9311744366552,-26.319234664178,1.51382648741802));
#25599=CARTESIAN_POINT('Ctrl Pts',(32.1142513000296,-26.5374163178695,1.51012745128737));
#25600=CARTESIAN_POINT('Ctrl Pts',(32.2949430642635,-26.7531357746902,1.50666813405654));
#25601=CARTESIAN_POINT('Ctrl Pts',(32.4730466959745,-26.9654180603387,1.50413682057756));
#25602=CARTESIAN_POINT('Ctrl Pts',(32.5932788659568,-27.1087231665129,1.50242801032164));
#25603=CARTESIAN_POINT('Ctrl Pts',(32.7123311760565,-27.2504621963818,1.50114220273886));
#25604=CARTESIAN_POINT('Ctrl Pts',(32.8301302692951,-27.3903440144041,1.50048655910813));
#25605=CARTESIAN_POINT('Ctrl Pts',(32.8868306159413,-27.457673459422,1.50017097755214));
#25606=CARTESIAN_POINT('Ctrl Pts',(32.9387123022443,-27.5192120661501,1.50000000000001));
#25607=CARTESIAN_POINT('Ctrl Pts',(33.,-27.5917792275077,1.50000000000001));
#25608=CARTESIAN_POINT('Ctrl Pts',(33.0955022515216,-27.7048578313703,1.50000000000001));
#25609=CARTESIAN_POINT('Ctrl Pts',(33.24174784516,-27.8775886863802,1.5));
#25610=CARTESIAN_POINT('Ctrl Pts',(33.3688392455923,-28.0268611295878,1.5));
#25611=CARTESIAN_POINT('Ctrl Pts',(34.2661932187598,-29.0808287429838,1.5));
#25612=CARTESIAN_POINT('Ctrl Pts',(35.2319960542697,-30.180966291201,1.50000000000001));
#25613=CARTESIAN_POINT('Ctrl Pts',(36.3004607333286,-31.2401426718624,1.50000000000001));
#25614=CARTESIAN_POINT('Ctrl Pts',(36.6891719086969,-31.6254747318907,1.50000000000001));
#25615=CARTESIAN_POINT('Ctrl Pts',(37.089305975904,-32.002886614661,1.50000000000001));
#25616=CARTESIAN_POINT('Ctrl Pts',(37.5,-32.3652591523689,1.50000000000001));
#25617=CARTESIAN_POINT('',(37.5,-32.1719479119405,3.83741678103716));
#25618=CARTESIAN_POINT('Origin',(37.5,0.,0.));
#25619=CARTESIAN_POINT('',(36.8,-31.4347259190859,4.53355051147315));
#25620=CARTESIAN_POINT('Ctrl Pts',(37.5,-32.1719479119405,3.83741678103717));
#25621=CARTESIAN_POINT('Ctrl Pts',(37.2470086540956,-31.9226755103028,4.04454785994593));
#25622=CARTESIAN_POINT('Ctrl Pts',(37.0122659037829,-31.6748439028166,4.2761329400914));
#25623=CARTESIAN_POINT('Ctrl Pts',(36.8,-31.4347259190859,4.53355051147316));
#25624=CARTESIAN_POINT('',(36.8,-29.4900464626661,11.7911930472673));
#25625=CARTESIAN_POINT('Ctrl Pts',(36.8,-31.4347259190859,4.53355051147315));
#25626=CARTESIAN_POINT('Ctrl Pts',(36.8,-31.1968691126063,6.18280168905531));
#25627=CARTESIAN_POINT('Ctrl Pts',(36.8,-30.8293258095436,7.81258162569766));
#25628=CARTESIAN_POINT('Ctrl Pts',(36.8,-30.0846548283827,10.2137688485759));
#25629=CARTESIAN_POINT('Ctrl Pts',(36.8,-29.8028301128151,11.0089139056503));
#25630=CARTESIAN_POINT('Ctrl Pts',(36.8,-29.4900464626661,11.7911930472673));
#25631=CARTESIAN_POINT('',(37.5,-29.7804325714888,12.7626735386834));
#25632=CARTESIAN_POINT('Ctrl Pts',(36.8,-29.4900464626661,11.7911930472673));
#25633=CARTESIAN_POINT('Ctrl Pts',(37.0122659037829,-29.5692859507915,12.1341821953298));
#25634=CARTESIAN_POINT('Ctrl Pts',(37.2470086540957,-29.6681218786625,12.4586565616163));
#25635=CARTESIAN_POINT('Ctrl Pts',(37.5,-29.7804325714888,12.7626735386834));
#25636=CARTESIAN_POINT('',(37.5,-28.7791366260183,14.8835914705078));
#25637=CARTESIAN_POINT('Origin',(37.5,0.,0.));
#25638=CARTESIAN_POINT('',(6.9,-10.3676856018661,-3.76156693666918));
#25639=CARTESIAN_POINT('Ctrl Pts',(37.5,-28.7791366260183,14.8835914705078));
#25640=CARTESIAN_POINT('Ctrl Pts',(36.6490696321449,-28.1289147924265,14.5081857198506));
#25641=CARTESIAN_POINT('Ctrl Pts',(35.8406537801018,-27.4207836130714,14.0993459928284));
#25642=CARTESIAN_POINT('Ctrl Pts',(35.0774452370719,-26.7027592163157,13.6847944140768));
#25643=CARTESIAN_POINT('Ctrl Pts',(34.695840965557,-26.3437470179379,13.477518624701));
#25644=CARTESIAN_POINT('Ctrl Pts',(34.325525504184,-25.9822790639256,13.2688250041486));
#25645=CARTESIAN_POINT('Ctrl Pts',(33.9666810635471,-25.6244801370893,13.0622496974238));
#25646=CARTESIAN_POINT('Ctrl Pts',(33.7186145566571,-25.3771363861544,12.9194457162392));
#25647=CARTESIAN_POINT('Ctrl Pts',(33.467102416882,-25.1224476749868,12.7724011202871));
#25648=CARTESIAN_POINT('Ctrl Pts',(33.2400985609469,-24.8908093158743,12.6386646512988));
#25649=CARTESIAN_POINT('Ctrl Pts',(33.1387264796113,-24.7873676254956,12.5789425635132));
#25650=CARTESIAN_POINT('Ctrl Pts',(33.0532004124129,-24.6997339702936,12.5283472490923));
#25651=CARTESIAN_POINT('Ctrl Pts',(33.,-24.6451817466334,12.4968515080772));
#25652=CARTESIAN_POINT('Ctrl Pts',(32.9185691495402,-24.5616817554558,12.4486427656934));
#25653=CARTESIAN_POINT('Ctrl Pts',(32.8516820632897,-24.4928265642338,12.4091965179816));
#25654=CARTESIAN_POINT('Ctrl Pts',(32.7777321455643,-24.4165289206393,12.3657029367261));
#25655=CARTESIAN_POINT('Ctrl Pts',(32.1788699539947,-23.7986543447101,12.013482647765));
#25656=CARTESIAN_POINT('Ctrl Pts',(31.5692879871422,-23.1567007301401,11.6640598398765));
#25657=CARTESIAN_POINT('Ctrl Pts',(30.9513498040681,-22.5260018679712,11.3096185478538));
#25658=CARTESIAN_POINT('Ctrl Pts',(30.642380712531,-22.2106524368868,11.1323979018424));
#25659=CARTESIAN_POINT('Ctrl Pts',(30.3347880607069,-21.9015729508076,10.9558507302082));
#25660=CARTESIAN_POINT('Ctrl Pts',(30.0249306371907,-21.5982641082844,10.7763433330207));
#25661=CARTESIAN_POINT('Ctrl Pts',(29.8700019254325,-21.4466096870229,10.6865896344269));
#25662=CARTESIAN_POINT('Ctrl Pts',(29.7145097313521,-21.296396533813,10.5960927952752));
#25663=CARTESIAN_POINT('Ctrl Pts',(29.5580100720471,-21.14757273789,10.5043591957288));
#25664=CARTESIAN_POINT('Ctrl Pts',(29.4797602423946,-21.0731608399285,10.4584923959556));
#25665=CARTESIAN_POINT('Ctrl Pts',(29.4012586241226,-20.9990965425469,10.4123158264265));
#25666=CARTESIAN_POINT('Ctrl Pts',(29.3224502420508,-20.9253755287759,10.3657636829137));
#25667=CARTESIAN_POINT('Ctrl Pts',(29.2736528206127,-20.8797281587468,10.336939026118));
#25668=CARTESIAN_POINT('Ctrl Pts',(29.224737793726,-20.8342124355846,10.3079703168507));
#25669=CARTESIAN_POINT('Ctrl Pts',(29.1756921969555,-20.7888277156719,10.2788413042191));
#25670=CARTESIAN_POINT('Ctrl Pts',(29.1455286057134,-20.7609156046929,10.2609266352547));
#25671=CARTESIAN_POINT('Ctrl Pts',(29.118149096832,-20.7356566759699,10.2446403152225));
#25672=CARTESIAN_POINT('Ctrl Pts',(29.0849408699094,-20.7051394327917,10.2248462834623));
#25673=CARTESIAN_POINT('Ctrl Pts',(29.0475462331583,-20.670775019842,10.2025569083253));
#25674=CARTESIAN_POINT('Ctrl Pts',(28.9599837407919,-20.5905365513284,10.150562007605));
#25675=CARTESIAN_POINT('Ctrl Pts',(28.8924081847562,-20.529003052346,10.1107110564809));
#25676=CARTESIAN_POINT('Ctrl Pts',(28.4410807634412,-20.1180296612357,9.84455228453923));
#25677=CARTESIAN_POINT('Ctrl Pts',(27.9936088566446,-19.7235361016266,9.59004457949594));
#25678=CARTESIAN_POINT('Ctrl Pts',(27.5122543094016,-19.3231338575611,9.31395242975933));
#25679=CARTESIAN_POINT('Ctrl Pts',(27.1397294105009,-19.0132587221866,9.10028206815794));
#25680=CARTESIAN_POINT('Ctrl Pts',(26.7276341640386,-18.6830630720646,8.86410488389253));
#25681=CARTESIAN_POINT('Ctrl Pts',(26.2530417505368,-18.3335669465969,8.57522710561968));
#25682=CARTESIAN_POINT('Ctrl Pts',(25.869494913884,-18.0511179871699,8.34176749926329));
#25683=CARTESIAN_POINT('Ctrl Pts',(25.4447383161098,-17.75405561874,8.07732257195745));
#25684=CARTESIAN_POINT('Ctrl Pts',(24.9635886608355,-17.4401876876767,7.77432947327157));
#25685=CARTESIAN_POINT('Ctrl Pts',(24.6119820459486,-17.210824454111,7.5529131704743));
#25686=CARTESIAN_POINT('Ctrl Pts',(24.2873626785981,-17.0017823418902,7.3468597886102));
#25687=CARTESIAN_POINT('Ctrl Pts',(23.6426616418513,-16.6259529315257,6.93898570173334));
#25688=CARTESIAN_POINT('Ctrl Pts',(23.5760533212114,-16.5871235137886,6.8968455368959));
#25689=CARTESIAN_POINT('Ctrl Pts',(23.5065967305478,-16.546947509856,6.85292160236948));
#25690=CARTESIAN_POINT('Ctrl Pts',(23.4342591639586,-16.5054784159948,6.80720851268154));
#25691=CARTESIAN_POINT('Ctrl Pts',(22.7443384436226,-16.1099662574108,6.37121917472936));
#25692=CARTESIAN_POINT('Ctrl Pts',(21.7987837593133,-15.6084067036785,5.75271743556796));
#25693=CARTESIAN_POINT('Ctrl Pts',(20.5610365528855,-15.0432759423309,4.96573918168374));
#25694=CARTESIAN_POINT('Ctrl Pts',(19.7234582214104,-14.6608543317657,4.43319430549868));
#25695=CARTESIAN_POINT('Ctrl Pts',(18.7603809281624,-14.2617573685878,3.80221290992159));
#25696=CARTESIAN_POINT('Ctrl Pts',(17.6514222906382,-13.8414640697512,3.10236545497629));
#25697=CARTESIAN_POINT('Ctrl Pts',(16.7565277906387,-13.5023006881889,2.53761072285444));
#25698=CARTESIAN_POINT('Ctrl Pts',(15.7613807992389,-13.1550491146656,1.89253400855812));
#25699=CARTESIAN_POINT('Ctrl Pts',(14.7199652846762,-12.8103195459473,1.24173803388781));
#25700=CARTESIAN_POINT('Ctrl Pts',(13.7316067501733,-12.4831529092169,0.624098151639976));
#25701=CARTESIAN_POINT('Ctrl Pts',(12.7260968661244,-12.1691790146818,-0.023032282421214));
#25702=CARTESIAN_POINT('Ctrl Pts',(11.7781012037546,-11.8786003909685,-0.615505739626223));
#25703=CARTESIAN_POINT('Ctrl Pts',(10.6475718363527,-11.5320717298292,-1.32205817373976));
#25704=CARTESIAN_POINT('Ctrl Pts',(9.62260863652904,-11.2216623289213,-1.98990805505865));
#25705=CARTESIAN_POINT('Ctrl Pts',(8.83596460437641,-10.9799836949691,-2.49396550450873));
#25706=CARTESIAN_POINT('Ctrl Pts',(8.38131550044618,-10.8403030136515,-2.78529075246711));
#25707=CARTESIAN_POINT('Ctrl Pts',(7.99969688490049,-10.7217137549231,-3.03233135775693));
#25708=CARTESIAN_POINT('Ctrl Pts',(7.59379043301041,-10.5924279410152,-3.29961262120675));
#25709=CARTESIAN_POINT('Ctrl Pts',(7.361457734305,-10.5184273383894,-3.45259904692512));
#25710=CARTESIAN_POINT('Ctrl Pts',(7.13004605045497,-10.4436236908379,-3.60654870801928));
#25711=CARTESIAN_POINT('Ctrl Pts',(6.9,-10.3676856018661,-3.76156693666918));
#25712=CARTESIAN_POINT('',(6.9,-11.02768739857,-0.168526548660246));
#25713=CARTESIAN_POINT('Ctrl Pts',(6.90000000000001,-10.3676856018661,-3.76156693666918));
#25714=CARTESIAN_POINT('Ctrl Pts',(6.90000000000001,-10.5551707158657,-3.24481773355662));
#25715=CARTESIAN_POINT('Ctrl Pts',(6.90000000000001,-10.7040448708755,-2.71398840242747));
#25716=CARTESIAN_POINT('Ctrl Pts',(6.90000000000001,-10.9457448952802,-1.51153848953113));
#25717=CARTESIAN_POINT('Ctrl Pts',(6.90000000000001,-11.0174195217678,-0.84041437002766));
#25718=CARTESIAN_POINT('Ctrl Pts',(6.90000000000001,-11.02768739857,-0.168526548660247));
#25719=CARTESIAN_POINT('',(37.5,-27.2791366260183,17.4816676818611));
#25720=CARTESIAN_POINT('Ctrl Pts',(6.9,-11.02768739857,-0.168526548660246));
#25721=CARTESIAN_POINT('Ctrl Pts',(6.98893730997578,-11.0357428000776,-0.109835775321743));
#25722=CARTESIAN_POINT('Ctrl Pts',(7.08052892388264,-11.0440392866244,-0.049724360260793));
#25723=CARTESIAN_POINT('Ctrl Pts',(7.17490192378011,-11.0526088775152,0.0118631160266181));
#25724=CARTESIAN_POINT('Ctrl Pts',(7.97363347621222,-11.1251381246873,0.533112420370669));
#25725=CARTESIAN_POINT('Ctrl Pts',(8.96286060502742,-11.2096216302968,1.17518961595099));
#25726=CARTESIAN_POINT('Ctrl Pts',(10.2403127965964,-11.3564324284624,1.93497024136951));
#25727=CARTESIAN_POINT('Ctrl Pts',(10.439427640776,-11.3793156403693,2.05339627863287));
#25728=CARTESIAN_POINT('Ctrl Pts',(10.6449386760821,-11.4036121640905,2.17568840229239));
#25729=CARTESIAN_POINT('Ctrl Pts',(10.857227022666,-11.4296460138916,2.30180801494842));
#25730=CARTESIAN_POINT('Ctrl Pts',(11.0079272576484,-11.4481270438004,2.39133838987944));
#25731=CARTESIAN_POINT('Ctrl Pts',(11.244571866198,-11.4774498561359,2.53195192940694));
#25732=CARTESIAN_POINT('Ctrl Pts',(11.5512244265066,-11.5182347543578,2.71302722024009));
#25733=CARTESIAN_POINT('Ctrl Pts',(12.004464269483,-11.5785158126582,2.98066084541349));
#25734=CARTESIAN_POINT('Ctrl Pts',(12.6082461583111,-11.6630662681827,3.33560449468883));
#25735=CARTESIAN_POINT('Ctrl Pts',(13.3027146141536,-11.7808809827897,3.73133446864291));
#25736=CARTESIAN_POINT('Ctrl Pts',(14.2466220417484,-11.9410123512658,4.2692026159931));
#25737=CARTESIAN_POINT('Ctrl Pts',(15.3788107201835,-12.1625996834172,4.92664534657395));
#25738=CARTESIAN_POINT('Ctrl Pts',(16.3720853361384,-12.4089023460099,5.48881820879721));
#25739=CARTESIAN_POINT('Ctrl Pts',(17.5300464833438,-12.6960423867943,6.1442002371016));
#25740=CARTESIAN_POINT('Ctrl Pts',(18.5522571217469,-13.0002012582108,6.74248287738932));
#25741=CARTESIAN_POINT('Ctrl Pts',(19.459740928474,-13.3207494833101,7.26206394073252));
#25742=CARTESIAN_POINT('Ctrl Pts',(20.7212139012125,-13.7663364121616,7.98432197299206));
#25743=CARTESIAN_POINT('Ctrl Pts',(21.7483180915274,-14.2134327156235,8.59417302929552));
#25744=CARTESIAN_POINT('Ctrl Pts',(22.5801692622301,-14.6264461342272,9.0770824783983));
#25745=CARTESIAN_POINT('Ctrl Pts',(23.3330995247002,-15.0002753871335,9.51417645754747));
#25746=CARTESIAN_POINT('Ctrl Pts',(23.9217876538143,-15.3300824094504,9.8613284118158));
#25747=CARTESIAN_POINT('Ctrl Pts',(24.4822919856966,-15.668320737957,10.1904384384949));
#25748=CARTESIAN_POINT('Ctrl Pts',(24.9418792864885,-15.9456603258612,10.4602932464266));
#25749=CARTESIAN_POINT('Ctrl Pts',(25.362627650368,-16.2195872237959,10.7067050298183));
#25750=CARTESIAN_POINT('Ctrl Pts',(25.7525302890144,-16.489196921628,10.9324873590558));
#25751=CARTESIAN_POINT('Ctrl Pts',(26.1776080055415,-16.7831294661882,11.1786386476896));
#25752=CARTESIAN_POINT('Ctrl Pts',(26.5661459570144,-17.0742513036037,11.3970084746332));
#25753=CARTESIAN_POINT('Ctrl Pts',(26.9267016829645,-17.357325727205,11.5990258161359));
#25754=CARTESIAN_POINT('Ctrl Pts',(27.1778777840597,-17.554525563243,11.7397583701913));
#25755=CARTESIAN_POINT('Ctrl Pts',(27.4154861117292,-17.747994947664,11.8724035103318));
#25756=CARTESIAN_POINT('Ctrl Pts',(27.6422281939979,-17.9373508254958,11.9995747618597));
#25757=CARTESIAN_POINT('Ctrl Pts',(27.8555559931681,-18.1155042246074,12.1192224379096));
#25758=CARTESIAN_POINT('Ctrl Pts',(28.1190837191615,-18.3396038860388,12.2669482012106));
#25759=CARTESIAN_POINT('Ctrl Pts',(28.4603051775582,-18.641045917149,12.4627212415658));
#25760=CARTESIAN_POINT('Ctrl Pts',(28.6017730832315,-18.7660215649979,12.5438873034438));
#25761=CARTESIAN_POINT('Ctrl Pts',(28.7540286646334,-18.9021161663134,12.6319513431655));
#25762=CARTESIAN_POINT('Ctrl Pts',(28.9157341130969,-19.0484400367167,12.7269375546994));
#25763=CARTESIAN_POINT('Ctrl Pts',(29.4787137469378,-19.557868505358,13.0576332925206));
#25764=CARTESIAN_POINT('Ctrl Pts',(30.1711677436509,-20.2292610528789,13.4573416990383));
#25765=CARTESIAN_POINT('Ctrl Pts',(30.8055547543906,-20.8740009526632,13.8222365906122));
#25766=CARTESIAN_POINT('Ctrl Pts',(31.1893125644552,-21.2640215044932,14.0429713505041));
#25767=CARTESIAN_POINT('Ctrl Pts',(31.5650207099141,-21.6546118380374,14.258854791945));
#25768=CARTESIAN_POINT('Ctrl Pts',(31.9311744366611,-22.0362125836393,14.4706295271182));
#25769=CARTESIAN_POINT('Ctrl Pts',(32.1142513000346,-22.2270129564403,14.5765168947048));
#25770=CARTESIAN_POINT('Ctrl Pts',(32.2949430642676,-22.4155611447519,14.6813807665129));
#25771=CARTESIAN_POINT('Ctrl Pts',(32.4730466959776,-22.6006686536355,14.7853297275589));
#25772=CARTESIAN_POINT('Ctrl Pts',(32.5932788659536,-22.7256289211957,14.8555024075504));
#25773=CARTESIAN_POINT('Ctrl Pts',(32.7123311760469,-22.8490214255548,14.9252583804501));
#25774=CARTESIAN_POINT('Ctrl Pts',(32.8301302692793,-22.9704904552987,14.9946314854175));
#25775=CARTESIAN_POINT('Ctrl Pts',(32.8868306159308,-23.0289572558904,15.0280229062851));
#25776=CARTESIAN_POINT('Ctrl Pts',(32.9387123022385,-23.0823367414113,15.0586441387483));
#25777=CARTESIAN_POINT('Ctrl Pts',(33.,-23.1451817466334,15.0949277194305));
#25778=CARTESIAN_POINT('Ctrl Pts',(33.0955022515197,-23.243110690201,15.1514670213607));
#25779=CARTESIAN_POINT('Ctrl Pts',(33.2417478451538,-23.3926999986525,15.2378324488631));
#25780=CARTESIAN_POINT('Ctrl Pts',(33.3688392455845,-23.5219737265538,15.312468670466));
#25781=CARTESIAN_POINT('Ctrl Pts',(34.266193219056,-24.43473645483,15.8394524773426));
#25782=CARTESIAN_POINT('Ctrl Pts',(35.231996054922,-25.3874835195854,16.3895212516487));
#25783=CARTESIAN_POINT('Ctrl Pts',(36.3004607343901,-26.3047571725944,16.919109442134));
#25784=CARTESIAN_POINT('Ctrl Pts',(36.6891719094257,-26.6384645251555,17.1117754719657));
#25785=CARTESIAN_POINT('Ctrl Pts',(37.0893059762781,-26.9653128030153,17.3004814131722));
#25786=CARTESIAN_POINT('Ctrl Pts',(37.5,-27.2791366260183,17.4816676818611));
#25787=CARTESIAN_POINT('',(37.5,-25.9430157904516,19.4092743732572));
#25788=CARTESIAN_POINT('Origin',(37.5,0.,0.));
#25789=CARTESIAN_POINT('',(36.8,-24.9564959511929,19.6435328718186));
#25790=CARTESIAN_POINT('Ctrl Pts',(37.5,-25.9430157904516,19.4092743732572));
#25791=CARTESIAN_POINT('Ctrl Pts',(37.2470086540956,-25.6235740187166,19.4640189486865));
#25792=CARTESIAN_POINT('Ctrl Pts',(37.0122659037829,-25.2931530107001,19.5406617074869));
#25793=CARTESIAN_POINT('Ctrl Pts',(36.8,-24.9564959511929,19.6435328718186));
#25794=CARTESIAN_POINT('',(36.8,-19.6435328718186,24.9564959511929));
#25795=CARTESIAN_POINT('Ctrl Pts',(36.8,-24.9564959511929,19.6435328718186));
#25796=CARTESIAN_POINT('Ctrl Pts',(36.8,-24.4957748831848,20.2288646216318));
#25797=CARTESIAN_POINT('Ctrl Pts',(36.8,-24.0141222843114,20.7984186457787));
#25798=CARTESIAN_POINT('Ctrl Pts',(36.8,-22.3234241559746,22.6602579716864));
#25799=CARTESIAN_POINT('Ctrl Pts',(36.8,-21.029056769996,23.8659348286794));
#25800=CARTESIAN_POINT('Ctrl Pts',(36.8,-19.6435328718186,24.9564959511929));
#25801=CARTESIAN_POINT('',(37.5,-19.4092743732571,25.9430157904517));
#25802=CARTESIAN_POINT('Ctrl Pts',(36.8,-19.6435328718186,24.9564959511929));
#25803=CARTESIAN_POINT('Ctrl Pts',(37.0122659037829,-19.5406617074869,25.2931530107001));
#25804=CARTESIAN_POINT('Ctrl Pts',(37.2470086540956,-19.4640189486865,25.6235740187166));
#25805=CARTESIAN_POINT('Ctrl Pts',(37.5,-19.4092743732572,25.9430157904516));
#25806=CARTESIAN_POINT('',(37.5,-17.4816676818611,27.2791366260183));
#25807=CARTESIAN_POINT('Origin',(37.5,0.,0.));
#25808=CARTESIAN_POINT('',(6.9,-10.8594625780008,1.9262302757419));
#25809=CARTESIAN_POINT('Ctrl Pts',(37.5,-17.4816676818611,27.2791366260183));
#25810=CARTESIAN_POINT('Ctrl Pts',(36.6490696321448,-17.1062619312039,26.6289147924265));
#25811=CARTESIAN_POINT('Ctrl Pts',(35.8406537801013,-16.6974222041815,25.920783613071));
#25812=CARTESIAN_POINT('Ctrl Pts',(35.0774452370697,-16.2828706254288,25.2027592163136));
#25813=CARTESIAN_POINT('Ctrl Pts',(34.6958409655539,-16.0755948360525,24.8437470179349));
#25814=CARTESIAN_POINT('Ctrl Pts',(34.3255255041797,-15.8669012154994,24.4822790639214));
#25815=CARTESIAN_POINT('Ctrl Pts',(33.9666810635412,-15.6603259087737,24.1244801370834));
#25816=CARTESIAN_POINT('Ctrl Pts',(33.718614556661,-15.5175219275947,23.8771363861582));
#25817=CARTESIAN_POINT('Ctrl Pts',(33.4671024168984,-15.3704773316499,23.6224476750034));
#25818=CARTESIAN_POINT('Ctrl Pts',(33.2400985609675,-15.2367408626642,23.3908093158952));
#25819=CARTESIAN_POINT('Ctrl Pts',(33.1387264796193,-15.1770187748713,23.2873676255038));
#25820=CARTESIAN_POINT('Ctrl Pts',(33.0532004124107,-15.1264234604443,23.1997339702914));
#25821=CARTESIAN_POINT('Ctrl Pts',(33.,-15.0949277194305,23.1451817466334));
#25822=CARTESIAN_POINT('Ctrl Pts',(32.9185691495597,-15.0467189770583,23.0616817554757));
#25823=CARTESIAN_POINT('Ctrl Pts',(32.851682063321,-15.0068117561407,22.9930927072745));
#25824=CARTESIAN_POINT('Ctrl Pts',(32.7777321456099,-14.9624828491754,22.917277339223));
#25825=CARTESIAN_POINT('Ctrl Pts',(32.1788699540345,-14.6034979145461,22.3033083332839));
#25826=CARTESIAN_POINT('Ctrl Pts',(31.5692879871757,-14.2222611802172,21.679722497699));
#25827=CARTESIAN_POINT('Ctrl Pts',(30.9513498040926,-13.8532805894466,21.0574179035634));
#25828=CARTESIAN_POINT('Ctrl Pts',(30.6423807125511,-13.6687902940613,20.7462656064956));
#25829=CARTESIAN_POINT('Ctrl Pts',(30.3347880607231,-13.4893931931425,20.4388315278504));
#25830=CARTESIAN_POINT('Ctrl Pts',(30.0249306372029,-13.3164737289165,20.1317191404533));
#25831=CARTESIAN_POINT('Ctrl Pts',(29.8700019254428,-13.2300139968034,19.9781629467547));
#25832=CARTESIAN_POINT('Ctrl Pts',(29.7145097313604,-13.1451740097158,19.8246838084803));
#25833=CARTESIAN_POINT('Ctrl Pts',(29.5580100720534,-13.0621556215309,19.670828282929));
#25834=CARTESIAN_POINT('Ctrl Pts',(29.4797602423999,-13.0206464274385,19.5939005201534));
#25835=CARTESIAN_POINT('Ctrl Pts',(29.401258624127,-12.9795931491566,19.5168782891898));
#25836=CARTESIAN_POINT('Ctrl Pts',(29.3224502420541,-12.939024950194,19.4397024434206));
#25837=CARTESIAN_POINT('Ctrl Pts',(29.2736528205583,-12.913905496501,19.3919158733091));
#25838=CARTESIAN_POINT('Ctrl Pts',(29.2247377936137,-12.8889720785753,19.3440703735311));
#25839=CARTESIAN_POINT('Ctrl Pts',(29.1756921967849,-12.8642322644742,19.2961515485917));
#25840=CARTESIAN_POINT('Ctrl Pts',(29.1455286055995,-12.8490170018044,19.2666809347342));
#25841=CARTESIAN_POINT('Ctrl Pts',(29.1181490967649,-12.8352852878977,19.2399471035364));
#25842=CARTESIAN_POINT('Ctrl Pts',(29.0849408699094,-12.8187535959654,19.2075463476651));
#25843=CARTESIAN_POINT('Ctrl Pts',(29.0475462330785,-12.8001378288936,19.1710609760093));
#25844=CARTESIAN_POINT('Ctrl Pts',(28.9599837406718,-12.7566467271403,19.0859128368227));
#25845=CARTESIAN_POINT('Ctrl Pts',(28.8924081845882,-12.7232826293765,19.0206341512474));
#25846=CARTESIAN_POINT('Ctrl Pts',(28.441080763257,-12.5004486183602,18.5846471977387));
#25847=CARTESIAN_POINT('Ctrl Pts',(27.9936088564545,-12.286061026631,18.1669902799056));
#25848=CARTESIAN_POINT('Ctrl Pts',(27.5122543091764,-12.0773485863978,17.7276863423864));
#25849=CARTESIAN_POINT('Ctrl Pts',(27.1397294103343,-11.9158240279936,17.3877048135723));
#25850=CARTESIAN_POINT('Ctrl Pts',(26.7276341639424,-11.7479547989366,17.0180715472069));
#25851=CARTESIAN_POINT('Ctrl Pts',(26.2530417505368,-11.5897211649258,16.593147989986));
#25852=CARTESIAN_POINT('Ctrl Pts',(25.8694949138842,-11.4618429939678,16.2497415604106));
#25853=CARTESIAN_POINT('Ctrl Pts',(25.4447383161107,-11.3368019000522,15.8721943512474));
#25854=CARTESIAN_POINT('Ctrl Pts',(24.9635886608374,-11.2164808476613,15.4528606650833));
#25855=CARTESIAN_POINT('Ctrl Pts',(24.6119820459382,-11.1285546120948,15.1464269052552));
#25856=CARTESIAN_POINT('Ctrl Pts',(24.2873626785755,-11.0505455233798,14.863458385904));
#25857=CARTESIAN_POINT('Ctrl Pts',(23.6426616417925,-10.9290047499479,14.3223143599116));
#25858=CARTESIAN_POINT('Ctrl Pts',(23.5760533211706,-10.9164475701956,14.2664051977893));
#25859=CARTESIAN_POINT('Ctrl Pts',(23.5065967305265,-10.9036160974344,14.2082779527054));
#25860=CARTESIAN_POINT('Ctrl Pts',(23.4342591639586,-10.8905593535264,14.1479547088373));
#25861=CARTESIAN_POINT('Ctrl Pts',(22.7443384436235,-10.7660304456633,13.5726207871003));
#25862=CARTESIAN_POINT('Ctrl Pts',(21.7987837593143,-10.640918000201,12.7862027918356));
#25863=CARTESIAN_POINT('Ctrl Pts',(20.5610365528855,-10.544989531356,11.8220942510713));
#25864=CARTESIAN_POINT('Ctrl Pts',(19.7234582214107,-10.4800751397429,11.1696860543574));
#25865=CARTESIAN_POINT('Ctrl Pts',(18.7603809281627,-10.4499377288461,10.4236916548834));
#25866=CARTESIAN_POINT('Ctrl Pts',(17.6514222906382,-10.4358767824859,9.60745933070834));
#25867=CARTESIAN_POINT('Ctrl Pts',(16.7565277906386,-10.4245300440805,8.94878569500211));
#25868=CARTESIAN_POINT('Ctrl Pts',(15.7613807992386,-10.4463397170534,8.21650708626994));
#25869=CARTESIAN_POINT('Ctrl Pts',(14.7199652846762,-10.4731931404428,7.48053645516581));
#25870=CARTESIAN_POINT('Ctrl Pts',(13.7316067501732,-10.4986784628874,6.78206130838347));
#25871=CARTESIAN_POINT('Ctrl Pts',(12.7260968661243,-10.5503343111255,6.06464296565691));
#25872=CARTESIAN_POINT('Ctrl Pts',(11.7781012037546,-10.5949225697956,5.40625658879283));
#25873=CARTESIAN_POINT('Ctrl Pts',(10.6475718363526,-10.6480961631663,4.62109990117504));
#25874=CARTESIAN_POINT('Ctrl Pts',(9.62260863652902,-10.713198677066,3.88752023758458));
#25875=CARTESIAN_POINT('Ctrl Pts',(8.83596460437641,-10.7559275652365,3.33015436441791));
#25876=CARTESIAN_POINT('Ctrl Pts',(8.38131550044684,-10.7806231707767,3.00801895826384));
#25877=CARTESIAN_POINT('Ctrl Pts',(7.99969688490164,-10.8014421627468,2.7347808889527));
#25878=CARTESIAN_POINT('Ctrl Pts',(7.59379043301203,-10.8231179952785,2.43866561789595));
#25879=CARTESIAN_POINT('Ctrl Pts',(7.36145773430608,-10.8355248063684,2.26917518547639));
#25880=CARTESIAN_POINT('Ctrl Pts',(7.1300460504555,-10.8477177778403,2.09844904428872));
#25881=CARTESIAN_POINT('Ctrl Pts',(6.9,-10.8594625780008,1.9262302757419));
#25882=CARTESIAN_POINT('',(6.9,-9.63452070648529,5.36789542693312));
#25883=CARTESIAN_POINT('Ctrl Pts',(6.90000000000001,-10.8594625780008,1.92623027574191));
#25884=CARTESIAN_POINT('Ctrl Pts',(6.90000000000001,-10.7829659225815,2.35749364924904));
#25885=CARTESIAN_POINT('Ctrl Pts',(6.90000000000001,-10.6806923192591,2.78469328079873));
#25886=CARTESIAN_POINT('Ctrl Pts',(6.90000000000001,-10.3240838050858,3.958690010018));
#25887=CARTESIAN_POINT('Ctrl Pts',(6.90000000000001,-10.0158641401962,4.68344446130229));
#25888=CARTESIAN_POINT('Ctrl Pts',(6.90000000000001,-9.6345207064853,5.36789542693312));
#25889=CARTESIAN_POINT('',(37.5,-14.8835914705078,28.7791366260183));
#25890=CARTESIAN_POINT('Ctrl Pts',(6.9,-9.6345207064853,5.36789542693312));
#25891=CARTESIAN_POINT('Ctrl Pts',(6.98893730997577,-9.61215150215932,5.42275082836582));
#25892=CARTESIAN_POINT('Ctrl Pts',(7.08052892388263,-9.58928076274048,5.47895708413941));
#25893=CARTESIAN_POINT('Ctrl Pts',(7.17490192378011,-9.56590850800827,5.5365781986047));
#25894=CARTESIAN_POINT('Ctrl Pts',(7.97363347621106,-9.36809602640493,6.02425796145695));
#25895=CARTESIAN_POINT('Ctrl Pts',(8.96286060502533,-9.12022229067351,6.62255487682446));
#25896=CARTESIAN_POINT('Ctrl Pts',(10.2403127965964,-8.8674738587251,7.35394959882411));
#25897=CARTESIAN_POINT('Ctrl Pts',(10.4394276407753,-8.82807828292514,7.46795116151676));
#25898=CARTESIAN_POINT('Ctrl Pts',(10.6449386760807,-8.78797362786174,7.58600750914886));
#25899=CARTESIAN_POINT('Ctrl Pts',(10.8572270226639,-8.74745979681984,7.70824722252455));
#25900=CARTESIAN_POINT('Ctrl Pts',(11.0079272576426,-8.71869965074415,7.79502331657747));
#25901=CARTESIAN_POINT('Ctrl Pts',(11.2445718661922,-8.67378718137334,7.93145962009207));
#25902=CARTESIAN_POINT('Ctrl Pts',(11.5512244264957,-8.61857029390861,8.1086678710592));
#25903=CARTESIAN_POINT('Ctrl Pts',(12.0044642694743,-8.53695840917655,8.37058591851777));
#25904=CARTESIAN_POINT('Ctrl Pts',(12.6082461583068,-8.43270942692374,8.72025136346692));
#25905=CARTESIAN_POINT('Ctrl Pts',(13.3027146141536,-8.33687497573541,9.12187093125611));
#25906=CARTESIAN_POINT('Ctrl Pts',(14.2466220417512,-8.20661873510301,9.66774409498751));
#25907=CARTESIAN_POINT('Ctrl Pts',(15.3788107201857,-8.06979762861279,10.3478998672794));
#25908=CARTESIAN_POINT('Ctrl Pts',(16.3720853361384,-8.00201556032625,10.9579071785779));
#25909=CARTESIAN_POINT('Ctrl Pts',(17.5300464833433,-7.92299511593714,11.6690546846652));
#25910=CARTESIAN_POINT('Ctrl Pts',(18.5522571217459,-7.8872631052263,12.3392620855055));
#25911=CARTESIAN_POINT('Ctrl Pts',(19.459740928474,-7.9050754796287,12.9495065982363));
#25912=CARTESIAN_POINT('Ctrl Pts',(20.7212139012062,-7.92983606347848,13.797793866682));
#25913=CARTESIAN_POINT('Ctrl Pts',(21.7483180915204,-8.01210729206202,14.5494885256954));
#25914=CARTESIAN_POINT('Ctrl Pts',(22.5801692622301,-8.12833268012627,15.1742070856531));
#25915=CARTESIAN_POINT('Ctrl Pts',(23.3330995247288,-8.23353132025034,15.7396562019122));
#25916=CARTESIAN_POINT('Ctrl Pts',(23.9217876538748,-8.34557660279632,16.2052021244665));
#25917=CARTESIAN_POINT('Ctrl Pts',(24.4822919857808,-8.47394457448518,16.6593389324847));
#25918=CARTESIAN_POINT('Ctrl Pts',(24.9418792865409,-8.57920029911431,17.0317098454144));
#25919=CARTESIAN_POINT('Ctrl Pts',(25.3626276503928,-8.69322205980333,17.3820721585682));
#25920=CARTESIAN_POINT('Ctrl Pts',(25.7525302890144,-8.81381974260611,17.7124102403086));
#25921=CARTESIAN_POINT('Ctrl Pts',(26.1776080055521,-8.94529714888064,18.0725497817287));
#25922=CARTESIAN_POINT('Ctrl Pts',(26.5661459570323,-9.08823114221038,18.4072245179962));
#25923=CARTESIAN_POINT('Ctrl Pts',(26.926701682987,-9.23237211346181,18.7237138795475));
#25924=CARTESIAN_POINT('Ctrl Pts',(27.1778777840906,-9.33278590406893,18.9441917645255));
#25925=CARTESIAN_POINT('Ctrl Pts',(27.4154861117667,-9.43401273576512,19.1558005177924));
#25926=CARTESIAN_POINT('Ctrl Pts',(27.6422281940404,-9.53441411056212,19.3606119911674));
#25927=CARTESIAN_POINT('Ctrl Pts',(27.8555559931963,-9.62887564193249,19.5533066176737));
#25928=CARTESIAN_POINT('Ctrl Pts',(28.1190837191893,-9.74908876006132,19.7932907122016));
#25929=CARTESIAN_POINT('Ctrl Pts',(28.4603051775662,-9.91225869658421,20.113556154062));
#25930=CARTESIAN_POINT('Ctrl Pts',(28.6017730832374,-9.97990775153573,20.2463358494959));
#25931=CARTESIAN_POINT('Ctrl Pts',(28.7540286646365,-10.0537371137307,20.39064884571));
#25932=CARTESIAN_POINT('Ctrl Pts',(28.9157341130969,-10.1329641969115,20.5460712531062));
#25933=CARTESIAN_POINT('Ctrl Pts',(29.4787137469323,-10.4087943232527,21.0871763972981));
#25934=CARTESIAN_POINT('Ctrl Pts',(30.1711677436376,-10.7903831220537,21.7690303052012));
#25935=CARTESIAN_POINT('Ctrl Pts',(30.8055547543695,-11.1662968083083,22.4074085008994));
#25936=CARTESIAN_POINT('Ctrl Pts',(31.189312564438,-11.3936971342473,22.7935806863828));
#25937=CARTESIAN_POINT('Ctrl Pts',(31.5650207099004,-11.6240165648507,23.1758363977026));
#25938=CARTESIAN_POINT('Ctrl Pts',(31.9311744366508,-11.8486051370605,23.5500390710467));
#25939=CARTESIAN_POINT('Ctrl Pts',(32.114251300026,-11.9608994231654,23.7371404077187));
#25940=CARTESIAN_POINT('Ctrl Pts',(32.2949430642606,-12.0717550081779,23.9222292788013));
#25941=CARTESIAN_POINT('Ctrl Pts',(32.4730466959723,-12.1800883327803,24.1048054742076));
#25942=CARTESIAN_POINT('Ctrl Pts',(32.5932788659641,-12.2532207589651,24.2280569315282));
#25943=CARTESIAN_POINT('Ctrl Pts',(32.7123311760732,-12.3252038159362,24.3501636283207));
#25944=CARTESIAN_POINT('Ctrl Pts',(32.8301302693208,-12.3957125289927,24.4709770144495));
#25945=CARTESIAN_POINT('Ctrl Pts',(32.8868306159583,-12.4296505531409,24.5291282334708));
#25946=CARTESIAN_POINT('Ctrl Pts',(32.9387123022541,-12.4605679274042,24.5823367414274));
#25947=CARTESIAN_POINT('Ctrl Pts',(33.,-12.4968515080772,24.6451817466334));
#25948=CARTESIAN_POINT('Ctrl Pts',(33.0955022515283,-12.5533908100124,24.7431106902098));
#25949=CARTESIAN_POINT('Ctrl Pts',(33.2417478451817,-12.6397562375262,24.8926999986811));
#25950=CARTESIAN_POINT('Ctrl Pts',(33.3688392456272,-12.7143924591378,25.0219737265972));
#25951=CARTESIAN_POINT('Ctrl Pts',(34.2661932188391,-13.2413762658613,25.9347364546084));
#25952=CARTESIAN_POINT('Ctrl Pts',(35.2319960544065,-13.7914450400007,26.8874835190751));
#25953=CARTESIAN_POINT('Ctrl Pts',(36.3004607335293,-14.321033230354,27.8047571718553));
#25954=CARTESIAN_POINT('Ctrl Pts',(36.6891719088346,-14.5136992603336,28.1384645246727));
#25955=CARTESIAN_POINT('Ctrl Pts',(37.0893059759746,-14.702405201685,28.4653128027834));
#25956=CARTESIAN_POINT('Ctrl Pts',(37.5,-14.8835914705078,28.7791366260183));
#25957=CARTESIAN_POINT('',(37.5,-12.7626735386834,29.7804325714888));
#25958=CARTESIAN_POINT('Origin',(37.5,0.,0.));
#25959=CARTESIAN_POINT('',(36.8,-11.7911930472672,29.4900464626661));
#25960=CARTESIAN_POINT('Ctrl Pts',(37.5,-12.7626735386834,29.7804325714888));
#25961=CARTESIAN_POINT('Ctrl Pts',(37.2470086540956,-12.4586565616162,29.6681218786625));
#25962=CARTESIAN_POINT('Ctrl Pts',(37.0122659037829,-12.1341821953297,29.5692859507915));
#25963=CARTESIAN_POINT('Ctrl Pts',(36.8,-11.7911930472673,29.4900464626661));
#25964=CARTESIAN_POINT('',(36.8,-4.53355051147314,31.4347259190859));
#25965=CARTESIAN_POINT('Ctrl Pts',(36.8,-11.7911930472672,29.4900464626661));
#25966=CARTESIAN_POINT('Ctrl Pts',(36.8,-9.4561105348841,30.4236973716148));
#25967=CARTESIAN_POINT('Ctrl Pts',(36.8,-7.0196747094175,31.0761743714061));
#25968=CARTESIAN_POINT('Ctrl Pts',(36.8,-4.53355051147314,31.4347259190859));
#25969=CARTESIAN_POINT('',(37.5,-3.83741678103714,32.1719479119405));
#25970=CARTESIAN_POINT('Ctrl Pts',(36.8,-4.53355051147314,31.4347259190859));
#25971=CARTESIAN_POINT('Ctrl Pts',(37.0122659037829,-4.27613294009141,31.6748439028166));
#25972=CARTESIAN_POINT('Ctrl Pts',(37.2470086540955,-4.04454785994598,31.9226755103027));
#25973=CARTESIAN_POINT('Ctrl Pts',(37.5,-3.83741678103716,32.1719479119405));
#25974=CARTESIAN_POINT('',(37.5,-1.5,32.3652591523689));
#25975=CARTESIAN_POINT('Origin',(37.5,0.,0.));
#25976=CARTESIAN_POINT('',(6.9,-8.44145532612415,7.09789564133157));
#25977=CARTESIAN_POINT('Ctrl Pts',(37.5,-1.5,32.3652591523689));
#25978=CARTESIAN_POINT('Ctrl Pts',(36.6490696321448,-1.5,31.6144476510545));
#25979=CARTESIAN_POINT('Ctrl Pts',(35.840653780102,-1.5,30.7967681970102));
#25980=CARTESIAN_POINT('Ctrl Pts',(35.0774452370729,-1.5,29.9676650395079));
#25981=CARTESIAN_POINT('Ctrl Pts',(34.6958409655584,-1.5,29.5531134607568));
#25982=CARTESIAN_POINT('Ctrl Pts',(34.325525504186,-1.5,29.1357262196526));
#25983=CARTESIAN_POINT('Ctrl Pts',(33.9666810635498,-1.5,28.7225756062041));
#25984=CARTESIAN_POINT('Ctrl Pts',(33.7186145566569,-1.5,28.4369676438316));
#25985=CARTESIAN_POINT('Ctrl Pts',(33.4671024168784,-1.5,28.1428784519232));
#25986=CARTESIAN_POINT('Ctrl Pts',(33.2400985609418,-1.5,27.8754055139448));
#25987=CARTESIAN_POINT('Ctrl Pts',(33.13872647961,-1.5,27.7559613383782));
#25988=CARTESIAN_POINT('Ctrl Pts',(33.0532004124147,-1.5,27.65477070954));
#25989=CARTESIAN_POINT('Ctrl Pts',(33.,-1.5,27.5917792275077));
#25990=CARTESIAN_POINT('Ctrl Pts',(32.9185691495555,-1.5,27.4953617427583));
#25991=CARTESIAN_POINT('Ctrl Pts',(32.8516820632662,-1.4997338569914,27.4160082740758));
#25992=CARTESIAN_POINT('Ctrl Pts',(32.7777321455096,-1.49925158146269,27.3281857858092));
#25993=CARTESIAN_POINT('Ctrl Pts',(32.1788699539487,-1.49534601146588,26.6169805622313));
#25994=CARTESIAN_POINT('Ctrl Pts',(31.5692879871054,-1.47697823247432,25.8863210200298));
#25995=CARTESIAN_POINT('Ctrl Pts',(30.9513498040414,-1.4685839644322,25.1628991372544));
#25996=CARTESIAN_POINT('Ctrl Pts',(30.6423807125094,-1.46438683041114,24.8011881958668));
#25997=CARTESIAN_POINT('Ctrl Pts',(30.3347880606899,-1.46274142297322,24.4452439233219));
#25998=CARTESIAN_POINT('Ctrl Pts',(30.024930637178,-1.46654496784342,24.0928170619159));
#25999=CARTESIAN_POINT('Ctrl Pts',(29.870001925422,-1.46844674027852,23.9166036312129));
#26000=CARTESIAN_POINT('Ctrl Pts',(29.7145097313437,-1.47171272534115,23.7412668049772));
#26001=CARTESIAN_POINT('Ctrl Pts',(29.558010072041,-1.47674445496737,23.5665148172495));
#26002=CARTESIAN_POINT('Ctrl Pts',(29.4797602423896,-1.47926031978048,23.4791388233857));
#26003=CARTESIAN_POINT('Ctrl Pts',(29.4012586241187,-1.48221825336153,23.3919089755765));
#26004=CARTESIAN_POINT('Ctrl Pts',(29.322450242048,-1.48567308535868,23.3047886331029));
#26005=CARTESIAN_POINT('Ctrl Pts',(29.2736528205962,-1.48781228538512,23.2508445226287));
#26006=CARTESIAN_POINT('Ctrl Pts',(29.2247377936956,-1.4901420619451,23.1969423954499));
#26007=CARTESIAN_POINT('Ctrl Pts',(29.1756921969113,-1.49267616691569,23.1430735687309));
#26008=CARTESIAN_POINT('Ctrl Pts',(29.145528605684,-1.49423466984912,23.1099436370839));
#26009=CARTESIAN_POINT('Ctrl Pts',(29.1181490968213,-1.49570957236866,23.0799256031418));
#26010=CARTESIAN_POINT('Ctrl Pts',(29.0849408699094,-1.4975930851266,23.0435998794277));
#26011=CARTESIAN_POINT('Ctrl Pts',(29.0475462331498,-1.49971404375539,23.0026947372493));
#26012=CARTESIAN_POINT('Ctrl Pts',(28.9599837408025,-1.50462371438853,22.9072087348165));
#26013=CARTESIAN_POINT('Ctrl Pts',(28.8924081847867,-1.50836890093464,22.8339936859735));
#26014=CARTESIAN_POINT('Ctrl Pts',(28.4410807635146,-1.53338246331873,22.3450009030674));
#26015=CARTESIAN_POINT('Ctrl Pts',(27.9936088567427,-1.55654582153956,21.8761056063188));
#26016=CARTESIAN_POINT('Ctrl Pts',(27.5122543095517,-1.59544751495705,21.391301016406));
#26017=CARTESIAN_POINT('Ctrl Pts',(27.1397294106107,-1.62555390845339,21.0161060963261));
#26018=CARTESIAN_POINT('Ctrl Pts',(26.7276341641016,-1.66499152476168,20.6120596829205));
#26019=CARTESIAN_POINT('Ctrl Pts',(26.2530417505368,-1.74041895661093,20.1649482705455));
#26020=CARTESIAN_POINT('Ctrl Pts',(25.8694949138819,-1.80137642675986,19.8036104932291));
#26021=CARTESIAN_POINT('Ctrl Pts',(25.4447383161056,-1.88186126749416,19.4141244720056));
#26022=CARTESIAN_POINT('Ctrl Pts',(24.9635886608287,-1.98732702259654,18.9908103209264));
#26023=CARTESIAN_POINT('Ctrl Pts',(24.6119820459616,-2.06439754884394,18.6814677825833));
#26024=CARTESIAN_POINT('Ctrl Pts',(24.2873626786293,-2.13832395595953,18.3974053120239));
#26025=CARTESIAN_POINT('Ctrl Pts',(23.6426616419432,-2.30363857154125,17.8679904517678));
#26026=CARTESIAN_POINT('Ctrl Pts',(23.5760533212753,-2.3207183159486,17.8132931071512));
#26027=CARTESIAN_POINT('Ctrl Pts',(23.506596730581,-2.3386695571242,17.7565376998347));
#26028=CARTESIAN_POINT('Ctrl Pts',(23.4342591639586,-2.3575237071575,17.697767866208));
#26029=CARTESIAN_POINT('Ctrl Pts',(22.7443384436212,-2.53734547031163,17.1372496203914));
#26030=CARTESIAN_POINT('Ctrl Pts',(21.7987837593118,-2.82220391184419,16.3936354357679));
#26031=CARTESIAN_POINT('Ctrl Pts',(20.5610365528855,-3.2211816912596,15.5107287130397));
#26032=CARTESIAN_POINT('Ctrl Pts',(19.7234582214102,-3.49116827740858,14.9132694452414));
#26033=CARTESIAN_POINT('Ctrl Pts',(18.7603809281622,-3.83806571370471,14.2521506387675));
#26034=CARTESIAN_POINT('Ctrl Pts',(17.6514222906382,-4.23400473904287,13.5382422374622));
#26035=CARTESIAN_POINT('Ctrl Pts',(16.7565277906387,-4.55351499318673,12.9621407669349));
#26036=CARTESIAN_POINT('Ctrl Pts',(15.7613807992389,-4.9385420283955,12.3388737256114));
#26037=CARTESIAN_POINT('Ctrl Pts',(14.7199652846762,-5.32978309078145,11.7149311743306));
#26038=CARTESIAN_POINT('Ctrl Pts',(13.7316067501733,-5.70109160083332,11.1227766145274));
#26039=CARTESIAN_POINT('Ctrl Pts',(12.7260968661244,-6.10453604902481,10.5273020287043));
#26040=CARTESIAN_POINT('Ctrl Pts',(11.7781012037546,-6.47234380217571,9.9794168301694));
#26041=CARTESIAN_POINT('Ctrl Pts',(10.6475718363526,-6.91097182865411,9.3260379894265));
#26042=CARTESIAN_POINT('Ctrl Pts',(9.62260863652896,-7.33414209133677,8.72329062200735));
#26043=CARTESIAN_POINT('Ctrl Pts',(8.83596460437641,-7.64982933055118,8.26196206072778));
#26044=CARTESIAN_POINT('Ctrl Pts',(8.38131550044836,-7.83228405538728,7.99533241831094));
#26045=CARTESIAN_POINT('Ctrl Pts',(7.99969688490427,-7.98693286596967,7.76911080499221));
#26046=CARTESIAN_POINT('Ctrl Pts',(7.59379043301555,-8.15376232311827,7.52350537407495));
#26047=CARTESIAN_POINT('Ctrl Pts',(7.36145773430845,-8.24925215291236,7.38292575944549));
#26048=CARTESIAN_POINT('Ctrl Pts',(7.13004605045667,-8.34517464654889,7.24116906982207));
#26049=CARTESIAN_POINT('Ctrl Pts',(6.9,-8.44145532612415,7.09789564133157));
#26050=CARTESIAN_POINT('',(6.9,-5.6597919716369,9.46599415782505));
#26051=CARTESIAN_POINT('Ctrl Pts',(6.90000000000001,-8.44145532612415,7.09789564133157));
#26052=CARTESIAN_POINT('Ctrl Pts',(6.90000000000001,-8.09681826844945,7.5077690000137));
#26053=CARTESIAN_POINT('Ctrl Pts',(6.90000000000001,-7.72210951819363,7.89280389060837));
#26054=CARTESIAN_POINT('Ctrl Pts',(6.90000000000001,-6.80464666682922,8.70687723936702));
#26055=CARTESIAN_POINT('Ctrl Pts',(6.90000000000001,-6.24868352466685,9.11389129061078));
#26056=CARTESIAN_POINT('Ctrl Pts',(6.90000000000001,-5.6597919716369,9.46599415782505));
#26057=CARTESIAN_POINT('',(37.5,1.5,32.3652591523689));
#26058=CARTESIAN_POINT('Ctrl Pts',(6.9,-5.6597919716369,9.46599415782505));
#26059=CARTESIAN_POINT('Ctrl Pts',(6.98893730997566,-5.61299197171187,9.50231572683753));
#26060=CARTESIAN_POINT('Ctrl Pts',(7.08052892388252,-5.56508220248504,9.53955640247964));
#26061=CARTESIAN_POINT('Ctrl Pts',(7.17490192378012,-5.51603067891051,9.57777162403489));
#26062=CARTESIAN_POINT('Ctrl Pts',(7.97363347620239,-5.10088016323476,9.90120844677132));
#26063=CARTESIAN_POINT('Ctrl Pts',(8.96286060501197,-4.58706675347826,10.2954119066179));
#26064=CARTESIAN_POINT('Ctrl Pts',(10.2403127965964,-4.0024828296383,10.8024441000946));
#26065=CARTESIAN_POINT('Ctrl Pts',(10.4394276407768,-3.91136447885181,10.8814745615582));
#26066=CARTESIAN_POINT('Ctrl Pts',(10.6449386760841,-3.81760465493997,10.9636620301547));
#26067=CARTESIAN_POINT('Ctrl Pts',(10.8572270226697,-3.72139879136416,11.0492678117694));
#26068=CARTESIAN_POINT('Ctrl Pts',(11.0079272576165,-3.65310372723407,11.1100380406097));
#26069=CARTESIAN_POINT('Ctrl Pts',(11.2445718661728,-3.54599023605203,11.2057391107691));
#26070=CARTESIAN_POINT('Ctrl Pts',(11.5512244264283,-3.40956688332716,11.3315975141146));
#26071=CARTESIAN_POINT('Ctrl Pts',(12.0044642694228,-3.20792989416164,11.5176192545635));
#26072=CARTESIAN_POINT('Ctrl Pts',(12.6082461582821,-2.94281490472512,11.7683139215994));
#26073=CARTESIAN_POINT('Ctrl Pts',(13.3027146141536,-2.65901005153359,12.0682094443783));
#26074=CARTESIAN_POINT('Ctrl Pts',(14.2466220417723,-2.27326825627017,12.4758213511068));
#26075=CARTESIAN_POINT('Ctrl Pts',(15.3788107202037,-1.8146998161318,12.9964429751969));
#26076=CARTESIAN_POINT('Ctrl Pts',(16.3720853361384,-1.45099516743194,13.4908337691235));
#26077=CARTESIAN_POINT('Ctrl Pts',(17.5300464833461,-1.02698770212797,14.0671953530399));
#26078=CARTESIAN_POINT('Ctrl Pts',(18.5522571217465,-0.660939172704794,
14.6297459826154));
#26079=CARTESIAN_POINT('Ctrl Pts',(19.459740928474,-0.371242885073753,15.1671394203612));
#26080=CARTESIAN_POINT('Ctrl Pts',(20.7212139011928,0.0314574545183544,
15.914158036459));
#26081=CARTESIAN_POINT('Ctrl Pts',(21.7483180915019,0.336055810070734,16.6062803213401));
#26082=CARTESIAN_POINT('Ctrl Pts',(22.5801692622301,0.547760951425958,17.2054151585246));
#26083=CARTESIAN_POINT('Ctrl Pts',(23.3330995247656,0.739380814773852,17.747707777841));
#26084=CARTESIAN_POINT('Ctrl Pts',(23.9217876539922,0.875119715010134,18.2069050147382));
#26085=CARTESIAN_POINT('Ctrl Pts',(24.4822919859555,0.991018194513003,18.6643830131721));
#26086=CARTESIAN_POINT('Ctrl Pts',(24.9418792866488,1.08604951953881,19.039493545664));
#26087=CARTESIAN_POINT('Ctrl Pts',(25.3626276504437,1.16248493476306,19.3999270896812));
#26088=CARTESIAN_POINT('Ctrl Pts',(25.7525302890144,1.22321331868058,19.7463071016619));
#26089=CARTESIAN_POINT('Ctrl Pts',(26.1776080055513,1.2894203155331,20.1239357965756));
#26090=CARTESIAN_POINT('Ctrl Pts',(26.5661459570286,1.33297321437855,20.4852396168503));
#26091=CARTESIAN_POINT('Ctrl Pts',(26.9267016829778,1.36638815232393,20.8313979296014));
#26092=CARTESIAN_POINT('Ctrl Pts',(27.1778777840728,1.38966620125619,21.0725442742603));
#26093=CARTESIAN_POINT('Ctrl Pts',(27.4154861117395,1.40780557009561,21.3064162460911));
#26094=CARTESIAN_POINT('Ctrl Pts',(27.6422281940027,1.42326116563352,21.5339888724078));
#26095=CARTESIAN_POINT('Ctrl Pts',(27.8555559931731,1.43780239304073,21.7480980798342));
#26096=CARTESIAN_POINT('Ctrl Pts',(28.1190837191602,1.45368682613675,22.0160369612575));
#26097=CARTESIAN_POINT('Ctrl Pts',(28.4603051775547,1.47251023690518,22.3749799381424));
#26098=CARTESIAN_POINT('Ctrl Pts',(28.6017730832288,1.48031428449229,22.5237950549738));
#26099=CARTESIAN_POINT('Ctrl Pts',(28.7540286646318,1.48853267939352,22.685688456893));
#26100=CARTESIAN_POINT('Ctrl Pts',(28.9157341130969,1.49763121638955,22.8599017516109));
#26101=CARTESIAN_POINT('Ctrl Pts',(29.4787137469316,1.52930789194493,23.4664276157693));
#26102=CARTESIAN_POINT('Ctrl Pts',(30.1711677436387,1.53976925233529,24.2477248210855));
#26103=CARTESIAN_POINT('Ctrl Pts',(30.8055547543725,1.53340754825755,24.9885333989119));
#26104=CARTESIAN_POINT('Ctrl Pts',(31.1893125644404,1.52955918190726,25.4366684847443));
#26105=CARTESIAN_POINT('Ctrl Pts',(31.5650207099025,1.5212245596794,25.8828713567903));
#26106=CARTESIAN_POINT('Ctrl Pts',(31.9311744366524,1.51382648741807,26.3192346641747));
#26107=CARTESIAN_POINT('Ctrl Pts',(32.1142513000274,1.51012745128741,26.5374163178669));
#26108=CARTESIAN_POINT('Ctrl Pts',(32.2949430642618,1.50666813405657,26.7531357746881));
#26109=CARTESIAN_POINT('Ctrl Pts',(32.4730466959732,1.50413682057757,26.9654180603372));
#26110=CARTESIAN_POINT('Ctrl Pts',(32.5932788659586,1.50242801032161,27.108723166515));
#26111=CARTESIAN_POINT('Ctrl Pts',(32.7123311760612,1.50114220273881,27.2504621963874));
#26112=CARTESIAN_POINT('Ctrl Pts',(32.8301302693026,1.50048655910809,27.390344014413));
#26113=CARTESIAN_POINT('Ctrl Pts',(32.8868306159462,1.50017097755213,27.4576734594278));
#26114=CARTESIAN_POINT('Ctrl Pts',(32.9387123022461,1.5,27.5192120661523));
#26115=CARTESIAN_POINT('Ctrl Pts',(33.,1.5,27.5917792275077));
#26116=CARTESIAN_POINT('Ctrl Pts',(33.0955022515303,1.5,27.7048578313807));
#26117=CARTESIAN_POINT('Ctrl Pts',(33.2417478451704,1.5,27.8775886863925));
#26118=CARTESIAN_POINT('Ctrl Pts',(33.3688392456061,1.5,28.026861129604));
#26119=CARTESIAN_POINT('Ctrl Pts',(34.266193218791,1.5,29.08082874302));
#26120=CARTESIAN_POINT('Ctrl Pts',(35.2319960543154,1.5,30.1809662912516));
#26121=CARTESIAN_POINT('Ctrl Pts',(36.3004607333866,1.5,31.2401426719198));
#26122=CARTESIAN_POINT('Ctrl Pts',(36.689171908737,1.5,31.6254747319285));
#26123=CARTESIAN_POINT('Ctrl Pts',(37.0893059759246,1.5,32.0028866146793));
#26124=CARTESIAN_POINT('Ctrl Pts',(37.5,1.5,32.3652591523689));
#26125=CARTESIAN_POINT('',(37.5,3.83741678103715,32.1719479119405));
#26126=CARTESIAN_POINT('Origin',(37.5,0.,0.));
#26127=CARTESIAN_POINT('',(36.8,4.53355051147315,31.4347259190859));
#26128=CARTESIAN_POINT('Ctrl Pts',(37.5,3.83741678103717,32.1719479119405));
#26129=CARTESIAN_POINT('Ctrl Pts',(37.2470086540956,4.04454785994596,31.9226755103027));
#26130=CARTESIAN_POINT('Ctrl Pts',(37.0122659037829,4.27613294009139,31.6748439028166));
#26131=CARTESIAN_POINT('Ctrl Pts',(36.8,4.53355051147315,31.4347259190859));
#26132=CARTESIAN_POINT('',(36.8,11.7911930472673,29.4900464626661));
#26133=CARTESIAN_POINT('Ctrl Pts',(36.8,4.53355051147315,31.4347259190859));
#26134=CARTESIAN_POINT('Ctrl Pts',(36.8,6.18280168905531,31.1968691126063));
#26135=CARTESIAN_POINT('Ctrl Pts',(36.8,7.81258162569765,30.8293258095436));
#26136=CARTESIAN_POINT('Ctrl Pts',(36.8,10.2137688485759,30.0846548283827));
#26137=CARTESIAN_POINT('Ctrl Pts',(36.8,11.0089139056503,29.8028301128151));
#26138=CARTESIAN_POINT('Ctrl Pts',(36.8,11.7911930472673,29.4900464626661));
#26139=CARTESIAN_POINT('',(37.5,12.7626735386834,29.7804325714888));
#26140=CARTESIAN_POINT('Ctrl Pts',(36.8,11.7911930472673,29.4900464626661));
#26141=CARTESIAN_POINT('Ctrl Pts',(37.0122659037828,12.1341821953296,29.5692859507915));
#26142=CARTESIAN_POINT('Ctrl Pts',(37.2470086540956,12.4586565616162,29.6681218786625));
#26143=CARTESIAN_POINT('Ctrl Pts',(37.5,12.7626735386834,29.7804325714888));
#26144=CARTESIAN_POINT('',(37.5,14.8835914705078,28.7791366260183));
#26145=CARTESIAN_POINT('Origin',(37.5,0.,0.));
#26146=CARTESIAN_POINT('',(6.9,-3.76156693666918,10.3676856018661));
#26147=CARTESIAN_POINT('Ctrl Pts',(37.5,14.8835914705078,28.7791366260183));
#26148=CARTESIAN_POINT('Ctrl Pts',(36.6490696321541,14.5081857198547,28.1289147924336));
#26149=CARTESIAN_POINT('Ctrl Pts',(35.8406537801186,14.0993459928369,27.4207836130862));
#26150=CARTESIAN_POINT('Ctrl Pts',(35.0774452370931,13.6847944140883,26.7027592163357));
#26151=CARTESIAN_POINT('Ctrl Pts',(34.6958409655804,13.4775186247139,26.3437470179604));
#26152=CARTESIAN_POINT('Ctrl Pts',(34.3255255042089,13.2688250041626,25.98227906395));
#26153=CARTESIAN_POINT('Ctrl Pts',(33.9666810635723,13.0622496974384,25.6244801371145));
#26154=CARTESIAN_POINT('Ctrl Pts',(33.71861455668,12.9194457162525,25.3771363861775));
#26155=CARTESIAN_POINT('Ctrl Pts',(33.467102416908,12.7724011203023,25.1224476750133));
#26156=CARTESIAN_POINT('Ctrl Pts',(33.2400985609625,12.638664651308,24.8908093158902));
#26157=CARTESIAN_POINT('Ctrl Pts',(33.1387264796258,12.5789425635218,24.7873676255104));
#26158=CARTESIAN_POINT('Ctrl Pts',(33.0532004124213,12.5283472490973,24.6997339703023));
#26159=CARTESIAN_POINT('Ctrl Pts',(33.,12.4968515080772,24.6451817466334));
#26160=CARTESIAN_POINT('Ctrl Pts',(32.9185691495566,12.4486427657032,24.5616817554726));
#26161=CARTESIAN_POINT('Ctrl Pts',(32.8516820632524,12.4091965179596,24.4928265641956));
#26162=CARTESIAN_POINT('Ctrl Pts',(32.7777321454818,12.3657029366776,24.4165289205543));
#26163=CARTESIAN_POINT('Ctrl Pts',(32.178869953925,12.0134826477248,23.7986543446369));
#26164=CARTESIAN_POINT('Ctrl Pts',(31.5692879870854,11.664059839844,23.1567007300813));
#26165=CARTESIAN_POINT('Ctrl Pts',(30.9513498040256,11.3096185478294,22.5260018679279));
#26166=CARTESIAN_POINT('Ctrl Pts',(30.6423807124957,11.1323979018221,22.2106524368512));
#26167=CARTESIAN_POINT('Ctrl Pts',(30.3347880606787,10.9558507301919,21.9015729507795));
#26168=CARTESIAN_POINT('Ctrl Pts',(30.0249306371694,10.7763433330083,21.5982641082636));
#26169=CARTESIAN_POINT('Ctrl Pts',(29.8700019254147,10.6865896344165,21.4466096870056));
#26170=CARTESIAN_POINT('Ctrl Pts',(29.7145097313378,10.5960927952669,21.2963965337993));
#26171=CARTESIAN_POINT('Ctrl Pts',(29.5580100720363,10.5043591957225,21.1475727378798));
#26172=CARTESIAN_POINT('Ctrl Pts',(29.4797602423856,10.4584923959504,21.07316083992));
#26173=CARTESIAN_POINT('Ctrl Pts',(29.4012586241155,10.4123158264222,20.9990965425402));
#26174=CARTESIAN_POINT('Ctrl Pts',(29.3224502420455,10.3657636829105,20.9253755287709));
#26175=CARTESIAN_POINT('Ctrl Pts',(29.2736528206492,10.3369390261396,20.8797281587809));
#26176=CARTESIAN_POINT('Ctrl Pts',(29.2247377938045,10.3079703168972,20.8342124356577));
#26177=CARTESIAN_POINT('Ctrl Pts',(29.1756921970763,10.2788413042909,20.7888277157836));
#26178=CARTESIAN_POINT('Ctrl Pts',(29.145528605794,10.2609266353026,20.7609156047673));
#26179=CARTESIAN_POINT('Ctrl Pts',(29.1181490968819,10.2446403152522,20.7356566760157));
#26180=CARTESIAN_POINT('Ctrl Pts',(29.0849408699094,10.2248462834623,20.7051394327917));
#26181=CARTESIAN_POINT('Ctrl Pts',(29.0475462332256,10.2025569083654,20.6707750199039));
#26182=CARTESIAN_POINT('Ctrl Pts',(28.9599837408864,10.150562007661,20.5905365514149));
#26183=CARTESIAN_POINT('Ctrl Pts',(28.8924081848889,10.1107110565592,20.529003052467));
#26184=CARTESIAN_POINT('Ctrl Pts',(28.4410807636115,9.84455228463784,20.1180296613881));
#26185=CARTESIAN_POINT('Ctrl Pts',(27.9936088568352,9.59004457960431,19.7235361017932));
#26186=CARTESIAN_POINT('Ctrl Pts',(27.5122543096508,9.31395242990228,19.3231338577684));
#26187=CARTESIAN_POINT('Ctrl Pts',(27.1397294106844,9.10028206826387,19.0132587223329));
#26188=CARTESIAN_POINT('Ctrl Pts',(26.7276341641442,8.86410488395679,18.6830630721424));
#26189=CARTESIAN_POINT('Ctrl Pts',(26.2530417505368,8.57522710561967,18.3335669465969));
#26190=CARTESIAN_POINT('Ctrl Pts',(25.8694949138829,8.34176749926266,18.0511179871691));
#26191=CARTESIAN_POINT('Ctrl Pts',(25.4447383161075,8.07732257195607,17.7540556187384));
#26192=CARTESIAN_POINT('Ctrl Pts',(24.9635886608316,7.77432947326916,17.4401876876742));
#26193=CARTESIAN_POINT('Ctrl Pts',(24.6119820459567,7.55291317047937,17.2108244541163));
#26194=CARTESIAN_POINT('Ctrl Pts',(24.2873626786171,7.34685978862235,17.001782341903));
#26195=CARTESIAN_POINT('Ctrl Pts',(23.6426616419067,6.93898570176839,16.625952931558));
#26196=CARTESIAN_POINT('Ctrl Pts',(23.5760533212499,6.89684553692024,16.5871235138108));
#26197=CARTESIAN_POINT('Ctrl Pts',(23.5065967305678,6.85292160238213,16.5469475098675));
#26198=CARTESIAN_POINT('Ctrl Pts',(23.4342591639586,6.80720851268154,16.5054784159948));
#26199=CARTESIAN_POINT('Ctrl Pts',(22.7443384436217,6.37121917472878,16.1099662574103));
#26200=CARTESIAN_POINT('Ctrl Pts',(21.7987837593123,5.75271743556738,15.6084067036781));
#26201=CARTESIAN_POINT('Ctrl Pts',(20.5610365528855,4.96573918168373,15.0432759423309));
#26202=CARTESIAN_POINT('Ctrl Pts',(19.7234582214102,4.43319430549857,14.6608543317656));
#26203=CARTESIAN_POINT('Ctrl Pts',(18.7603809281623,3.80221290992149,14.2617573685877));
#26204=CARTESIAN_POINT('Ctrl Pts',(17.6514222906382,3.10236545497629,13.8414640697512));
#26205=CARTESIAN_POINT('Ctrl Pts',(16.7565277906387,2.53761072285442,13.5023006881889));
#26206=CARTESIAN_POINT('Ctrl Pts',(15.7613807992389,1.89253400855812,13.1550491146656));
#26207=CARTESIAN_POINT('Ctrl Pts',(14.7199652846762,1.2417380338878,12.8103195459473));
#26208=CARTESIAN_POINT('Ctrl Pts',(13.7316067501733,0.624098151639976,12.4831529092169));
#26209=CARTESIAN_POINT('Ctrl Pts',(12.7260968661244,-0.0230322824212142,
12.1691790146818));
#26210=CARTESIAN_POINT('Ctrl Pts',(11.7781012037546,-0.615505739626224,
11.8786003909685));
#26211=CARTESIAN_POINT('Ctrl Pts',(10.6475718363527,-1.32205817373976,11.5320717298292));
#26212=CARTESIAN_POINT('Ctrl Pts',(9.62260863652904,-1.98990805505865,11.2216623289213));
#26213=CARTESIAN_POINT('Ctrl Pts',(8.83596460437641,-2.49396550450873,10.9799836949691));
#26214=CARTESIAN_POINT('Ctrl Pts',(8.3813155004462,-2.7852907524671,10.8403030136515));
#26215=CARTESIAN_POINT('Ctrl Pts',(7.99969688490053,-3.03233135775691,10.7217137549231));
#26216=CARTESIAN_POINT('Ctrl Pts',(7.59379043301053,-3.29961262120668,10.5924279410152));
#26217=CARTESIAN_POINT('Ctrl Pts',(7.36145773430507,-3.45259904692508,10.5184273383894));
#26218=CARTESIAN_POINT('Ctrl Pts',(7.130046050455,-3.60654870801926,10.4436236908379));
#26219=CARTESIAN_POINT('Ctrl Pts',(6.9,-3.76156693666918,10.3676856018661));
#26220=CARTESIAN_POINT('',(6.9,-0.168526548660249,11.02768739857));
#26221=CARTESIAN_POINT('Ctrl Pts',(6.90000000000001,-3.76156693666918,10.3676856018661));
#26222=CARTESIAN_POINT('Ctrl Pts',(6.90000000000001,-3.24481773355662,10.5551707158657));
#26223=CARTESIAN_POINT('Ctrl Pts',(6.89999999999998,-2.71398840242747,10.7040448708755));
#26224=CARTESIAN_POINT('Ctrl Pts',(6.89999999999998,-1.51153848953113,10.9457448952802));
#26225=CARTESIAN_POINT('Ctrl Pts',(6.90000000000001,-0.840414370027661,
11.0174195217678));
#26226=CARTESIAN_POINT('Ctrl Pts',(6.90000000000001,-0.168526548660249,
11.02768739857));
#26227=CARTESIAN_POINT('',(37.5,17.4816676818611,27.2791366260183));
#26228=CARTESIAN_POINT('Ctrl Pts',(6.9,-0.168526548660249,11.02768739857));
#26229=CARTESIAN_POINT('Ctrl Pts',(6.98893730997575,-0.10983577532176,11.0357428000776));
#26230=CARTESIAN_POINT('Ctrl Pts',(7.08052892388262,-0.0497243602608107,
11.0440392866244));
#26231=CARTESIAN_POINT('Ctrl Pts',(7.17490192378012,0.0118631160266181,
11.0526088775152));
#26232=CARTESIAN_POINT('Ctrl Pts',(7.9736334762095,0.53311242036889,11.1251381246871));
#26233=CARTESIAN_POINT('Ctrl Pts',(8.96286060502258,1.1751896159481,11.2096216302963));
#26234=CARTESIAN_POINT('Ctrl Pts',(10.2403127965964,1.93497024136951,11.3564324284624));
#26235=CARTESIAN_POINT('Ctrl Pts',(10.4394276407766,2.05339627863326,11.3793156403694));
#26236=CARTESIAN_POINT('Ctrl Pts',(10.6449386760836,2.17568840229328,11.4036121640907));
#26237=CARTESIAN_POINT('Ctrl Pts',(10.8572270226685,2.30180801494992,11.4296460138919));
#26238=CARTESIAN_POINT('Ctrl Pts',(11.0079272576413,2.39133838987524,11.4481270437995));
#26239=CARTESIAN_POINT('Ctrl Pts',(11.2445718661931,2.53195192940405,11.4774498561353));
#26240=CARTESIAN_POINT('Ctrl Pts',(11.5512244264873,2.71302722022868,11.5182347543553));
#26241=CARTESIAN_POINT('Ctrl Pts',(12.0044642694683,2.98066084540491,11.5785158126561));
#26242=CARTESIAN_POINT('Ctrl Pts',(12.6082461583042,3.33560449468488,11.6630662681815));
#26243=CARTESIAN_POINT('Ctrl Pts',(13.3027146141536,3.73133446864291,11.7808809827897));
#26244=CARTESIAN_POINT('Ctrl Pts',(14.2466220417547,4.26920261599668,11.9410123512669));
#26245=CARTESIAN_POINT('Ctrl Pts',(15.3788107201888,4.92664534657693,12.1625996834186));
#26246=CARTESIAN_POINT('Ctrl Pts',(16.3720853361384,5.48881820879721,12.4089023460099));
#26247=CARTESIAN_POINT('Ctrl Pts',(17.5300464833439,6.14420023710166,12.6960423867944));
#26248=CARTESIAN_POINT('Ctrl Pts',(18.5522571217461,6.74248287738888,13.0002012582105));
#26249=CARTESIAN_POINT('Ctrl Pts',(19.459740928474,7.26206394073251,13.3207494833101));
#26250=CARTESIAN_POINT('Ctrl Pts',(20.7212139012038,7.98432197298711,13.7663364121585));
#26251=CARTESIAN_POINT('Ctrl Pts',(21.748318091517,8.59417302928943,14.2134327156183));
#26252=CARTESIAN_POINT('Ctrl Pts',(22.5801692622301,9.0770824783983,14.6264461342272));
#26253=CARTESIAN_POINT('Ctrl Pts',(23.3330995247344,9.51417645756738,15.0002753871505));
#26254=CARTESIAN_POINT('Ctrl Pts',(23.9217876538942,9.86132841186279,15.3300824094945));
#26255=CARTESIAN_POINT('Ctrl Pts',(24.4822919858109,10.190438438562,15.668320738026));
#26256=CARTESIAN_POINT('Ctrl Pts',(24.9418792865584,10.4602932464676,15.9456603259067));
#26257=CARTESIAN_POINT('Ctrl Pts',(25.3626276504005,10.7067050298371,16.2195872238184));
#26258=CARTESIAN_POINT('Ctrl Pts',(25.7525302890143,10.9324873590558,16.489196921628));
#26259=CARTESIAN_POINT('Ctrl Pts',(26.1776080055349,11.1786386476857,16.7831294661836));
#26260=CARTESIAN_POINT('Ctrl Pts',(26.566145957002,11.3970084746262,17.0742513035944));
#26261=CARTESIAN_POINT('Ctrl Pts',(26.9267016829466,11.5990258161259,17.357325727191));
#26262=CARTESIAN_POINT('Ctrl Pts',(27.1778854594997,11.7397626706971,17.5545315892759));
#26263=CARTESIAN_POINT('Ctrl Pts',(27.4155006347601,11.8724116206269,17.7480067679658));
#26264=CARTESIAN_POINT('Ctrl Pts',(27.6422489803528,11.9995864201593,17.9373681845217));
#26265=CARTESIAN_POINT('Ctrl Pts',(27.8555706599243,12.1192306970096,18.1155167629388));
#26266=CARTESIAN_POINT('Ctrl Pts',(28.1190985482737,12.2669566516382,18.3396168643542));
#26267=CARTESIAN_POINT('Ctrl Pts',(28.4603120647663,12.462725193046,18.6410520014511));
#26268=CARTESIAN_POINT('Ctrl Pts',(28.6017780250768,12.5438901626918,18.7660259813188));
#26269=CARTESIAN_POINT('Ctrl Pts',(28.7540312887802,12.6319528845963,18.9021185408488));
#26270=CARTESIAN_POINT('Ctrl Pts',(28.9157341130969,12.7269375546994,19.0484400367167));
#26271=CARTESIAN_POINT('Ctrl Pts',(29.4787137469306,13.0576332925164,19.5578685053516));
#26272=CARTESIAN_POINT('Ctrl Pts',(30.1711677436355,13.4573416990294,20.2292610528638));
#26273=CARTESIAN_POINT('Ctrl Pts',(30.805554754367,13.8222365905986,20.8740009526392));
#26274=CARTESIAN_POINT('Ctrl Pts',(31.1893125644359,14.042971350493,21.2640215044733));
#26275=CARTESIAN_POINT('Ctrl Pts',(31.5650207098988,14.2588547919362,21.6546118380215));
#26276=CARTESIAN_POINT('Ctrl Pts',(31.9311744366496,14.4706295271116,22.0362125836274));
#26277=CARTESIAN_POINT('Ctrl Pts',(32.1142513000251,14.5765168946992,22.2270129564303));
#26278=CARTESIAN_POINT('Ctrl Pts',(32.2949430642599,14.6813807665084,22.4155611447439));
#26279=CARTESIAN_POINT('Ctrl Pts',(32.4730466959718,14.7853297275555,22.6006686536295));
#26280=CARTESIAN_POINT('Ctrl Pts',(32.5932788659518,14.8555024075494,22.7256289211939));
#26281=CARTESIAN_POINT('Ctrl Pts',(32.7123311760492,14.9252583804514,22.8490214255572));
#26282=CARTESIAN_POINT('Ctrl Pts',(32.8301302692855,14.9946314854212,22.9704904553051));
#26283=CARTESIAN_POINT('Ctrl Pts',(32.8868306159349,15.0280229062875,23.0289572558946));
#26284=CARTESIAN_POINT('Ctrl Pts',(32.9387123022399,15.0586441387491,23.0823367414128));
#26285=CARTESIAN_POINT('Ctrl Pts',(33.,15.0949277194305,23.1451817466334));
#26286=CARTESIAN_POINT('Ctrl Pts',(33.0955022515224,15.1514670213623,23.2431106902038));
#26287=CARTESIAN_POINT('Ctrl Pts',(33.2417478451566,15.2378324488647,23.3926999986554));
#26288=CARTESIAN_POINT('Ctrl Pts',(33.3688392455861,15.3124686704669,23.5219737265553));
#26289=CARTESIAN_POINT('Ctrl Pts',(34.2661932187784,15.8394524771795,24.4347364545476));
#26290=CARTESIAN_POINT('Ctrl Pts',(35.2319960543174,16.3895212513045,25.3874835189893));
#26291=CARTESIAN_POINT('Ctrl Pts',(36.3004607334107,16.9191094416485,26.3047571717535));
#26292=CARTESIAN_POINT('Ctrl Pts',(36.6891719087532,17.1117754716485,26.6384645246061));
#26293=CARTESIAN_POINT('Ctrl Pts',(37.0893059759329,17.3004814130199,26.9653128027515));
#26294=CARTESIAN_POINT('Ctrl Pts',(37.5,17.4816676818611,27.2791366260183));
#26295=CARTESIAN_POINT('',(37.5,19.4092743732571,25.9430157904517));
#26296=CARTESIAN_POINT('Origin',(37.5,0.,0.));
#26297=CARTESIAN_POINT('',(36.8,19.6435328718186,24.9564959511929));
#26298=CARTESIAN_POINT('Ctrl Pts',(37.5,19.4092743732572,25.9430157904516));
#26299=CARTESIAN_POINT('Ctrl Pts',(37.2470086540956,19.4640189486865,25.6235740187165));
#26300=CARTESIAN_POINT('Ctrl Pts',(37.0122659037829,19.5406617074869,25.2931530107));
#26301=CARTESIAN_POINT('Ctrl Pts',(36.8,19.6435328718186,24.9564959511929));
#26302=CARTESIAN_POINT('',(36.8,24.9564959511929,19.6435328718186));
#26303=CARTESIAN_POINT('Ctrl Pts',(36.8,19.6435328718186,24.9564959511929));
#26304=CARTESIAN_POINT('Ctrl Pts',(36.8,20.2288646216318,24.4957748831848));
#26305=CARTESIAN_POINT('Ctrl Pts',(36.8,20.7984186457787,24.0141222843114));
#26306=CARTESIAN_POINT('Ctrl Pts',(36.8,22.6602579716864,22.3234241559746));
#26307=CARTESIAN_POINT('Ctrl Pts',(36.8,23.8659348286794,21.029056769996));
#26308=CARTESIAN_POINT('Ctrl Pts',(36.8,24.9564959511929,19.6435328718186));
#26309=CARTESIAN_POINT('',(37.5,25.9430157904516,19.4092743732571));
#26310=CARTESIAN_POINT('Ctrl Pts',(36.8,24.9564959511929,19.6435328718186));
#26311=CARTESIAN_POINT('Ctrl Pts',(37.0122659037829,25.2931530107001,19.5406617074869));
#26312=CARTESIAN_POINT('Ctrl Pts',(37.2470086540957,25.6235740187166,19.4640189486865));
#26313=CARTESIAN_POINT('Ctrl Pts',(37.5,25.9430157904516,19.4092743732572));
#26314=CARTESIAN_POINT('',(37.5,27.2791366260183,17.4816676818611));
#26315=CARTESIAN_POINT('Origin',(37.5,0.,0.));
#26316=CARTESIAN_POINT('',(6.9,1.9262302757419,10.8594625780008));
#26317=CARTESIAN_POINT('Ctrl Pts',(37.5,27.2791366260183,17.4816676818611));
#26318=CARTESIAN_POINT('Ctrl Pts',(36.6490696321414,26.6289147924239,17.1062619312024));
#26319=CARTESIAN_POINT('Ctrl Pts',(35.8406537800949,25.9207836130653,16.6974222041782));
#26320=CARTESIAN_POINT('Ctrl Pts',(35.0774452370608,25.2027592163052,16.282870625424));
#26321=CARTESIAN_POINT('Ctrl Pts',(34.6958409655438,24.8437470179252,16.0755948360469));
#26322=CARTESIAN_POINT('Ctrl Pts',(34.3255255041686,24.4822790639105,15.8669012154931));
#26323=CARTESIAN_POINT('Ctrl Pts',(33.9666810635291,24.1244801370714,15.6603259087668));
#26324=CARTESIAN_POINT('Ctrl Pts',(33.718614556656,23.8771363861531,15.5175219275918));
#26325=CARTESIAN_POINT('Ctrl Pts',(33.4671024169005,23.6224476750055,15.3704773316512));
#26326=CARTESIAN_POINT('Ctrl Pts',(33.2400985609757,23.3908093159037,15.2367408626691));
#26327=CARTESIAN_POINT('Ctrl Pts',(33.1387264796202,23.2873676255047,15.1770187748718));
#26328=CARTESIAN_POINT('Ctrl Pts',(33.0532004124066,23.1997339702871,15.1264234604419));
#26329=CARTESIAN_POINT('Ctrl Pts',(33.,23.1451817466334,15.0949277194305));
#26330=CARTESIAN_POINT('Ctrl Pts',(32.9185691495926,23.0616817555095,15.0467189770778));
#26331=CARTESIAN_POINT('Ctrl Pts',(32.8516820633429,22.9930927072969,15.0068117561538));
#26332=CARTESIAN_POINT('Ctrl Pts',(32.7777321456298,22.9172773392435,14.9624828491874));
#26333=CARTESIAN_POINT('Ctrl Pts',(32.1788699540528,22.3033083333026,14.6034979145574));
#26334=CARTESIAN_POINT('Ctrl Pts',(31.5692879871913,21.6797224977148,14.2222611802267));
#26335=CARTESIAN_POINT('Ctrl Pts',(30.9513498041043,21.0574179035752,13.8532805894536));
#26336=CARTESIAN_POINT('Ctrl Pts',(30.6423807125608,20.7462656065053,13.668790294067));
#26337=CARTESIAN_POINT('Ctrl Pts',(30.3347880607311,20.4388315278584,13.4893931931471));
#26338=CARTESIAN_POINT('Ctrl Pts',(30.0249306372092,20.1317191404595,13.31647372892));
#26339=CARTESIAN_POINT('Ctrl Pts',(29.8700019254482,19.9781629467601,13.2300139968064));
#26340=CARTESIAN_POINT('Ctrl Pts',(29.7145097313649,19.8246838084848,13.1451740097183));
#26341=CARTESIAN_POINT('Ctrl Pts',(29.5580100720571,19.6708282829326,13.0621556215329));
#26342=CARTESIAN_POINT('Ctrl Pts',(29.4797602424031,19.5939005201566,13.0206464274402));
#26343=CARTESIAN_POINT('Ctrl Pts',(29.4012586241297,19.5168782891925,12.979593149158));
#26344=CARTESIAN_POINT('Ctrl Pts',(29.3224502420564,19.4397024434229,12.9390249501952));
#26345=CARTESIAN_POINT('Ctrl Pts',(29.2736528205926,19.3919158733428,12.9139054965186));
#26346=CARTESIAN_POINT('Ctrl Pts',(29.2247377936802,19.3440703735961,12.8889720786092));
#26347=CARTESIAN_POINT('Ctrl Pts',(29.1756921968838,19.2961515486883,12.8642322645241));
#26348=CARTESIAN_POINT('Ctrl Pts',(29.1455286056658,19.2666809347989,12.8490170018376));
#26349=CARTESIAN_POINT('Ctrl Pts',(29.1181490968165,19.2399471035866,12.8352852879233));
#26350=CARTESIAN_POINT('Ctrl Pts',(29.0849408699094,19.2075463476651,12.8187535959654));
#26351=CARTESIAN_POINT('Ctrl Pts',(29.0475462331044,19.1710609760345,12.8001378289065));
#26352=CARTESIAN_POINT('Ctrl Pts',(28.9599837408215,19.0859128369681,12.7566467272147));
#26353=CARTESIAN_POINT('Ctrl Pts',(28.8924081848413,19.020634151492,12.7232826295015));
#26354=CARTESIAN_POINT('Ctrl Pts',(28.4410807636646,18.5846471981269,12.5004486185587));
#26355=CARTESIAN_POINT('Ctrl Pts',(27.9936088569637,18.1669902803798,12.2860610268735));
#26356=CARTESIAN_POINT('Ctrl Pts',(27.5122543099026,17.7276863430492,12.0773485867127));
#26357=CARTESIAN_POINT('Ctrl Pts',(27.1397294108722,17.3877048140558,11.91582402821));
#26358=CARTESIAN_POINT('Ctrl Pts',(26.7276341642532,17.018071547485,11.7479547990402));
#26359=CARTESIAN_POINT('Ctrl Pts',(26.2530417505368,16.593147989986,11.5897211649258));
#26360=CARTESIAN_POINT('Ctrl Pts',(25.8694949138879,16.2497415604138,11.461842993969));
#26361=CARTESIAN_POINT('Ctrl Pts',(25.4447383161176,15.8721943512536,11.3368019000542));
#26362=CARTESIAN_POINT('Ctrl Pts',(24.9635886608481,15.4528606650926,11.2164808476639));
#26363=CARTESIAN_POINT('Ctrl Pts',(24.6119820458991,15.146426905221,11.1285546120848));
#26364=CARTESIAN_POINT('Ctrl Pts',(24.2873626784886,14.8634583858271,11.0505455233574));
#26365=CARTESIAN_POINT('Ctrl Pts',(23.6426616415564,14.3223143597134,10.9290047499034));
#26366=CARTESIAN_POINT('Ctrl Pts',(23.5760533210065,14.266405197652,10.9164475701653));
#26367=CARTESIAN_POINT('Ctrl Pts',(23.5065967304411,14.2082779526342,10.9036160974189));
#26368=CARTESIAN_POINT('Ctrl Pts',(23.4342591639586,14.1479547088373,10.8905593535265));
#26369=CARTESIAN_POINT('Ctrl Pts',(22.7443384436269,13.5726207871031,10.766030445664));
#26370=CARTESIAN_POINT('Ctrl Pts',(21.7987837593177,12.7862027918382,10.6409180002013));
#26371=CARTESIAN_POINT('Ctrl Pts',(20.5610365528855,11.8220942510713,10.544989531356));
#26372=CARTESIAN_POINT('Ctrl Pts',(19.7234582214113,11.1696860543579,10.480075139743));
#26373=CARTESIAN_POINT('Ctrl Pts',(18.7603809281633,10.4236916548838,10.4499377288461));
#26374=CARTESIAN_POINT('Ctrl Pts',(17.6514222906382,9.60745933070834,10.4358767824859));
#26375=CARTESIAN_POINT('Ctrl Pts',(16.7565277906389,8.94878569500229,10.4245300440805));
#26376=CARTESIAN_POINT('Ctrl Pts',(15.7613807992389,8.21650708627013,10.4463397170534));
#26377=CARTESIAN_POINT('Ctrl Pts',(14.7199652846762,7.48053645516581,10.4731931404428));
#26378=CARTESIAN_POINT('Ctrl Pts',(13.7316067501733,6.78206130838355,10.4986784628874));
#26379=CARTESIAN_POINT('Ctrl Pts',(12.7260968661244,6.06464296565697,10.5503343111255));
#26380=CARTESIAN_POINT('Ctrl Pts',(11.7781012037546,5.40625658879283,10.5949225697956));
#26381=CARTESIAN_POINT('Ctrl Pts',(10.6475718363527,4.62109990117509,10.6480961631663));
#26382=CARTESIAN_POINT('Ctrl Pts',(9.62260863652905,3.8875202375846,10.713198677066));
#26383=CARTESIAN_POINT('Ctrl Pts',(8.83596460437641,3.33015436441791,10.7559275652365));
#26384=CARTESIAN_POINT('Ctrl Pts',(8.38131550044648,3.00801895826358,10.7806231707768));
#26385=CARTESIAN_POINT('Ctrl Pts',(7.999696884901,2.73478088895225,10.8014421627469));
#26386=CARTESIAN_POINT('Ctrl Pts',(7.59379043301109,2.43866561789527,10.8231179952786));
#26387=CARTESIAN_POINT('Ctrl Pts',(7.36145773430546,2.26917518547593,10.8355248063685));
#26388=CARTESIAN_POINT('Ctrl Pts',(7.13004605045519,2.0984490442885,10.8477177778403));
#26389=CARTESIAN_POINT('Ctrl Pts',(6.9,1.9262302757419,10.8594625780008));
#26390=CARTESIAN_POINT('',(6.9,5.36789542693312,9.63452070648529));
#26391=CARTESIAN_POINT('Ctrl Pts',(6.90000000000001,1.9262302757419,10.8594625780008));
#26392=CARTESIAN_POINT('Ctrl Pts',(6.90000000000001,2.35749364924904,10.7829659225815));
#26393=CARTESIAN_POINT('Ctrl Pts',(6.90000000000001,2.78469328079872,10.6806923192591));
#26394=CARTESIAN_POINT('Ctrl Pts',(6.90000000000001,3.958690010018,10.3240838050858));
#26395=CARTESIAN_POINT('Ctrl Pts',(6.90000000000001,4.68344446130229,10.0158641401962));
#26396=CARTESIAN_POINT('Ctrl Pts',(6.90000000000001,5.36789542693312,9.6345207064853));
#26397=CARTESIAN_POINT('',(37.5,28.7791366260183,14.8835914705078));
#26398=CARTESIAN_POINT('Ctrl Pts',(6.9,5.36789542693312,9.6345207064853));
#26399=CARTESIAN_POINT('Ctrl Pts',(6.98893730997578,5.42275082836583,9.61215150215932));
#26400=CARTESIAN_POINT('Ctrl Pts',(7.08052892388264,5.47895708413941,9.58928076274048));
#26401=CARTESIAN_POINT('Ctrl Pts',(7.17490192378012,5.5365781986047,9.56590850800827));
#26402=CARTESIAN_POINT('Ctrl Pts',(7.97363347621182,6.02425796145741,9.36809602640473));
#26403=CARTESIAN_POINT('Ctrl Pts',(8.96286060502644,6.62255487682508,9.12022229067329));
#26404=CARTESIAN_POINT('Ctrl Pts',(10.2403127965964,7.35394959882411,8.86747385872511));
#26405=CARTESIAN_POINT('Ctrl Pts',(10.4394276407767,7.46795116151759,8.82807828292486));
#26406=CARTESIAN_POINT('Ctrl Pts',(10.6449386760836,7.58600750915056,8.78797362786116));
#26407=CARTESIAN_POINT('Ctrl Pts',(10.8572270226685,7.70824722252718,8.74745979681897));
#26408=CARTESIAN_POINT('Ctrl Pts',(11.0079272576493,7.79502331658132,8.71869965074289));
#26409=CARTESIAN_POINT('Ctrl Pts',(11.2445718661999,7.93145962009647,8.67378718137191));
#26410=CARTESIAN_POINT('Ctrl Pts',(11.551224426506,8.10866787106516,8.61857029390676));
#26411=CARTESIAN_POINT('Ctrl Pts',(12.0044642694828,8.37058591852268,8.53695840917511));
#26412=CARTESIAN_POINT('Ctrl Pts',(12.6082461583112,8.72025136346947,8.43270942692314));
#26413=CARTESIAN_POINT('Ctrl Pts',(13.3027146141536,9.12187093125612,8.33687497573541));
#26414=CARTESIAN_POINT('Ctrl Pts',(14.2466220417493,9.66774409498637,8.20661873510328));
#26415=CARTESIAN_POINT('Ctrl Pts',(15.3788107201844,10.3478998672786,8.06979762861289));
#26416=CARTESIAN_POINT('Ctrl Pts',(16.3720853361384,10.9579071785779,8.00201556032625));
#26417=CARTESIAN_POINT('Ctrl Pts',(17.5300464833445,11.669054684666,7.92299511593705));
#26418=CARTESIAN_POINT('Ctrl Pts',(18.5522571217475,12.3392620855066,7.88726310522634));
#26419=CARTESIAN_POINT('Ctrl Pts',(19.459740928474,12.9495065982363,7.9050754796287));
#26420=CARTESIAN_POINT('Ctrl Pts',(20.7212139012143,13.7977938666874,7.92983606347863));
#26421=CARTESIAN_POINT('Ctrl Pts',(21.7483180915291,14.5494885257019,8.01210729206323));
#26422=CARTESIAN_POINT('Ctrl Pts',(22.5801692622301,15.1742070856531,8.12833268012627));
#26423=CARTESIAN_POINT('Ctrl Pts',(23.3330995246905,15.7396562018834,8.23353132024499));
#26424=CARTESIAN_POINT('Ctrl Pts',(23.9217876537976,16.2052021244058,8.34557660278196));
#26425=CARTESIAN_POINT('Ctrl Pts',(24.4822919856751,16.6593389323991,8.47394457446099));
#26426=CARTESIAN_POINT('Ctrl Pts',(24.9418792864744,17.0317098453591,8.57920029909639));
#26427=CARTESIAN_POINT('Ctrl Pts',(25.3626276503609,17.3820721585412,8.69322205979346));
#26428=CARTESIAN_POINT('Ctrl Pts',(25.7525302890143,17.7124102403086,8.81381974260611));
#26429=CARTESIAN_POINT('Ctrl Pts',(26.177608005523,18.0725497817041,8.94529714887164));
#26430=CARTESIAN_POINT('Ctrl Pts',(26.5661459569821,18.4072245179529,9.08823114219187));
#26431=CARTESIAN_POINT('Ctrl Pts',(26.926701682922,18.7237138794904,9.23237211343583));
#26432=CARTESIAN_POINT('Ctrl Pts',(27.1778777840053,18.9441917644501,9.33278590403371));
#26433=CARTESIAN_POINT('Ctrl Pts',(27.4154861116651,19.1558005177017,9.43401273572152));
#26434=CARTESIAN_POINT('Ctrl Pts',(27.6422281939261,19.3606119910642,9.5344141105115));
#26435=CARTESIAN_POINT('Ctrl Pts',(27.8555559931215,19.5533066176051,9.62887564189806));
#26436=CARTESIAN_POINT('Ctrl Pts',(28.119083719114,19.7932907121314,9.74908876002559));
#26437=CARTESIAN_POINT('Ctrl Pts',(28.460305177545,20.113556154042,9.91225869657406));
#26438=CARTESIAN_POINT('Ctrl Pts',(28.6017730832218,20.2463358494812,9.97990775152821));
#26439=CARTESIAN_POINT('Ctrl Pts',(28.7540286646281,20.390648845702,10.0537371137266));
#26440=CARTESIAN_POINT('Ctrl Pts',(28.9157341130969,20.5460712531062,10.1329641969115));
#26441=CARTESIAN_POINT('Ctrl Pts',(29.4787137469279,21.0871763972938,10.4087943232505));
#26442=CARTESIAN_POINT('Ctrl Pts',(30.1711677436301,21.7690303051937,10.7903831220494));
#26443=CARTESIAN_POINT('Ctrl Pts',(30.8055547543591,22.4074085008889,11.1662968083021));
#26444=CARTESIAN_POINT('Ctrl Pts',(31.1893125644294,22.793580686374,11.393697134242));
#26445=CARTESIAN_POINT('Ctrl Pts',(31.5650207098935,23.1758363976956,11.6240165648465));
#26446=CARTESIAN_POINT('Ctrl Pts',(31.9311744366457,23.5500390710414,11.8486051370574));
#26447=CARTESIAN_POINT('Ctrl Pts',(32.1142513000217,23.7371404077143,11.9608994231628));
#26448=CARTESIAN_POINT('Ctrl Pts',(32.2949430642572,23.9222292787978,12.0717550081758));
#26449=CARTESIAN_POINT('Ctrl Pts',(32.4730466959697,24.1048054742049,12.1800883327787));
#26450=CARTESIAN_POINT('Ctrl Pts',(32.5932788659409,24.2280569315044,12.2532207589509));
#26451=CARTESIAN_POINT('Ctrl Pts',(32.7123311760297,24.3501636282761,12.3252038159099));
#26452=CARTESIAN_POINT('Ctrl Pts',(32.8301302692575,24.4709770143846,12.3957125289548));
#26453=CARTESIAN_POINT('Ctrl Pts',(32.8868306159163,24.5291282334276,12.4296505531158));
#26454=CARTESIAN_POINT('Ctrl Pts',(32.9387123022288,24.5823367414014,12.4605679273892));
#26455=CARTESIAN_POINT('Ctrl Pts',(33.,24.6451817466334,12.4968515080772));
#26456=CARTESIAN_POINT('Ctrl Pts',(33.0955022515085,24.7431106901895,12.5533908100007));
#26457=CARTESIAN_POINT('Ctrl Pts',(33.2417478451339,24.8926999986323,12.6397562374981));
#26458=CARTESIAN_POINT('Ctrl Pts',(33.3688392455532,25.0219737265219,12.7143924590943));
#26459=CARTESIAN_POINT('Ctrl Pts',(34.2661932187446,25.9347364545141,13.2413762658068));
#26460=CARTESIAN_POINT('Ctrl Pts',(35.2319960542717,26.8874835189453,13.7914450399258));
#26461=CARTESIAN_POINT('Ctrl Pts',(36.3004607333495,27.804757171701,14.3210332302649));
#26462=CARTESIAN_POINT('Ctrl Pts',(36.6891719087116,28.1384645245721,14.5136992602756));
#26463=CARTESIAN_POINT('Ctrl Pts',(37.0893059759116,28.4653128027352,14.7024052016572));
#26464=CARTESIAN_POINT('Ctrl Pts',(37.5,28.7791366260183,14.8835914705078));
#26465=CARTESIAN_POINT('',(37.5,29.7804325714888,12.7626735386834));
#26466=CARTESIAN_POINT('Origin',(37.5,0.,0.));
#26467=CARTESIAN_POINT('',(36.8,29.4900464626661,11.7911930472673));
#26468=CARTESIAN_POINT('Ctrl Pts',(37.5,29.7804325714888,12.7626735386834));
#26469=CARTESIAN_POINT('Ctrl Pts',(37.2470086540956,29.6681218786625,12.4586565616162));
#26470=CARTESIAN_POINT('Ctrl Pts',(37.0122659037829,29.5692859507915,12.1341821953297));
#26471=CARTESIAN_POINT('Ctrl Pts',(36.8,29.4900464626661,11.7911930472673));
#26472=CARTESIAN_POINT('',(36.8,31.4347259190859,4.53355051147315));
#26473=CARTESIAN_POINT('Ctrl Pts',(36.8,29.4900464626661,11.7911930472673));
#26474=CARTESIAN_POINT('Ctrl Pts',(36.8,30.4236973716148,9.45611053488411));
#26475=CARTESIAN_POINT('Ctrl Pts',(36.8,31.0761743714062,7.01967470941751));
#26476=CARTESIAN_POINT('Ctrl Pts',(36.8,31.4347259190859,4.53355051147315));
#26477=CARTESIAN_POINT('',(37.5,32.1719479119405,3.83741678103715));
#26478=CARTESIAN_POINT('Ctrl Pts',(36.8,31.4347259190859,4.53355051147314));
#26479=CARTESIAN_POINT('Ctrl Pts',(37.0122659037829,31.6748439028166,4.27613294009139));
#26480=CARTESIAN_POINT('Ctrl Pts',(37.2470086540956,31.9226755103027,4.04454785994593));
#26481=CARTESIAN_POINT('Ctrl Pts',(37.5,32.1719479119405,3.83741678103717));
#26482=CARTESIAN_POINT('',(37.5,32.3652591523689,1.5));
#26483=CARTESIAN_POINT('Origin',(37.5,0.,0.));
#26484=CARTESIAN_POINT('',(6.9,7.09789564133157,8.44145532612415));
#26485=CARTESIAN_POINT('Ctrl Pts',(37.5,32.3652591523689,1.5));
#26486=CARTESIAN_POINT('Ctrl Pts',(36.64906963214,31.6144476510502,1.5));
#26487=CARTESIAN_POINT('Ctrl Pts',(35.8406537800928,30.7967681970009,1.5));
#26488=CARTESIAN_POINT('Ctrl Pts',(35.0774452370603,29.9676650394942,1.5));
#26489=CARTESIAN_POINT('Ctrl Pts',(34.6958409655441,29.5531134607409,1.5));
#26490=CARTESIAN_POINT('Ctrl Pts',(34.3255255041702,29.1357262196348,1.5));
#26491=CARTESIAN_POINT('Ctrl Pts',(33.9666810635328,28.7225756061845,1.5));
#26492=CARTESIAN_POINT('Ctrl Pts',(33.7186145566461,28.436967643819,1.5));
#26493=CARTESIAN_POINT('Ctrl Pts',(33.4671024168721,28.1428784519157,1.5));
#26494=CARTESIAN_POINT('Ctrl Pts',(33.2400985609432,27.8754055139464,1.5));
#26495=CARTESIAN_POINT('Ctrl Pts',(33.1387264796055,27.7559613383729,1.5));
#26496=CARTESIAN_POINT('Ctrl Pts',(33.0532004124081,27.6547707095322,1.5));
#26497=CARTESIAN_POINT('Ctrl Pts',(33.,27.5917792275077,1.5));
#26498=CARTESIAN_POINT('Ctrl Pts',(32.9185691495653,27.4953617427699,1.5));
#26499=CARTESIAN_POINT('Ctrl Pts',(32.8516820633046,27.4160082741213,1.49973385699152));
#26500=CARTESIAN_POINT('Ctrl Pts',(32.7777321455755,27.3281857858874,1.49925158146312));
#26501=CARTESIAN_POINT('Ctrl Pts',(32.1788699540067,26.6169805623007,1.4953460114673));
#26502=CARTESIAN_POINT('Ctrl Pts',(31.569287987155,25.8863210200885,1.47697823247539));
#26503=CARTESIAN_POINT('Ctrl Pts',(30.9513498040767,25.1628991372958,1.46858396443269));
#26504=CARTESIAN_POINT('Ctrl Pts',(30.6423807125376,24.8011881958995,1.46438683041133));
#26505=CARTESIAN_POINT('Ctrl Pts',(30.3347880607121,24.4452439233475,1.46274142297315));
#26506=CARTESIAN_POINT('Ctrl Pts',(30.0249306371945,24.0928170619347,1.46654496784322));
#26507=CARTESIAN_POINT('Ctrl Pts',(29.8700019254357,23.9166036312283,1.46844674027826));
#26508=CARTESIAN_POINT('Ctrl Pts',(29.7145097313546,23.7412668049894,1.47171272534086));
#26509=CARTESIAN_POINT('Ctrl Pts',(29.558010072049,23.5665148172585,1.47674445496712));
#26510=CARTESIAN_POINT('Ctrl Pts',(29.4797602423961,23.479138823393,1.47926031978024));
#26511=CARTESIAN_POINT('Ctrl Pts',(29.4012586241238,23.3919089755822,1.48221825336132));
#26512=CARTESIAN_POINT('Ctrl Pts',(29.3224502420517,23.3047886331069,1.48567308535852));
#26513=CARTESIAN_POINT('Ctrl Pts',(29.2736528206717,23.2508445227123,1.4878122853818));
#26514=CARTESIAN_POINT('Ctrl Pts',(29.2247377938435,23.1969423956128,1.49014206193805));
#26515=CARTESIAN_POINT('Ctrl Pts',(29.1756921971318,23.1430735689731,1.4926761669043));
#26516=CARTESIAN_POINT('Ctrl Pts',(29.145528605831,23.109943637245,1.49423466984117));
#26517=CARTESIAN_POINT('Ctrl Pts',(29.118149096899,23.0799256032268,1.49570957236425));
#26518=CARTESIAN_POINT('Ctrl Pts',(29.0849408699094,23.0435998794277,1.49759308512661));
#26519=CARTESIAN_POINT('Ctrl Pts',(29.0475462332514,23.0026947373604,1.49971404374963));
#26520=CARTESIAN_POINT('Ctrl Pts',(28.9599837410406,22.9072087350758,1.50462371437525));
#26521=CARTESIAN_POINT('Ctrl Pts',(28.8924081851533,22.8339936863707,1.50836890091433));
#26522=CARTESIAN_POINT('Ctrl Pts',(28.441080763973,22.3450009035549,1.53338246329392));
#26523=CARTESIAN_POINT('Ctrl Pts',(27.9936088572591,21.8761056068567,1.55654582151093));
#26524=CARTESIAN_POINT('Ctrl Pts',(27.5122543102273,21.3913010170864,1.59544751490245));
#26525=CARTESIAN_POINT('Ctrl Pts',(27.1397294111092,21.0161060968145,1.62555390840296));
#26526=CARTESIAN_POINT('Ctrl Pts',(26.7276341643888,20.612059683191,1.66499152471603));
#26527=CARTESIAN_POINT('Ctrl Pts',(26.2530417505368,20.1649482705455,1.74041895661093));
#26528=CARTESIAN_POINT('Ctrl Pts',(25.869494913883,19.8036104932301,1.80137642675969));
#26529=CARTESIAN_POINT('Ctrl Pts',(25.4447383161079,19.4141244720077,1.88186126749374));
#26530=CARTESIAN_POINT('Ctrl Pts',(24.9635886608324,18.9908103209297,1.98732702259573));
#26531=CARTESIAN_POINT('Ctrl Pts',(24.6119820459508,18.6814677825737,2.06439754884626));
#26532=CARTESIAN_POINT('Ctrl Pts',(24.2873626786048,18.3974053120019,2.1383239559649));
#26533=CARTESIAN_POINT('Ctrl Pts',(23.642661641875,17.8679904517118,2.30363857155873));
#26534=CARTESIAN_POINT('Ctrl Pts',(23.5760533212279,17.8132931071125,2.32071831596085));
#26535=CARTESIAN_POINT('Ctrl Pts',(23.5065967305564,17.7565376998146,2.33866955713063));
#26536=CARTESIAN_POINT('Ctrl Pts',(23.4342591639586,17.697767866208,2.3575237071575));
#26537=CARTESIAN_POINT('Ctrl Pts',(22.7443384436221,17.1372496203922,2.53734547031137));
#26538=CARTESIAN_POINT('Ctrl Pts',(21.7987837593128,16.3936354357686,2.82220391184387));
#26539=CARTESIAN_POINT('Ctrl Pts',(20.5610365528854,15.5107287130397,3.22118169125961));
#26540=CARTESIAN_POINT('Ctrl Pts',(19.7234582214103,14.9132694452415,3.49116827740851));
#26541=CARTESIAN_POINT('Ctrl Pts',(18.7603809281624,14.2521506387677,3.83806571370465));
#26542=CARTESIAN_POINT('Ctrl Pts',(17.6514222906382,13.5382422374622,4.23400473904287));
#26543=CARTESIAN_POINT('Ctrl Pts',(16.7565277906387,12.9621407669349,4.55351499318671));
#26544=CARTESIAN_POINT('Ctrl Pts',(15.7613807992389,12.3388737256115,4.93854202839549));
#26545=CARTESIAN_POINT('Ctrl Pts',(14.7199652846762,11.7149311743306,5.32978309078145));
#26546=CARTESIAN_POINT('Ctrl Pts',(13.7316067501733,11.1227766145274,5.7010916008333));
#26547=CARTESIAN_POINT('Ctrl Pts',(12.7260968661244,10.5273020287043,6.10453604902479));
#26548=CARTESIAN_POINT('Ctrl Pts',(11.7781012037546,9.97941683016941,6.47234380217571));
#26549=CARTESIAN_POINT('Ctrl Pts',(10.6475718363527,9.32603798942654,6.91097182865408));
#26550=CARTESIAN_POINT('Ctrl Pts',(9.62260863652904,8.72329062200739,7.33414209133673));
#26551=CARTESIAN_POINT('Ctrl Pts',(8.83596460437641,8.26196206072778,7.64982933055117));
#26552=CARTESIAN_POINT('Ctrl Pts',(8.38131550044699,7.99533241831014,7.83228405538783));
#26553=CARTESIAN_POINT('Ctrl Pts',(7.99969688490189,7.7691108049908,7.98693286597064));
#26554=CARTESIAN_POINT('Ctrl Pts',(7.59379043301236,7.52350537407302,8.15376232311959));
#26555=CARTESIAN_POINT('Ctrl Pts',(7.36145773430631,7.38292575944418,8.24925215291325));
#26556=CARTESIAN_POINT('Ctrl Pts',(7.13004605045561,7.24116906982141,8.34517464654934));
#26557=CARTESIAN_POINT('Ctrl Pts',(6.9,7.09789564133157,8.44145532612415));
#26558=CARTESIAN_POINT('',(6.9,9.46599415782505,5.6597919716369));
#26559=CARTESIAN_POINT('Ctrl Pts',(6.90000000000001,7.09789564133157,8.44145532612415));
#26560=CARTESIAN_POINT('Ctrl Pts',(6.90000000000001,7.5077690000137,8.09681826844945));
#26561=CARTESIAN_POINT('Ctrl Pts',(6.90000000000001,7.89280389060836,7.72210951819363));
#26562=CARTESIAN_POINT('Ctrl Pts',(6.90000000000001,8.70687723936702,6.80464666682922));
#26563=CARTESIAN_POINT('Ctrl Pts',(6.90000000000001,9.11389129061078,6.24868352466685));
#26564=CARTESIAN_POINT('Ctrl Pts',(6.90000000000001,9.46599415782505,5.6597919716369));
#26565=CARTESIAN_POINT('Ctrl Pts',(6.9,9.46599415782505,5.6597919716369));
#26566=CARTESIAN_POINT('Ctrl Pts',(6.98893730997541,9.50231572683742,5.61299197171201));
#26567=CARTESIAN_POINT('Ctrl Pts',(7.08052892388223,9.53955640247952,5.56508220248518));
#26568=CARTESIAN_POINT('Ctrl Pts',(7.17490192378012,9.57777162403489,5.51603067891051));
#26569=CARTESIAN_POINT('Ctrl Pts',(7.97363347618104,9.90120844676267,5.10088016324584));
#26570=CARTESIAN_POINT('Ctrl Pts',(8.96286060497891,10.2954119066048,4.58706675349338));
#26571=CARTESIAN_POINT('Ctrl Pts',(10.2403127965964,10.8024441000946,4.00248282963831));
#26572=CARTESIAN_POINT('Ctrl Pts',(10.439427640778,10.8814745615587,3.91136447885127));
#26573=CARTESIAN_POINT('Ctrl Pts',(10.6449386760872,10.9636620301559,3.81760465493853));
#26574=CARTESIAN_POINT('Ctrl Pts',(10.8572270226758,11.0492678117718,3.7213987913614));
#26575=CARTESIAN_POINT('Ctrl Pts',(11.0079272575452,11.1100380405809,3.6531037272664));
#26576=CARTESIAN_POINT('Ctrl Pts',(11.2445718661156,11.2057391107462,3.54599023607825));
#26577=CARTESIAN_POINT('Ctrl Pts',(11.5512244262555,11.3315975140437,3.40956688340402));
#26578=CARTESIAN_POINT('Ctrl Pts',(12.00446426929,11.5176192545082,3.20792989421962));
#26579=CARTESIAN_POINT('Ctrl Pts',(12.6082461582178,11.7683139215717,2.9428149047514));
#26580=CARTESIAN_POINT('Ctrl Pts',(13.3027146141536,12.0682094443783,2.65901005153358));
#26581=CARTESIAN_POINT('Ctrl Pts',(14.2466220418243,12.4758213511293,2.2732682562489));
#26582=CARTESIAN_POINT('Ctrl Pts',(15.3788272822924,12.9964524563587,1.81469502494887));
#26583=CARTESIAN_POINT('Ctrl Pts',(16.3720352459916,13.4908088373714,1.45101350883608));
#26584=CARTESIAN_POINT('Ctrl Pts',(17.5299186899716,14.0671303026852,1.02703301151891));
#26585=CARTESIAN_POINT('Ctrl Pts',(18.5521204793993,14.6296677023245,0.660984941495812));
#26586=CARTESIAN_POINT('Ctrl Pts',(19.4596586821662,15.1670907158914,0.371269140680975));
#26587=CARTESIAN_POINT('Ctrl Pts',(19.880385055414,15.4162350876749,0.236959557042726));
#26588=CARTESIAN_POINT('Ctrl Pts',(20.27477945539,15.6592719448482,0.112950602571839));
#26589=CARTESIAN_POINT('Ctrl Pts',(20.644698628669,15.8947820241755,3.27862736959617E-15));
#26590=CARTESIAN_POINT('Origin',(155.122410108095,0.,0.));
#26591=CARTESIAN_POINT('',(172.622410108095,-2.87422589366703,0.00219230231809422));
#26592=CARTESIAN_POINT('',(172.819589891905,-2.86687004470951,-0.000292364604808637));
#26593=CARTESIAN_POINT('',(155.122410108095,-2.872,-3.13019997719247E-13));
#26594=CARTESIAN_POINT('',(173.058,2.64453949578291,-1.13133757670319));
#26595=CARTESIAN_POINT('Ctrl Pts',(172.622410108095,-2.87422589366703,0.00219230231809418));
#26596=CARTESIAN_POINT('Ctrl Pts',(172.666840602011,-2.86739304828907,-0.797854553035495));
#26597=CARTESIAN_POINT('Ctrl Pts',(172.763886767894,-2.10484582911375,-2.55670607422354));
#26598=CARTESIAN_POINT('Ctrl Pts',(172.909083398529,0.776574793634194,-3.25358644951632));
#26599=CARTESIAN_POINT('Ctrl Pts',(173.009849535248,2.29916206741707,-1.92522559845067));
#26600=CARTESIAN_POINT('Ctrl Pts',(173.058,2.64453949578291,-1.13133757670319));
#26601=CARTESIAN_POINT('',(173.058,-0.208958374082678,-2.86438831129802));
#26602=CARTESIAN_POINT('Origin',(173.058,0.,0.));
#26603=CARTESIAN_POINT('Ctrl Pts',(172.819589891905,-2.86687004470951,-0.000292364604808186));
#26604=CARTESIAN_POINT('Ctrl Pts',(172.846444255971,-2.86629933481412,-0.486922577646889));
#26605=CARTESIAN_POINT('Ctrl Pts',(172.925914292002,-2.51836703171159,-1.92675278851268));
#26606=CARTESIAN_POINT('Ctrl Pts',(173.005384328034,-1.15590801223433,-2.79530792301902));
#26607=CARTESIAN_POINT('Ctrl Pts',(173.058,-0.208958374082637,-2.86438831129802));
#26608=CARTESIAN_POINT('Origin',(155.122410108095,0.,0.));
#26609=CARTESIAN_POINT('',(171.622410108095,-2.87356135069046,-0.00235826304143971));
#26610=CARTESIAN_POINT('',(171.819589891905,-2.87424241070289,0.00217440260399965));
#26611=CARTESIAN_POINT('',(155.122410108095,-2.872,-3.13019997719247E-13));
#26612=CARTESIAN_POINT('Ctrl Pts',(171.622410108095,-2.87356135069046,-0.00235826304143932));
#26613=CARTESIAN_POINT('Ctrl Pts',(171.631864231582,-2.87506858034527,-0.172686974326985));
#26614=CARTESIAN_POINT('Ctrl Pts',(171.693934027035,-2.78407626657566,-1.28935039450392));
#26615=CARTESIAN_POINT('Ctrl Pts',(171.808619494454,-1.32187438082726,-3.1195126227806));
#26616=CARTESIAN_POINT('Ctrl Pts',(171.966466510352,1.88769284474709,-2.81340333947064));
#26617=CARTESIAN_POINT('Ctrl Pts',(172.124313526251,3.38780638409936,0.0405047390324093));
#26618=CARTESIAN_POINT('Ctrl Pts',(172.282160542149,1.81982745081448,2.85778026783241));
#26619=CARTESIAN_POINT('Ctrl Pts',(172.440007558048,-1.39600998068982,3.08694689555915));
#26620=CARTESIAN_POINT('Ctrl Pts',(172.553424080029,-2.79854500868001,1.24309116568133));
#26621=CARTESIAN_POINT('Ctrl Pts',(172.614224930045,-2.87548467004053,0.149580399589383));
#26622=CARTESIAN_POINT('Ctrl Pts',(172.622410108095,-2.87422589366703,0.00219230231809418));
#26623=CARTESIAN_POINT('Ctrl Pts',(171.819589891905,-2.87424241070289,0.00217440260399975));
#26624=CARTESIAN_POINT('Ctrl Pts',(171.864083557507,-2.86748730574921,-0.798952851534598));
#26625=CARTESIAN_POINT('Ctrl Pts',(171.961192895075,-2.10336452521562,-2.55874939692443));
#26626=CARTESIAN_POINT('Ctrl Pts',(172.110917904609,0.869829193827587,-3.27436767007504));
#26627=CARTESIAN_POINT('Ctrl Pts',(172.268764920508,3.21691519730582,-1.0637880016197));
#26628=CARTESIAN_POINT('Ctrl Pts',(172.426611936406,2.65009699317679,2.11067616912988));
#26629=CARTESIAN_POINT('Ctrl Pts',(172.584458952305,-0.315318796737369,
3.37266439996185));
#26630=CARTESIAN_POINT('Ctrl Pts',(172.715451604138,-2.54150147573075,1.88704582168949));
#26631=CARTESIAN_POINT('Ctrl Pts',(172.793828584004,-2.8674175249366,0.466530484796677));
#26632=CARTESIAN_POINT('Ctrl Pts',(172.819589891905,-2.86687004470951,-0.000292364604808186));
#26633=CARTESIAN_POINT('Origin',(155.122410108095,0.,0.));
#26634=CARTESIAN_POINT('',(170.622410108095,-2.8674942953205,0.000227582857409601));
#26635=CARTESIAN_POINT('',(170.819589891905,-2.87352757519475,-0.00236597882501771));
#26636=CARTESIAN_POINT('',(155.122410108095,-2.872,-3.13019997719247E-13));
#26637=CARTESIAN_POINT('Ctrl Pts',(170.622410108095,-2.8674942953205,0.000227582857409842));
#26638=CARTESIAN_POINT('Ctrl Pts',(170.649503533118,-2.86714338948619,-0.490524080721482));
#26639=CARTESIAN_POINT('Ctrl Pts',(170.729212630108,-2.51520696034054,-1.93479179819195));
#26640=CARTESIAN_POINT('Ctrl Pts',(170.861537399063,-0.231273610377281,
-3.38012116904044));
#26641=CARTESIAN_POINT('Ctrl Pts',(171.019384414961,2.70261668758891,-2.04317595483142));
#26642=CARTESIAN_POINT('Ctrl Pts',(171.17723143086,3.18901336295286,1.14407252761205));
#26643=CARTESIAN_POINT('Ctrl Pts',(171.335078446758,0.787432799006144,3.2952476962313));
#26644=CARTESIAN_POINT('Ctrl Pts',(171.48347133917,-2.14069437351883,2.51213187458012));
#26645=CARTESIAN_POINT('Ctrl Pts',(171.579248559616,-2.86668029335008,0.775254906480099));
#26646=CARTESIAN_POINT('Ctrl Pts',(171.622410108095,-2.87356135069046,-0.00235826304143932));
#26647=CARTESIAN_POINT('Ctrl Pts',(170.819589891905,-2.87352757519475,-0.0023659788250179));
#26648=CARTESIAN_POINT('Ctrl Pts',(170.829107187077,-2.87504739493669,-0.173837919594956));
#26649=CARTESIAN_POINT('Ctrl Pts',(170.891240154216,-2.78334526035724,-1.29165779848931));
#26650=CARTESIAN_POINT('Ctrl Pts',(171.00598879332,-1.31816431809934,-3.12108180407131));
#26651=CARTESIAN_POINT('Ctrl Pts',(171.163835809219,1.89105258537231,-2.81115929350443));
#26652=CARTESIAN_POINT('Ctrl Pts',(171.321682825117,3.38773384709925,0.04455010635921));
#26653=CARTESIAN_POINT('Ctrl Pts',(171.479529841016,1.81646787669691,2.85992243368512));
#26654=CARTESIAN_POINT('Ctrl Pts',(171.637376856914,-1.39977490155201,3.08532882114793));
#26655=CARTESIAN_POINT('Ctrl Pts',(171.75073020721,-2.79913811640008,1.2407317623324));
#26656=CARTESIAN_POINT('Ctrl Pts',(171.811467885541,-2.87547550769956,0.148414559907332));
#26657=CARTESIAN_POINT('Ctrl Pts',(171.819589891905,-2.87424241070289,0.00217440260399975));
#26658=CARTESIAN_POINT('Origin',(155.122410108095,0.,0.));
#26659=CARTESIAN_POINT('',(169.622410108095,-2.87435821711997,0.00213318404225128));
#26660=CARTESIAN_POINT('',(169.819589891905,-2.86749724845603,0.000245826060064624));
#26661=CARTESIAN_POINT('',(155.122410108095,-2.872,-3.13019997719247E-13));
#26662=CARTESIAN_POINT('Ctrl Pts',(169.622410108095,-2.87435821711997,0.00213318404225135));
#26663=CARTESIAN_POINT('Ctrl Pts',(169.667142834655,-2.8676581248492,-0.803206107247127));
#26664=CARTESIAN_POINT('Ctrl Pts',(169.76449123318,-2.09660336467381,-2.56705067797754));
#26665=CARTESIAN_POINT('Ctrl Pts',(169.914455303673,0.884666035299711,-3.27048502929561));
#26666=CARTESIAN_POINT('Ctrl Pts',(170.072302319571,3.22149246026824,-1.04913899093533));
#26667=CARTESIAN_POINT('Ctrl Pts',(170.230149335469,2.64092984065361,2.12230909777109));
#26668=CARTESIAN_POINT('Ctrl Pts',(170.387996351368,-0.331263356051794,
3.37179046643881));
#26669=CARTESIAN_POINT('Ctrl Pts',(170.518749942243,-2.54479782657719,1.87742068807177));
#26670=CARTESIAN_POINT('Ctrl Pts',(170.596887861152,-2.86782485173223,0.46252000748776));
#26671=CARTESIAN_POINT('Ctrl Pts',(170.622410108095,-2.8674942953205,0.000227582857409842));
#26672=CARTESIAN_POINT('Ctrl Pts',(169.819589891905,-2.86749724845603,0.00024582606006452));
#26673=CARTESIAN_POINT('Ctrl Pts',(169.846746488614,-2.86711729687761,-0.491648894342766));
#26674=CARTESIAN_POINT('Ctrl Pts',(169.926518757289,-2.51399256659462,-1.93709682488167));
#26675=CARTESIAN_POINT('Ctrl Pts',(170.05890669793,-0.227248629623084,-3.38039427118688));
#26676=CARTESIAN_POINT('Ctrl Pts',(170.216753713828,2.7050479786207,-2.03995651601825));
#26677=CARTESIAN_POINT('Ctrl Pts',(170.374600729726,3.18764860462061,1.14786927643015));
#26678=CARTESIAN_POINT('Ctrl Pts',(170.532447745625,0.783509087420058,3.2961828100762));
#26679=CARTESIAN_POINT('Ctrl Pts',(170.680777466351,-2.1424393721461,2.50991663454912));
#26680=CARTESIAN_POINT('Ctrl Pts',(170.776491515111,-2.86664518238132,0.77413219414454));
#26681=CARTESIAN_POINT('Ctrl Pts',(170.819589891905,-2.87352757519475,-0.0023659788250179));
#26682=CARTESIAN_POINT('Origin',(155.122410108095,0.,0.));
#26683=CARTESIAN_POINT('',(168.622410108095,-2.87340176099087,-0.00239232046765291));
#26684=CARTESIAN_POINT('',(168.819589891905,-2.87438921400676,0.00212235973350849));
#26685=CARTESIAN_POINT('',(155.122410108095,-2.872,-3.13019997719247E-13));
#26686=CARTESIAN_POINT('Ctrl Pts',(168.622410108095,-2.87340176099087,-0.00239232046765273));
#26687=CARTESIAN_POINT('Ctrl Pts',(168.632166464225,-2.87496866737895,-0.178191256630362));
#26688=CARTESIAN_POINT('Ctrl Pts',(168.694538492321,-2.78056600145512,-1.300389394094));
#26689=CARTESIAN_POINT('Ctrl Pts',(168.809526192383,-1.30408738860609,-3.12698935027992));
#26690=CARTESIAN_POINT('Ctrl Pts',(168.967373208282,1.9037022189819,-2.80261024323187));
#26691=CARTESIAN_POINT('Ctrl Pts',(169.12522022418,3.38749585741264,0.0598174693970574));
#26692=CARTESIAN_POINT('Ctrl Pts',(169.283067240079,1.80356748292359,2.86807437987086));
#26693=CARTESIAN_POINT('Ctrl Pts',(169.440914255977,-1.41367467356012,3.07899825141338));
#26694=CARTESIAN_POINT('Ctrl Pts',(169.554028545316,-2.80175403108198,1.23199926250765));
#26695=CARTESIAN_POINT('Ctrl Pts',(169.614527162688,-2.87553892899808,0.144052672416806));
#26696=CARTESIAN_POINT('Ctrl Pts',(169.622410108095,-2.87435821711997,0.00213318404225135));
#26697=CARTESIAN_POINT('Ctrl Pts',(168.819589891905,-2.87438921400676,0.00212235973350855));
#26698=CARTESIAN_POINT('Ctrl Pts',(168.86438579015,-2.86770274060997,-0.804331700826428));
#26699=CARTESIAN_POINT('Ctrl Pts',(168.961797360362,-2.09480143196574,-2.56925069528134));
#26700=CARTESIAN_POINT('Ctrl Pts',(169.111824602539,0.888559801961863,-3.26942943049782));
#26701=CARTESIAN_POINT('Ctrl Pts',(169.269671618437,3.2227395907929,-1.04530227652681));
#26702=CARTESIAN_POINT('Ctrl Pts',(169.427518634336,2.63840092301917,2.12545239707543));
#26703=CARTESIAN_POINT('Ctrl Pts',(169.585365650234,-0.335278112564125,
3.37139376458444));
#26704=CARTESIAN_POINT('Ctrl Pts',(169.716056069424,-2.54596312587379,1.87511246443019));
#26705=CARTESIAN_POINT('Ctrl Pts',(169.794130816648,-2.86785344978467,0.461392885089547));
#26706=CARTESIAN_POINT('Ctrl Pts',(169.819589891905,-2.86749724845603,0.00024582606006452));
#26707=CARTESIAN_POINT('Origin',(155.122410108095,0.,0.));
#26708=CARTESIAN_POINT('',(167.622410108095,-2.8675098280091,0.000314758925835955));
#26709=CARTESIAN_POINT('',(167.819589891905,-2.87336857678864,-0.00239892095949074));
#26710=CARTESIAN_POINT('',(155.122410108095,-2.872,-3.13019997719247E-13));
#26711=CARTESIAN_POINT('Ctrl Pts',(167.622410108095,-2.8675098280091,0.000314758925835865));
#26712=CARTESIAN_POINT('Ctrl Pts',(167.649805765761,-2.86701892352542,-0.49590461907087));
#26713=CARTESIAN_POINT('Ctrl Pts',(167.729817095394,-2.50937904224953,-1.94581795526478));
#26714=CARTESIAN_POINT('Ctrl Pts',(167.862444096993,-0.212013665700137,
-3.38138381723357));
#26715=CARTESIAN_POINT('Ctrl Pts',(168.020291112891,2.7142128214914,-2.02774630403978));
#26716=CARTESIAN_POINT('Ctrl Pts',(168.17813812879,3.18244355869507,1.16222171275988));
#26717=CARTESIAN_POINT('Ctrl Pts',(168.335985144688,0.76864799350228,3.29967976870115));
#26718=CARTESIAN_POINT('Ctrl Pts',(168.484075804457,-2.14901785032668,2.50152539436281));
#26719=CARTESIAN_POINT('Ctrl Pts',(168.579550792259,-2.86651839850613,0.769885979781707));
#26720=CARTESIAN_POINT('Ctrl Pts',(168.622410108095,-2.87340176099087,-0.00239232046765273));
#26721=CARTESIAN_POINT('Ctrl Pts',(167.819589891905,-2.87336857678864,-0.00239892095949067));
#26722=CARTESIAN_POINT('Ctrl Pts',(167.82940941972,-2.87494778079546,-0.17934145242446));
#26723=CARTESIAN_POINT('Ctrl Pts',(167.891844619502,-2.7798280420658,-1.30269698359132));
#26724=CARTESIAN_POINT('Ctrl Pts',(168.00689549125,-1.30036303375706,-3.12854012314479));
#26725=CARTESIAN_POINT('Ctrl Pts',(168.164742507148,1.90703818343888,-2.80034153070911));
#26726=CARTESIAN_POINT('Ctrl Pts',(168.322589523047,3.38742237645021,0.0638511173542441));
#26727=CARTESIAN_POINT('Ctrl Pts',(168.480436538945,1.80015110090155,2.87022008487266));
#26728=CARTESIAN_POINT('Ctrl Pts',(168.638283554844,-1.41734007501666,3.07731285922868));
#26729=CARTESIAN_POINT('Ctrl Pts',(168.751334672497,-2.80244519982093,1.22969466039503));
#26730=CARTESIAN_POINT('Ctrl Pts',(168.811770118184,-2.8755564349132,0.142900612140373));
#26731=CARTESIAN_POINT('Ctrl Pts',(168.819589891905,-2.87438921400676,0.00212235973350855));
#26732=CARTESIAN_POINT('Origin',(155.122410108095,0.,0.));
#26733=CARTESIAN_POINT('',(166.622410108095,-2.87450488446859,0.00208020559110183));
#26734=CARTESIAN_POINT('',(166.819589891905,-2.86751383367012,0.000332938889392731));
#26735=CARTESIAN_POINT('',(155.122410108095,-2.872,-3.13019997719247E-13));
#26736=CARTESIAN_POINT('Ctrl Pts',(166.622410108095,-2.87450488446859,0.00208020559110164));
#26737=CARTESIAN_POINT('Ctrl Pts',(166.667445067298,-2.86787466431953,-0.808592444296684));
#26738=CARTESIAN_POINT('Ctrl Pts',(166.765095698467,-2.08796138916789,-2.57756977721455));
#26739=CARTESIAN_POINT('Ctrl Pts',(166.915362001602,0.903283370530585,-3.26539208463793));
#26740=CARTESIAN_POINT('Ctrl Pts',(167.0732090175,3.22741704709102,-1.03076938159775));
#26741=CARTESIAN_POINT('Ctrl Pts',(167.231056033399,2.62879635362904,2.13731982750353));
#26742=CARTESIAN_POINT('Ctrl Pts',(167.388903049297,-0.350466791168255,
3.36984856368669));
#26743=CARTESIAN_POINT('Ctrl Pts',(167.519354407529,-2.55035531167827,1.86637599950059));
#26744=CARTESIAN_POINT('Ctrl Pts',(167.597190093795,-2.86796174700476,0.457126563237285));
#26745=CARTESIAN_POINT('Ctrl Pts',(167.622410108095,-2.8675098280091,0.000314758925835865));
#26746=CARTESIAN_POINT('Ctrl Pts',(166.819589891905,-2.86751383367012,0.000332938889392939));
#26747=CARTESIAN_POINT('Ctrl Pts',(166.847048721257,-2.86699333758779,-0.497029011732394));
#26748=CARTESIAN_POINT('Ctrl Pts',(166.927123222575,-2.50815544873722,-1.94812225213107));
#26749=CARTESIAN_POINT('Ctrl Pts',(167.059813395859,-0.207987114903346,
-3.38163402539736));
#26750=CARTESIAN_POINT('Ctrl Pts',(167.217660411758,2.71662557150557,-2.02451298487645));
#26751=CARTESIAN_POINT('Ctrl Pts',(167.375507427656,3.18105751740887,1.16601045991334));
#26752=CARTESIAN_POINT('Ctrl Pts',(167.533354443555,0.764718362261322,3.3005928479761));
#26753=CARTESIAN_POINT('Ctrl Pts',(167.681381931638,-2.15075093712925,2.4993067245601));
#26754=CARTESIAN_POINT('Ctrl Pts',(167.776793747754,-2.86648598084416,0.768764237317345));
#26755=CARTESIAN_POINT('Ctrl Pts',(167.819589891905,-2.87336857678864,-0.00239892095949067));
#26756=CARTESIAN_POINT('Origin',(155.122410108095,0.,0.));
#26757=CARTESIAN_POINT('',(165.622410108095,-2.87324197174522,-0.00242261092417198));
#26758=CARTESIAN_POINT('',(165.819589891905,-2.87453532874939,0.00206875392256244));
#26759=CARTESIAN_POINT('',(155.122410108095,-2.872,-3.13019997719247E-13));
#26760=CARTESIAN_POINT('Ctrl Pts',(165.622410108095,-2.87324197174522,-0.00242261092417158));
#26761=CARTESIAN_POINT('Ctrl Pts',(165.632468696868,-2.8748671275446,-0.183693495603892));
#26762=CARTESIAN_POINT('Ctrl Pts',(165.695142957607,-2.7770207161025,-1.31143012210531));
#26763=CARTESIAN_POINT('Ctrl Pts',(165.810432890313,-1.28625201732507,-3.13436788871701));
#26764=CARTESIAN_POINT('Ctrl Pts',(165.968279906211,1.91963757364734,-2.79171952383016));
#26765=CARTESIAN_POINT('Ctrl Pts',(166.12612692211,3.38710011122917,0.0791147925766244));
#26766=CARTESIAN_POINT('Ctrl Pts',(166.283973938008,1.78719902416841,2.87830261819438));
#26767=CARTESIAN_POINT('Ctrl Pts',(166.441820953907,-1.43119254050081,3.07089469469534));
#26768=CARTESIAN_POINT('Ctrl Pts',(166.554633010602,-2.80504650106343,1.22097398834813));
#26769=CARTESIAN_POINT('Ctrl Pts',(166.614829395332,-2.87562094619924,0.138540338178042));
#26770=CARTESIAN_POINT('Ctrl Pts',(166.622410108095,-2.87450488446859,0.00208020559110164));
#26771=CARTESIAN_POINT('Ctrl Pts',(165.819589891905,-2.87453532874939,0.00206875392256263));
#26772=CARTESIAN_POINT('Ctrl Pts',(165.864688022793,-2.86792123297805,-0.809718743524386));
#26773=CARTESIAN_POINT('Ctrl Pts',(165.962401825648,-2.08614859619317,-2.57976665801494));
#26774=CARTESIAN_POINT('Ctrl Pts',(166.112731300469,0.90717106151226,-3.26431432108579));
#26775=CARTESIAN_POINT('Ctrl Pts',(166.270578316367,3.22864229756116,-1.02692562344606));
#26776=CARTESIAN_POINT('Ctrl Pts',(166.428425332265,2.62624957467685,2.14044866633159));
#26777=CARTESIAN_POINT('Ctrl Pts',(166.586272348164,-0.354479232189763,
3.36942900142401));
#26778=CARTESIAN_POINT('Ctrl Pts',(166.71666053471,-2.55151157895156,1.86406723401458));
#26779=CARTESIAN_POINT('Ctrl Pts',(166.794433049291,-2.86799069442252,0.455998989096919));
#26780=CARTESIAN_POINT('Ctrl Pts',(166.819589891905,-2.86751383367012,0.000332938889392939));
#26781=CARTESIAN_POINT('Origin',(155.122410108095,0.,0.));
#26782=CARTESIAN_POINT('',(164.622410108095,-2.86753036214098,0.00040157864720313));
#26783=CARTESIAN_POINT('',(164.819589891905,-2.87320857308323,-0.00242853002640792));
#26784=CARTESIAN_POINT('',(155.122410108095,-2.872,-3.13019997719247E-13));
#26785=CARTESIAN_POINT('Ctrl Pts',(164.622410108095,-2.86753036214098,0.000401578647203325));
#26786=CARTESIAN_POINT('Ctrl Pts',(164.650107998405,-2.86689688195682,-0.501283178591449));
#26787=CARTESIAN_POINT('Ctrl Pts',(164.73042156068,-2.50350697808224,-1.95684059811892));
#26788=CARTESIAN_POINT('Ctrl Pts',(164.863350794922,-0.192746751143198,
-3.38253677050477));
#26789=CARTESIAN_POINT('Ctrl Pts',(165.021197810821,2.72572068544879,-2.01225074451711));
#26790=CARTESIAN_POINT('Ctrl Pts',(165.179044826719,3.1757708308709,1.18033298000295));
#26791=CARTESIAN_POINT('Ctrl Pts',(165.336891842617,0.749837507567218,3.30400514923002));
#26792=CARTESIAN_POINT('Ctrl Pts',(165.484680269743,-2.15728879001875,2.49090483660323));
#26793=CARTESIAN_POINT('Ctrl Pts',(165.579853024902,-2.86636606776747,0.764519978515341));
#26794=CARTESIAN_POINT('Ctrl Pts',(165.622410108095,-2.87324197174522,-0.00242261092417158));
#26795=CARTESIAN_POINT('Ctrl Pts',(164.819589891905,-2.87320857308323,-0.00242853002640802));
#26796=CARTESIAN_POINT('Ctrl Pts',(164.829711652364,-2.87484571022488,-0.184843366841589));
#26797=CARTESIAN_POINT('Ctrl Pts',(164.892449084789,-2.77627531036844,-1.31373812678202));
#26798=CARTESIAN_POINT('Ctrl Pts',(165.007802189179,-1.28251888829241,-3.13589741905954));
#26799=CARTESIAN_POINT('Ctrl Pts',(165.165649205078,1.92296055931244,-2.78943184340823));
#26800=CARTESIAN_POINT('Ctrl Pts',(165.323496220976,3.38700365205358,0.0831479564798997));
#26801=CARTESIAN_POINT('Ctrl Pts',(165.481343236875,1.78377047374568,2.88042882548487));
#26802=CARTESIAN_POINT('Ctrl Pts',(165.639190252773,-1.43484828107338,3.06918844843256));
#26803=CARTESIAN_POINT('Ctrl Pts',(165.751939137783,-2.80573043323553,1.21866986550307));
#26804=CARTESIAN_POINT('Ctrl Pts',(165.812072350827,-2.87563785197317,0.13738801745482));
#26805=CARTESIAN_POINT('Ctrl Pts',(165.819589891905,-2.87453532874939,0.00206875392256263));
#26806=CARTESIAN_POINT('Origin',(155.122410108095,0.,0.));
#26807=CARTESIAN_POINT('',(163.622410108095,-2.87464881776804,0.00202424674990214));
#26808=CARTESIAN_POINT('',(163.819589891905,-2.86753540926279,0.000419670536143391));
#26809=CARTESIAN_POINT('',(155.122410108095,-2.872,-3.13019997719247E-13));
#26810=CARTESIAN_POINT('Ctrl Pts',(163.622410108095,-2.87464881776804,0.00202424674990246));
#26811=CARTESIAN_POINT('Ctrl Pts',(163.667747299941,-2.86810059116501,-0.813982217531092));
#26812=CARTESIAN_POINT('Ctrl Pts',(163.765700163753,-2.07926741161996,-2.58807376981798));
#26813=CARTESIAN_POINT('Ctrl Pts',(163.916268699531,0.921871390857911,-3.26019316185573));
#26814=CARTESIAN_POINT('Ctrl Pts',(164.07411571543,3.23323688492365,-1.01236631703268));
#26815=CARTESIAN_POINT('Ctrl Pts',(164.231962731328,2.61657755392199,2.15226118726438));
#26816=CARTESIAN_POINT('Ctrl Pts',(164.389809747227,-0.369658862607259,
3.36779729781782));
#26817=CARTESIAN_POINT('Ctrl Pts',(164.519958872816,-2.55586969631235,1.85532880014071));
#26818=CARTESIAN_POINT('Ctrl Pts',(164.597492326438,-2.868100258286,0.451730943503979));
#26819=CARTESIAN_POINT('Ctrl Pts',(164.622410108095,-2.86753036214098,0.000401578647203325));
#26820=CARTESIAN_POINT('Ctrl Pts',(163.819589891905,-2.86753540926279,0.000419670536143772));
#26821=CARTESIAN_POINT('Ctrl Pts',(163.8473509539,-2.86687181424791,-0.502407163892982));
#26822=CARTESIAN_POINT('Ctrl Pts',(163.927727687861,-2.50227413339466,-1.95914414506922));
#26823=CARTESIAN_POINT('Ctrl Pts',(164.060720093789,-0.188718840271762,
-3.38276403566928));
#26824=CARTESIAN_POINT('Ctrl Pts',(164.218567109687,2.72811497634857,-2.00900373257834));
#26825=CARTESIAN_POINT('Ctrl Pts',(164.376414125585,3.17436322788575,1.18411376950773));
#26826=CARTESIAN_POINT('Ctrl Pts',(164.534261141484,0.74590273835584,3.30489582689142));
#26827=CARTESIAN_POINT('Ctrl Pts',(164.681986396924,-2.15901119308368,2.48868340770977));
#26828=CARTESIAN_POINT('Ctrl Pts',(164.777095980397,-2.86633542477008,0.763398715632628));
#26829=CARTESIAN_POINT('Ctrl Pts',(164.819589891905,-2.87320857308323,-0.00242853002640802));
#26830=CARTESIAN_POINT('Origin',(155.122410108095,0.,0.));
#26831=CARTESIAN_POINT('',(162.622410108095,-2.8730812386835,-0.00244963452792444));
#26832=CARTESIAN_POINT('',(162.819589891905,-2.87467866166092,0.0020121790497752));
#26833=CARTESIAN_POINT('',(155.122410108095,-2.872,-3.13019997719247E-13));
#26834=CARTESIAN_POINT('Ctrl Pts',(162.622410108095,-2.8730812386835,-0.00244963452792442));
#26835=CARTESIAN_POINT('Ctrl Pts',(162.632770929511,-2.87476306855881,-0.189194165208951));
#26836=CARTESIAN_POINT('Ctrl Pts',(162.695747422894,-2.7734397513437,-1.32247281514995));
#26837=CARTESIAN_POINT('Ctrl Pts',(162.811339588242,-1.26837490053319,-3.14164470072457));
#26838=CARTESIAN_POINT('Ctrl Pts',(162.969186604141,1.9355106261794,-2.78073819872344));
#26839=CARTESIAN_POINT('Ctrl Pts',(163.127033620039,3.38659443611677,0.0984095480937175));
#26840=CARTESIAN_POINT('Ctrl Pts',(163.284880635938,1.77077256165387,2.88843744069124));
#26841=CARTESIAN_POINT('Ctrl Pts',(163.442727651836,-1.44866395801099,3.0626914716721));
#26842=CARTESIAN_POINT('Ctrl Pts',(163.555237475889,-2.80830440148675,1.20995102409985));
#26843=CARTESIAN_POINT('Ctrl Pts',(163.615131627975,-2.87570007690456,0.133026776600459));
#26844=CARTESIAN_POINT('Ctrl Pts',(163.622410108095,-2.87464881776804,0.00202424674990246));
#26845=CARTESIAN_POINT('Ctrl Pts',(162.819589891905,-2.87467866166092,0.00201217904977503));
#26846=CARTESIAN_POINT('Ctrl Pts',(162.864990255437,-2.86814913610333,-0.815109254849669));
#26847=CARTESIAN_POINT('Ctrl Pts',(162.963006290934,-2.07744373508779,-2.59026746179106));
#26848=CARTESIAN_POINT('Ctrl Pts',(163.113637998398,0.925752878818704,-3.25909326792743));
#26849=CARTESIAN_POINT('Ctrl Pts',(163.271485014297,3.23444021792712,-1.00851564110162));
#26850=CARTESIAN_POINT('Ctrl Pts',(163.429332030195,2.61401299155246,2.15537546652226));
#26851=CARTESIAN_POINT('Ctrl Pts',(163.587179046093,-0.37366884830378,3.36735488380693));
#26852=CARTESIAN_POINT('Ctrl Pts',(163.717264999997,-2.55701697759514,1.85301952789162));
#26853=CARTESIAN_POINT('Ctrl Pts',(163.794735281934,-2.868129529015,0.450602911181542));
#26854=CARTESIAN_POINT('Ctrl Pts',(163.819589891905,-2.86753540926279,0.000419670536143772));
#26855=CARTESIAN_POINT('Origin',(155.122410108095,0.,0.));
#26856=CARTESIAN_POINT('',(161.622410108095,-2.86755587111262,0.000487937565173562));
#26857=CARTESIAN_POINT('',(161.819589891905,-2.87304766888017,-0.00245486878760248));
#26858=CARTESIAN_POINT('',(155.122410108095,-2.872,-3.13019997719247E-13));
#26859=CARTESIAN_POINT('Ctrl Pts',(161.622410108095,-2.86755587111262,0.000487937565173541));
#26860=CARTESIAN_POINT('Ctrl Pts',(161.650410231048,-2.86677736484341,-0.506659802481027));
#26861=CARTESIAN_POINT('Ctrl Pts',(161.731026025967,-2.49759059547312,-1.96785959265111));
#26862=CARTESIAN_POINT('Ctrl Pts',(161.864257492852,-0.173473580959878,
-3.38357994299221));
#26863=CARTESIAN_POINT('Ctrl Pts',(162.02210450875,2.73714008569463,-1.99668987706511));
#26864=CARTESIAN_POINT('Ctrl Pts',(162.179951524649,3.16899503288228,1.1984059393451));
#26865=CARTESIAN_POINT('Ctrl Pts',(162.337798540547,0.731002685534005,3.30822329772906));
#26866=CARTESIAN_POINT('Ctrl Pts',(162.485284735029,-2.16550866044979,2.48027117452657));
#26867=CARTESIAN_POINT('Ctrl Pts',(162.580155257545,-2.86622218116522,0.759156218698579));
#26868=CARTESIAN_POINT('Ctrl Pts',(162.622410108095,-2.8730812386835,-0.00244963452792442));
#26869=CARTESIAN_POINT('Ctrl Pts',(161.819589891905,-2.87304766888017,-0.00245486878760231));
#26870=CARTESIAN_POINT('Ctrl Pts',(161.830013885007,-2.87474113114852,-0.190343703764303));
#26871=CARTESIAN_POINT('Ctrl Pts',(161.893053550075,-2.77268687039962,-1.32478122490515));
#26872=CARTESIAN_POINT('Ctrl Pts',(162.008708887109,-1.26463311846787,-3.14315293890823));
#26873=CARTESIAN_POINT('Ctrl Pts',(162.166555903007,1.93882052518752,-2.77843162464046));
#26874=CARTESIAN_POINT('Ctrl Pts',(162.324402918906,3.38647500189316,0.102442097028211));
#26875=CARTESIAN_POINT('Ctrl Pts',(162.482249934804,1.76733195403479,2.89054408130007));
#26876=CARTESIAN_POINT('Ctrl Pts',(162.640096950703,-1.4523099189108,3.0609644266349));
#26877=CARTESIAN_POINT('Ctrl Pts',(162.75254360307,-2.80898112495851,1.20764738811918));
#26878=CARTESIAN_POINT('Ctrl Pts',(162.81237458347,-2.87571637451529,0.131874204714068));
#26879=CARTESIAN_POINT('Ctrl Pts',(162.819589891905,-2.87467866166092,0.00201217904977503));
#26880=CARTESIAN_POINT('Origin',(155.122410108095,0.,0.));
#26881=CARTESIAN_POINT('',(160.622410108095,-2.87478978750438,0.00196536333635101));
#26882=CARTESIAN_POINT('',(160.819589891905,-2.86756195538547,0.000505920555084749));
#26883=CARTESIAN_POINT('',(155.122410108095,-2.872,-3.13019997719247E-13));
#26884=CARTESIAN_POINT('Ctrl Pts',(160.622410108095,-2.87478978750438,0.00196536333635124));
#26885=CARTESIAN_POINT('Ctrl Pts',(160.668049532584,-2.86833601734048,-0.819375583152982));
#26886=CARTESIAN_POINT('Ctrl Pts',(160.76630462904,-2.07052132275083,-2.59856240354522));
#26887=CARTESIAN_POINT('Ctrl Pts',(160.917175397461,0.940429491634335,-3.25488842913799));
#26888=CARTESIAN_POINT('Ctrl Pts',(161.075022413359,3.23895178755388,-0.993930395869087));
#26889=CARTESIAN_POINT('Ctrl Pts',(161.232869429258,2.60427383274531,2.16713269499377));
#26890=CARTESIAN_POINT('Ctrl Pts',(161.390716445156,-0.388838936699488,
3.36563672955522));
#26891=CARTESIAN_POINT('Ctrl Pts',(161.520563338102,-2.56134114788908,1.84427923030537));
#26892=CARTESIAN_POINT('Ctrl Pts',(161.597794559082,-2.86824027379397,0.446333124501563));
#26893=CARTESIAN_POINT('Ctrl Pts',(161.622410108095,-2.86755587111262,0.000487937565173541));
#26894=CARTESIAN_POINT('Ctrl Pts',(160.819589891905,-2.86756195538547,0.000505920555084784));
#26895=CARTESIAN_POINT('Ctrl Pts',(160.847653186543,-2.86675283921063,-0.507783388132381));
#26896=CARTESIAN_POINT('Ctrl Pts',(160.928332153148,-2.49634846830188,-1.97016235883692));
#26897=CARTESIAN_POINT('Ctrl Pts',(161.061626791718,-0.169444440750171,
-3.38378425779796));
#26898=CARTESIAN_POINT('Ctrl Pts',(161.219473807617,2.73951583977761,-1.99342927772498));
#26899=CARTESIAN_POINT('Ctrl Pts',(161.377320823515,3.16756591388022,1.2021786484908));
#26900=CARTESIAN_POINT('Ctrl Pts',(161.535167839414,0.727062906055984,3.30909154487233));
#26901=CARTESIAN_POINT('Ctrl Pts',(161.68259086221,-2.16722040452248,2.47804703603232));
#26902=CARTESIAN_POINT('Ctrl Pts',(161.777398213041,-2.86619328827026,0.758035406874766));
#26903=CARTESIAN_POINT('Ctrl Pts',(161.819589891905,-2.87304766888017,-0.00245486878760231));
#26904=CARTESIAN_POINT('Origin',(155.122410108095,0.,0.));
#26905=CARTESIAN_POINT('',(159.622410108095,-2.87291976826755,-0.00247337730410335));
#26906=CARTESIAN_POINT('',(159.819589891905,-2.87481898359611,0.00195269049801133));
#26907=CARTESIAN_POINT('',(155.122410108095,-2.872,-3.13019997719247E-13));
#26908=CARTESIAN_POINT('Ctrl Pts',(159.622410108095,-2.87291976826755,-0.00247337730410344));
#26909=CARTESIAN_POINT('Ctrl Pts',(159.633073162154,-2.87465654392156,-0.194693232183184));
#26910=CARTESIAN_POINT('Ctrl Pts',(159.69635188818,-2.76982297949715,-1.33351745257318));
#26911=CARTESIAN_POINT('Ctrl Pts',(159.812246286172,-1.25045660967965,-3.14881952692657));
#26912=CARTESIAN_POINT('Ctrl Pts',(159.97009330207,1.9513208570681,-2.76966663578875));
#26913=CARTESIAN_POINT('Ctrl Pts',(160.127940317969,3.38597885066797,0.117701115397386));
#26914=CARTESIAN_POINT('Ctrl Pts',(160.285787333867,1.75428862736512,2.89847851566358));
#26915=CARTESIAN_POINT('Ctrl Pts',(160.443634349766,-1.46608835837003,3.05438884988658));
#26916=CARTESIAN_POINT('Ctrl Pts',(160.555841941175,-2.81152786482851,1.19893040514894));
#26917=CARTESIAN_POINT('Ctrl Pts',(160.615433860618,-2.87577628324411,0.127512032028115));
#26918=CARTESIAN_POINT('Ctrl Pts',(160.622410108095,-2.87478978750438,0.00196536333635124));
#26919=CARTESIAN_POINT('Ctrl Pts',(159.819589891905,-2.87481898359611,0.00195269049801145));
#26920=CARTESIAN_POINT('Ctrl Pts',(159.86529248808,-2.86838656291233,-0.820503393147137));
#26921=CARTESIAN_POINT('Ctrl Pts',(159.963610756221,-2.0686867388201,-2.60075285164511));
#26922=CARTESIAN_POINT('Ctrl Pts',(160.114544696328,0.944304649918255,-3.25376644164669));
#26923=CARTESIAN_POINT('Ctrl Pts',(160.272391712226,3.24013316437363,-0.99007292658079));
#26924=CARTESIAN_POINT('Ctrl Pts',(160.430238728125,2.6016915700248,2.17023231333377));
#26925=CARTESIAN_POINT('Ctrl Pts',(160.588085744023,-0.392846336843677,
3.36517147828997));
#26926=CARTESIAN_POINT('Ctrl Pts',(160.717869465283,-2.56247947481748,1.84196947851954));
#26927=CARTESIAN_POINT('Ctrl Pts',(160.795037514577,-2.86826984538495,0.445204629650228));
#26928=CARTESIAN_POINT('Ctrl Pts',(160.819589891905,-2.86756195538547,0.000505920555084784));
#26929=CARTESIAN_POINT('Origin',(155.122410108095,0.,0.));
#26930=CARTESIAN_POINT('',(158.622410108095,-2.86758577620084,0.000575212723279395));
#26931=CARTESIAN_POINT('',(158.819589891905,-2.87288607329111,-0.00247792941845876));
#26932=CARTESIAN_POINT('',(155.122410108095,-2.872,-3.13019997719247E-13));
#26933=CARTESIAN_POINT('Ctrl Pts',(158.622410108095,-2.86758577620084,0.000575212723279185));
#26934=CARTESIAN_POINT('Ctrl Pts',(158.650712463691,-2.86666019302301,-0.51203374944874));
#26935=CARTESIAN_POINT('Ctrl Pts',(158.731630491253,-2.49163067088092,-1.97887724836087));
#26936=CARTESIAN_POINT('Ctrl Pts',(158.865164190781,-0.154194185277631,
-3.38451172074282));
#26937=CARTESIAN_POINT('Ctrl Pts',(159.02301120668,2.74847035696387,-1.98106498867635));
#26938=CARTESIAN_POINT('Ctrl Pts',(159.180858222578,3.16211653045467,1.21644039120453));
#26939=CARTESIAN_POINT('Ctrl Pts',(159.338705238477,0.71214406652733,3.31233388578888));
#26940=CARTESIAN_POINT('Ctrl Pts',(159.485889200316,-2.17367755200914,2.4696247196516));
#26941=CARTESIAN_POINT('Ctrl Pts',(159.580457490188,-2.86608661474556,0.753794581273767));
#26942=CARTESIAN_POINT('Ctrl Pts',(159.622410108095,-2.87291976826755,-0.00247337730410344));
#26943=CARTESIAN_POINT('Ctrl Pts',(158.819589891905,-2.87288607329111,-0.00247792941845921));
#26944=CARTESIAN_POINT('Ctrl Pts',(158.83031611765,-2.87463411866077,-0.195842464930666));
#26945=CARTESIAN_POINT('Ctrl Pts',(158.893658015361,-2.76906270875085,-1.33582644427906));
#26946=CARTESIAN_POINT('Ctrl Pts',(159.009615585039,-1.24670620219767,-3.15030627040552));
#26947=CARTESIAN_POINT('Ctrl Pts',(159.167462600937,1.95461751556788,-2.76734131891007));
#26948=CARTESIAN_POINT('Ctrl Pts',(159.325309616835,3.38583646824711,0.121732956096346));
#26949=CARTESIAN_POINT('Ctrl Pts',(159.483156632734,1.75083606284643,2.90056550260836));
#26950=CARTESIAN_POINT('Ctrl Pts',(159.641003648632,-1.46972441564107,3.05264107133596));
#26951=CARTESIAN_POINT('Ctrl Pts',(159.753148068356,-2.81219740750062,1.1966272626752));
#26952=CARTESIAN_POINT('Ctrl Pts',(159.812676816114,-2.87579196577723,0.126359216980713));
#26953=CARTESIAN_POINT('Ctrl Pts',(159.819589891905,-2.87481898359611,0.00195269049801145));
#26954=CARTESIAN_POINT('Origin',(155.122410108095,0.,0.));
#26955=CARTESIAN_POINT('',(157.622410108095,-2.87487623080957,0.00203977944324937));
#26956=CARTESIAN_POINT('',(157.819589891905,-2.86758689937222,0.000602879185873928));
#26957=CARTESIAN_POINT('',(155.122410108095,-2.872,-3.13019997719247E-13));
#26958=CARTESIAN_POINT('Ctrl Pts',(157.622410108095,-2.87487623080957,0.00203977944324927));
#26959=CARTESIAN_POINT('Ctrl Pts',(157.668351765227,-2.86851795772887,-0.824605202196607));
#26960=CARTESIAN_POINT('Ctrl Pts',(157.766909094326,-2.06179973823486,-2.60923904502658));
#26961=CARTESIAN_POINT('Ctrl Pts',(157.918082095391,0.958997601442651,-3.24937049328252));
#26962=CARTESIAN_POINT('Ctrl Pts',(158.075929111289,3.24454151146318,-0.97551544854114));
#26963=CARTESIAN_POINT('Ctrl Pts',(158.233776127188,2.5918955157916,2.18196021165553));
#26964=CARTESIAN_POINT('Ctrl Pts',(158.391623143086,-0.408011303340585,
3.36335389202508));
#26965=CARTESIAN_POINT('Ctrl Pts',(158.521167803389,-2.56676870336052,1.83323037708674));
#26966=CARTESIAN_POINT('Ctrl Pts',(158.598096791725,-2.86838090424426,0.44093516188752));
#26967=CARTESIAN_POINT('Ctrl Pts',(158.622410108095,-2.86758577620084,0.000575212723279185));
#26968=CARTESIAN_POINT('Ctrl Pts',(157.819589891905,-2.86758689937222,0.000602879185874344));
#26969=CARTESIAN_POINT('Ctrl Pts',(157.847955419186,-2.86663306014058,-0.513151746479082));
#26970=CARTESIAN_POINT('Ctrl Pts',(157.928936618434,-2.49038917880739,-1.98119549062785));
#26971=CARTESIAN_POINT('Ctrl Pts',(158.062533489648,-0.150157556215628,
-3.38468261701631));
#26972=CARTESIAN_POINT('Ctrl Pts',(158.220380505546,2.7508243349508,-1.97779608453694));
#26973=CARTESIAN_POINT('Ctrl Pts',(158.378227521445,3.1606675065917,1.2202074592191));
#26974=CARTESIAN_POINT('Ctrl Pts',(158.536074537343,0.708198630334437,3.31317840661986));
#26975=CARTESIAN_POINT('Ctrl Pts',(158.683195327497,-2.17537835758644,2.46739841906479));
#26976=CARTESIAN_POINT('Ctrl Pts',(158.777700445684,-2.86605938007723,0.752674302497539));
#26977=CARTESIAN_POINT('Ctrl Pts',(158.819589891905,-2.87288607329111,-0.00247792941845921));
#26978=CARTESIAN_POINT('Origin',(43.7856267685719,0.,-3.14037644537578E-16));
#26979=CARTESIAN_POINT('',(44.,9.5,-1.16341445918999E-15));
#26980=CARTESIAN_POINT('Origin',(44.,0.,0.));
#26981=CARTESIAN_POINT('',(43.5712535371437,10.2572478777138,1.25615057815031E-15));
#26982=CARTESIAN_POINT('',(43.7856267685719,9.87862393885688,1.20978251867015E-15));
#26983=CARTESIAN_POINT('',(43.5712535371437,-10.2572478777138,-1.25615057815031E-15));
#26984=CARTESIAN_POINT('Origin',(43.5712535371437,0.,-6.28075289075157E-16));
#26985=CARTESIAN_POINT('Origin',(43.5712535371437,0.,-6.28075289075157E-16));
#26986=CARTESIAN_POINT('Origin',(43.5,0.,0.));
#26987=CARTESIAN_POINT('',(43.,-10.6,-1.29812560709619E-15));
#26988=CARTESIAN_POINT('',(43.5,-10.3,-1.26138620312177E-15));
#26989=CARTESIAN_POINT('Origin',(43.,0.,0.));
#26990=CARTESIAN_POINT('Origin',(44.,8.8,0.));
#26991=CARTESIAN_POINT('',(44.,-8.8,-1.07768918324967E-15));
#26992=CARTESIAN_POINT('Origin',(44.,0.,0.));
#26993=CARTESIAN_POINT('Origin',(0.,8.73662794227019,5.0440944942793));
#26994=CARTESIAN_POINT('',(0.376949928312602,8.73662794227019,5.0440944942793));
#26995=CARTESIAN_POINT('',(0.6,8.52364026992269,5.41299996417101));
#26996=CARTESIAN_POINT('',(0.770188275695485,8.36112965323919,5.69447660903617));
#26997=CARTESIAN_POINT('',(6.5,8.52364026992269,5.41299996417101));
#26998=CARTESIAN_POINT('',(0.,8.52364026992269,5.41299996417101));
#26999=CARTESIAN_POINT('',(6.5,8.9496156146177,4.67518902438759));
#27000=CARTESIAN_POINT('',(6.5,10.1116279422702,2.66252463387209));
#27001=CARTESIAN_POINT('',(0.6,8.9496156146177,4.67518902438759));
#27002=CARTESIAN_POINT('',(0.,8.9496156146177,4.67518902438759));
#27003=CARTESIAN_POINT('',(1.01481910015687,9.34572108958711,3.98911421658436));
#27004=CARTESIAN_POINT('Origin',(0.,8.96336292916894,5.175));
#27005=CARTESIAN_POINT('',(0.6,6.50538238691624,6.50538238691624));
#27006=CARTESIAN_POINT('',(0.6,6.58029128183,6.46483793479242));
#27007=CARTESIAN_POINT('',(6.5,6.50538238691624,6.50538238691624));
#27008=CARTESIAN_POINT('',(0.,6.50538238691624,6.50538238691624));
#27009=CARTESIAN_POINT('',(6.5,10.8341236570311,4.16245043758503));
#27010=CARTESIAN_POINT('Origin',(0.3,6.43749130332739,6.20100433924467));
#27011=CARTESIAN_POINT('',(0.,8.3534505847788,4.82286694378428));
#27012=CARTESIAN_POINT('',(0.,8.3534505847788,4.82286694378428));
#27013=CARTESIAN_POINT('',(0.,6.06272341459609,6.06272341459609));
#27014=CARTESIAN_POINT('',(0.,6.29469132482479,5.93717074369692));
#27015=CARTESIAN_POINT('',(0.,6.06272341459609,6.06272341459609));
#27016=CARTESIAN_POINT('Origin',(0.3,8.55055027477236,1.07759644317218));
#27017=CARTESIAN_POINT('',(0.6,8.88651760185943,2.38113521494319));
#27018=CARTESIAN_POINT('',(0.6,8.85043686013981,1.06934805444143));
#27019=CARTESIAN_POINT('',(0.,8.28183420045699,2.2191107858609));
#27020=CARTESIAN_POINT('',(0.,8.28183420045699,2.2191107858609));
#27021=CARTESIAN_POINT('',(0.,8.25066368940492,1.08584483190292));
#27022=CARTESIAN_POINT('Origin',(0.,5.0440944942793,8.73662794227019));
#27023=CARTESIAN_POINT('',(0.376949928312603,5.0440944942793,8.73662794227019));
#27024=CARTESIAN_POINT('',(0.6,4.67518902438759,8.9496156146177));
#27025=CARTESIAN_POINT('',(0.770188275695485,4.39371237952243,9.11212623130119));
#27026=CARTESIAN_POINT('',(6.5,4.67518902438759,8.9496156146177));
#27027=CARTESIAN_POINT('',(0.,4.67518902438759,8.9496156146177));
#27028=CARTESIAN_POINT('',(6.5,5.41299996417101,8.52364026992268));
#27029=CARTESIAN_POINT('',(6.5,9.1690944942793,6.35505808186298));
#27030=CARTESIAN_POINT('',(0.6,5.41299996417101,8.52364026992269));
#27031=CARTESIAN_POINT('',(0.,5.41299996417101,8.52364026992268));
#27032=CARTESIAN_POINT('',(1.01481910015687,6.09907477197424,8.12753479495327));
#27033=CARTESIAN_POINT('Origin',(0.,5.175,8.96336292916894));
#27034=CARTESIAN_POINT('',(0.6,2.38113521494319,8.88651760185943));
#27035=CARTESIAN_POINT('',(0.6,2.46628044696984,8.88885952379457));
#27036=CARTESIAN_POINT('',(6.5,2.38113521494319,8.88651760185943));
#27037=CARTESIAN_POINT('',(0.,2.38113521494319,8.88651760185943));
#27038=CARTESIAN_POINT('',(6.5,7.96212269650768,9.04002281514855));
#27039=CARTESIAN_POINT('Origin',(0.3,2.47452883570058,8.58897293842712));
#27040=CARTESIAN_POINT('',(0.,4.82286694378428,8.3534505847788));
#27041=CARTESIAN_POINT('',(0.,4.82286694378428,8.3534505847788));
#27042=CARTESIAN_POINT('',(0.,2.2191107858609,8.28183420045699));
#27043=CARTESIAN_POINT('',(0.,2.48277722443133,8.28908635305967));
#27044=CARTESIAN_POINT('',(0.,2.2191107858609,8.28183420045699));
#27045=CARTESIAN_POINT('Origin',(0.3,6.86619553270279,5.20850103220104));
#27046=CARTESIAN_POINT('',(0.6,7.13002912825054,5.35130101070365));
#27047=CARTESIAN_POINT('',(0.,6.60236193715504,5.06570105369843));
#27048=CARTESIAN_POINT('Origin',(0.,2.98372437868011E-15,10.0881889885586));
#27049=CARTESIAN_POINT('',(0.376949928312603,5.01337711727344E-16,10.0881889885586));
#27050=CARTESIAN_POINT('',(0.6,-0.425975344695007,10.0881889885586));
#27051=CARTESIAN_POINT('',(0.770188275695485,-0.750996578061993,10.0881889885586));
#27052=CARTESIAN_POINT('',(6.5,-0.425975344695008,10.0881889885586));
#27053=CARTESIAN_POINT('',(0.,-0.425975344695007,10.0881889885586));
#27054=CARTESIAN_POINT('',(6.5,0.425975344695013,10.0881889885586));
#27055=CARTESIAN_POINT('',(6.5,5.50000000000002,10.0881889885586));
#27056=CARTESIAN_POINT('',(0.6,0.425975344695013,10.0881889885586));
#27057=CARTESIAN_POINT('',(0.,0.425975344695013,10.0881889885586));
#27058=CARTESIAN_POINT('',(1.01481910015687,1.21818629463384,10.0881889885586));
#27059=CARTESIAN_POINT('Origin',(0.,6.33754718558755E-16,10.35));
#27060=CARTESIAN_POINT('',(0.6,-2.38113521494319,8.88651760185943));
#27061=CARTESIAN_POINT('',(0.6,-2.30856824196456,8.93111838176226));
#27062=CARTESIAN_POINT('',(6.5,-2.38113521494319,8.88651760185943));
#27063=CARTESIAN_POINT('',(0.,-2.38113521494319,8.88651760185943));
#27064=CARTESIAN_POINT('',(6.5,1.68344163237214,11.3846691703236));
#27065=CARTESIAN_POINT('Origin',(0.3,-2.15148163509972,8.67553317494525));
#27066=CARTESIAN_POINT('',(0.,5.55111512312578E-16,9.64573388756855));
#27067=CARTESIAN_POINT('',(0.,2.77555756156289E-16,9.64573388756855));
#27068=CARTESIAN_POINT('',(0.,-2.21911078586091,8.28183420045699));
#27069=CARTESIAN_POINT('',(0.,-1.99439502823489,8.41994796812825));
#27070=CARTESIAN_POINT('',(0.,-2.21911078586091,8.28183420045699));
#27071=CARTESIAN_POINT('Origin',(0.3,3.34204924257132,7.94379197587497));
#27072=CARTESIAN_POINT('',(0.6,3.49913584943616,8.19937718269197));
#27073=CARTESIAN_POINT('',(0.,3.18496263570648,7.68820676905796));
#27074=CARTESIAN_POINT('Origin',(0.,-5.0440944942793,8.73662794227019));
#27075=CARTESIAN_POINT('',(0.376949928312603,-5.0440944942793,8.73662794227019));
#27076=CARTESIAN_POINT('',(0.6,-5.41299996417101,8.52364026992269));
#27077=CARTESIAN_POINT('',(0.770188275695485,-5.69447660903617,8.36112965323919));
#27078=CARTESIAN_POINT('',(6.5,-5.41299996417101,8.52364026992269));
#27079=CARTESIAN_POINT('',(0.,-5.41299996417101,8.52364026992269));
#27080=CARTESIAN_POINT('',(6.5,-4.67518902438759,8.9496156146177));
#27081=CARTESIAN_POINT('',(6.5,-0.919094494279296,11.1181978026774));
#27082=CARTESIAN_POINT('',(0.6,-4.67518902438759,8.9496156146177));
#27083=CARTESIAN_POINT('',(0.,-4.67518902438759,8.9496156146177));
#27084=CARTESIAN_POINT('',(1.01481910015687,-3.98911421658436,9.34572108958711));
#27085=CARTESIAN_POINT('Origin',(0.,-5.175,8.96336292916894));
#27086=CARTESIAN_POINT('',(0.6,-6.50538238691624,6.50538238691624));
#27087=CARTESIAN_POINT('',(0.6,-6.46483793479242,6.58029128183));
#27088=CARTESIAN_POINT('',(6.5,-6.50538238691624,6.50538238691624));
#27089=CARTESIAN_POINT('',(0.,-6.50538238691624,6.50538238691624));
#27090=CARTESIAN_POINT('',(6.5,-5.21867030999356,8.88267877903739));
#27091=CARTESIAN_POINT('Origin',(0.3,-6.20100433924467,6.4374913033274));
#27092=CARTESIAN_POINT('',(0.,-4.82286694378427,8.3534505847788));
#27093=CARTESIAN_POINT('',(0.,-4.82286694378427,8.3534505847788));
#27094=CARTESIAN_POINT('',(0.,-6.06272341459609,6.06272341459609));
#27095=CARTESIAN_POINT('',(0.,-5.93717074369692,6.29469132482479));
#27096=CARTESIAN_POINT('',(0.,-6.06272341459609,6.06272341459609));
#27097=CARTESIAN_POINT('Origin',(0.3,-1.07759644317218,8.55055027477236));
#27098=CARTESIAN_POINT('',(0.6,-1.06934805444143,8.85043686013981));
#27099=CARTESIAN_POINT('',(0.,-1.08584483190292,8.25066368940492));
#27100=CARTESIAN_POINT('Origin',(0.,-8.73662794227019,5.0440944942793));
#27101=CARTESIAN_POINT('',(0.376949928312603,-8.73662794227019,5.0440944942793));
#27102=CARTESIAN_POINT('',(0.6,-8.9496156146177,4.67518902438759));
#27103=CARTESIAN_POINT('',(0.770188275695485,-9.11212623130119,4.39371237952243));
#27104=CARTESIAN_POINT('',(6.5,-8.9496156146177,4.67518902438759));
#27105=CARTESIAN_POINT('',(0.,-8.9496156146177,4.67518902438759));
#27106=CARTESIAN_POINT('',(6.5,-8.52364026992269,5.41299996417101));
#27107=CARTESIAN_POINT('',(6.5,-7.36162794227019,7.42566435468651));
#27108=CARTESIAN_POINT('',(0.6,-8.52364026992269,5.41299996417101));
#27109=CARTESIAN_POINT('',(0.,-8.52364026992269,5.41299996417101));
#27110=CARTESIAN_POINT('',(1.01481910015687,-8.12753479495327,6.09907477197424));
#27111=CARTESIAN_POINT('Origin',(0.,-8.96336292916894,5.175));
#27112=CARTESIAN_POINT('',(0.6,-8.88651760185943,2.38113521494319));
#27113=CARTESIAN_POINT('',(0.6,-8.88885952379457,2.46628044696983));
#27114=CARTESIAN_POINT('',(6.5,-8.88651760185943,2.38113521494319));
#27115=CARTESIAN_POINT('',(0.,-8.88651760185943,2.38113521494319));
#27116=CARTESIAN_POINT('',(6.5,-8.88470177333241,2.31511715561584));
#27117=CARTESIAN_POINT('Origin',(0.3,-8.58897293842712,2.47452883570058));
#27118=CARTESIAN_POINT('',(0.,-8.3534505847788,4.82286694378428));
#27119=CARTESIAN_POINT('',(0.,-8.3534505847788,4.82286694378428));
#27120=CARTESIAN_POINT('',(0.,-8.281834200457,2.21911078586091));
#27121=CARTESIAN_POINT('',(0.,-8.28908635305967,2.48277722443133));
#27122=CARTESIAN_POINT('',(0.,-8.281834200457,2.21911078586091));
#27123=CARTESIAN_POINT('Origin',(0.3,-5.20850103220104,6.86619553270279));
#27124=CARTESIAN_POINT('',(0.6,-5.35130101070365,7.13002912825054));
#27125=CARTESIAN_POINT('',(0.,-5.06570105369844,6.60236193715504));
#27126=CARTESIAN_POINT('Origin',(0.,10.0881889885586,-3.46944695195361E-16));
#27127=CARTESIAN_POINT('',(0.376949928312603,10.0881889885586,-4.12725542052732E-16));
#27128=CARTESIAN_POINT('',(0.6,10.0881889885586,0.425975344695008));
#27129=CARTESIAN_POINT('',(0.770188275695485,10.0881889885586,0.750996578061995));
#27130=CARTESIAN_POINT('',(6.5,10.0881889885586,0.425975344695008));
#27131=CARTESIAN_POINT('',(0.,10.0881889885586,0.425975344695009));
#27132=CARTESIAN_POINT('',(6.5,10.0881889885586,-0.42597534469501));
#27133=CARTESIAN_POINT('',(6.5,10.0881889885586,1.01475790048603E-15));
#27134=CARTESIAN_POINT('',(0.6,10.0881889885586,-0.42597534469501));
#27135=CARTESIAN_POINT('',(0.,10.0881889885586,-0.42597534469501));
#27136=CARTESIAN_POINT('',(1.01481910015687,10.0881889885586,-1.21818629463384));
#27137=CARTESIAN_POINT('Origin',(0.,10.35,0.));
#27138=CARTESIAN_POINT('',(0.6,8.93111838176226,2.30856824196456));
#27139=CARTESIAN_POINT('',(6.5,8.88651760185943,2.38113521494319));
#27140=CARTESIAN_POINT('',(0.,8.88651760185943,2.38113521494319));
#27141=CARTESIAN_POINT('',(6.5,10.4391085074256,-0.144982546596809));
#27142=CARTESIAN_POINT('Origin',(0.3,8.67553317494525,2.15148163509972));
#27143=CARTESIAN_POINT('',(0.,9.64573388756855,-1.11022302462516E-15));
#27144=CARTESIAN_POINT('',(0.,9.64573388756855,-1.11022302462516E-15));
#27145=CARTESIAN_POINT('',(0.,8.41994796812825,1.99439502823489));
#27146=CARTESIAN_POINT('Origin',(0.3,7.94379197587497,-3.34204924257132));
#27147=CARTESIAN_POINT('',(0.6,8.88651760185943,-2.38113521494319));
#27148=CARTESIAN_POINT('',(0.6,8.19937718269197,-3.49913584943616));
#27149=CARTESIAN_POINT('',(0.,8.28183420045699,-2.2191107858609));
#27150=CARTESIAN_POINT('',(0.6,8.88651760185943,-2.38113521494319));
#27151=CARTESIAN_POINT('',(0.,7.68820676905796,-3.18496263570648));
#27152=CARTESIAN_POINT('Origin',(0.,8.73662794227019,-5.0440944942793));
#27153=CARTESIAN_POINT('',(0.376949928312602,8.73662794227019,-5.0440944942793));
#27154=CARTESIAN_POINT('',(0.6,8.94961561461769,-4.67518902438759));
#27155=CARTESIAN_POINT('',(0.770188275695484,9.11212623130119,-4.39371237952243));
#27156=CARTESIAN_POINT('',(6.5,8.94961561461769,-4.67518902438759));
#27157=CARTESIAN_POINT('',(0.,8.94961561461769,-4.67518902438759));
#27158=CARTESIAN_POINT('',(6.5,8.52364026992268,-5.41299996417101));
#27159=CARTESIAN_POINT('',(6.5,10.1116279422702,-2.6625246338721));
#27160=CARTESIAN_POINT('',(0.6,8.52364026992268,-5.41299996417102));
#27161=CARTESIAN_POINT('',(0.,8.52364026992268,-5.41299996417101));
#27162=CARTESIAN_POINT('',(1.01481910015687,8.12753479495326,-6.09907477197424));
#27163=CARTESIAN_POINT('Origin',(0.,8.96336292916894,-5.175));
#27164=CARTESIAN_POINT('',(0.6,8.88885952379457,-2.46628044696984));
#27165=CARTESIAN_POINT('',(6.5,8.88651760185943,-2.38113521494319));
#27166=CARTESIAN_POINT('',(0.,8.88651760185943,-2.38113521494319));
#27167=CARTESIAN_POINT('',(6.5,8.89301727425672,-2.61744373832382));
#27168=CARTESIAN_POINT('Origin',(0.3,8.58897293842712,-2.47452883570059));
#27169=CARTESIAN_POINT('',(0.,8.3534505847788,-4.82286694378428));
#27170=CARTESIAN_POINT('',(0.,8.3534505847788,-4.82286694378428));
#27171=CARTESIAN_POINT('',(0.,8.28908635305967,-2.48277722443133));
#27172=CARTESIAN_POINT('Origin',(0.,5.0440944942793,-8.73662794227019));
#27173=CARTESIAN_POINT('',(0.376949928312603,5.0440944942793,-8.73662794227019));
#27174=CARTESIAN_POINT('',(0.6,5.41299996417101,-8.52364026992269));
#27175=CARTESIAN_POINT('',(0.770188275695485,5.69447660903618,-8.36112965323919));
#27176=CARTESIAN_POINT('',(6.5,5.41299996417101,-8.52364026992269));
#27177=CARTESIAN_POINT('',(0.,5.41299996417101,-8.52364026992269));
#27178=CARTESIAN_POINT('',(6.5,4.67518902438759,-8.9496156146177));
#27179=CARTESIAN_POINT('',(6.5,9.1690944942793,-6.35505808186299));
#27180=CARTESIAN_POINT('',(0.6,4.67518902438759,-8.9496156146177));
#27181=CARTESIAN_POINT('',(0.,4.67518902438759,-8.9496156146177));
#27182=CARTESIAN_POINT('',(1.01481910015687,3.98911421658436,-9.34572108958711));
#27183=CARTESIAN_POINT('Origin',(0.,5.175,-8.96336292916894));
#27184=CARTESIAN_POINT('',(0.6,6.50538238691624,-6.50538238691624));
#27185=CARTESIAN_POINT('',(0.6,6.46483793479242,-6.58029128183));
#27186=CARTESIAN_POINT('',(6.5,6.50538238691624,-6.50538238691624));
#27187=CARTESIAN_POINT('',(0.,6.50538238691624,-6.50538238691624));
#27188=CARTESIAN_POINT('',(6.5,7.71100555959128,-4.27790378462261));
#27189=CARTESIAN_POINT('Origin',(0.3,6.20100433924467,-6.43749130332739));
#27190=CARTESIAN_POINT('',(0.,4.82286694378428,-8.3534505847788));
#27191=CARTESIAN_POINT('',(0.,4.82286694378428,-8.3534505847788));
#27192=CARTESIAN_POINT('',(0.,6.06272341459609,-6.06272341459609));
#27193=CARTESIAN_POINT('',(0.,5.93717074369692,-6.29469132482479));
#27194=CARTESIAN_POINT('',(0.,6.06272341459609,-6.06272341459609));
#27195=CARTESIAN_POINT('Origin',(0.3,1.07759644317218,-8.55055027477237));
#27196=CARTESIAN_POINT('',(0.6,2.38113521494319,-8.88651760185943));
#27197=CARTESIAN_POINT('',(0.6,1.06934805444143,-8.85043686013981));
#27198=CARTESIAN_POINT('',(0.,2.2191107858609,-8.281834200457));
#27199=CARTESIAN_POINT('',(0.,2.2191107858609,-8.281834200457));
#27200=CARTESIAN_POINT('',(0.,1.08584483190293,-8.25066368940492));
#27201=CARTESIAN_POINT('Origin',(0.,-3.53883589099269E-15,-10.0881889885586));
#27202=CARTESIAN_POINT('',(0.376949928312603,-1.0912875931293E-15,-10.0881889885586));
#27203=CARTESIAN_POINT('',(0.6,0.425975344695006,-10.0881889885586));
#27204=CARTESIAN_POINT('',(0.770188275695485,0.750996578061993,-10.0881889885586));
#27205=CARTESIAN_POINT('',(6.5,0.425975344695005,-10.0881889885586));
#27206=CARTESIAN_POINT('',(0.,0.425975344695005,-10.0881889885586));
#27207=CARTESIAN_POINT('',(6.5,-0.425975344695013,-10.0881889885586));
#27208=CARTESIAN_POINT('',(6.5,5.49999999999998,-10.0881889885586));
#27209=CARTESIAN_POINT('',(0.6,-0.425975344695012,-10.0881889885586));
#27210=CARTESIAN_POINT('',(0.,-0.425975344695013,-10.0881889885586));
#27211=CARTESIAN_POINT('',(1.01481910015687,-1.21818629463384,-10.0881889885586));
#27212=CARTESIAN_POINT('Origin',(0.,-1.90126415567627E-15,-10.35));
#27213=CARTESIAN_POINT('',(0.6,2.30856824196456,-8.93111838176226));
#27214=CARTESIAN_POINT('',(6.5,2.38113521494319,-8.88651760185943));
#27215=CARTESIAN_POINT('',(0.,2.38113521494319,-8.88651760185943));
#27216=CARTESIAN_POINT('',(6.5,6.30057811630126,-6.47756759320089));
#27217=CARTESIAN_POINT('Origin',(0.3,2.15148163509972,-8.67553317494525));
#27218=CARTESIAN_POINT('',(0.,0.,-9.64573388756855));
#27219=CARTESIAN_POINT('',(0.,2.77555756156289E-16,-9.64573388756855));
#27220=CARTESIAN_POINT('',(0.,1.99439502823488,-8.41994796812825));
#27221=CARTESIAN_POINT('Origin',(0.3,-3.34204924257132,-7.94379197587497));
#27222=CARTESIAN_POINT('',(0.6,-2.38113521494319,-8.88651760185943));
#27223=CARTESIAN_POINT('',(0.6,-3.49913584943616,-8.19937718269197));
#27224=CARTESIAN_POINT('',(0.,-2.2191107858609,-8.28183420045699));
#27225=CARTESIAN_POINT('',(0.,-2.2191107858609,-8.28183420045699));
#27226=CARTESIAN_POINT('',(0.,-3.18496263570648,-7.68820676905796));
#27227=CARTESIAN_POINT('Origin',(0.,-5.0440944942793,-8.73662794227019));
#27228=CARTESIAN_POINT('',(0.376949928312602,-5.0440944942793,-8.73662794227019));
#27229=CARTESIAN_POINT('',(0.6,-4.67518902438759,-8.94961561461769));
#27230=CARTESIAN_POINT('',(0.770188275695484,-4.39371237952243,-9.11212623130119));
#27231=CARTESIAN_POINT('',(6.5,-4.67518902438759,-8.94961561461769));
#27232=CARTESIAN_POINT('',(0.,-4.67518902438759,-8.94961561461769));
#27233=CARTESIAN_POINT('',(6.5,-5.41299996417102,-8.52364026992268));
#27234=CARTESIAN_POINT('',(6.5,-0.919094494279309,-11.1181978026774));
#27235=CARTESIAN_POINT('',(0.6,-5.41299996417101,-8.52364026992268));
#27236=CARTESIAN_POINT('',(0.,-5.41299996417101,-8.52364026992268));
#27237=CARTESIAN_POINT('',(1.01481910015687,-6.09907477197424,-8.12753479495327));
#27238=CARTESIAN_POINT('Origin',(0.,-5.175,-8.96336292916894));
#27239=CARTESIAN_POINT('',(0.6,-2.46628044696984,-8.88885952379457));
#27240=CARTESIAN_POINT('',(6.5,-2.38113521494319,-8.88651760185943));
#27241=CARTESIAN_POINT('',(0.,-2.38113521494319,-8.88651760185943));
#27242=CARTESIAN_POINT('',(6.5,3.029561802568,-8.73769623244058));
#27243=CARTESIAN_POINT('Origin',(0.3,-2.47452883570059,-8.58897293842712));
#27244=CARTESIAN_POINT('',(0.,-4.82286694378428,-8.3534505847788));
#27245=CARTESIAN_POINT('',(0.,-4.82286694378428,-8.3534505847788));
#27246=CARTESIAN_POINT('',(0.,-2.48277722443133,-8.28908635305967));
#27247=CARTESIAN_POINT('Origin',(0.3,-6.86619553270279,-5.20850103220104));
#27248=CARTESIAN_POINT('',(0.6,-6.50538238691624,-6.50538238691624));
#27249=CARTESIAN_POINT('',(0.6,-7.13002912825054,-5.35130101070365));
#27250=CARTESIAN_POINT('',(0.,-6.06272341459609,-6.06272341459609));
#27251=CARTESIAN_POINT('',(0.,-6.06272341459609,-6.06272341459609));
#27252=CARTESIAN_POINT('',(0.,-6.60236193715504,-5.06570105369843));
#27253=CARTESIAN_POINT('Origin',(0.,-8.73662794227019,-5.0440944942793));
#27254=CARTESIAN_POINT('',(0.376949928312602,-8.73662794227019,-5.0440944942793));
#27255=CARTESIAN_POINT('',(0.6,-8.52364026992268,-5.41299996417101));
#27256=CARTESIAN_POINT('',(0.770188275695484,-8.36112965323919,-5.69447660903617));
#27257=CARTESIAN_POINT('',(6.5,-8.52364026992268,-5.41299996417101));
#27258=CARTESIAN_POINT('',(0.,-8.52364026992268,-5.41299996417101));
#27259=CARTESIAN_POINT('',(6.5,-8.9496156146177,-4.67518902438759));
#27260=CARTESIAN_POINT('',(6.5,-7.36162794227019,-7.42566435468651));
#27261=CARTESIAN_POINT('',(0.6,-8.9496156146177,-4.67518902438759));
#27262=CARTESIAN_POINT('',(0.,-8.9496156146177,-4.67518902438759));
#27263=CARTESIAN_POINT('',(1.01481910015687,-9.34572108958711,-3.98911421658436));
#27264=CARTESIAN_POINT('Origin',(0.,-8.96336292916894,-5.175));
#27265=CARTESIAN_POINT('',(0.6,-6.58029128183,-6.46483793479242));
#27266=CARTESIAN_POINT('',(6.5,-6.50538238691624,-6.50538238691624));
#27267=CARTESIAN_POINT('',(0.,-6.50538238691624,-6.50538238691624));
#27268=CARTESIAN_POINT('',(6.5,-2.32645890662886,-8.76722543199981));
#27269=CARTESIAN_POINT('Origin',(0.3,-6.43749130332739,-6.20100433924467));
#27270=CARTESIAN_POINT('',(0.,-8.3534505847788,-4.82286694378428));
#27271=CARTESIAN_POINT('',(0.,-8.3534505847788,-4.82286694378428));
#27272=CARTESIAN_POINT('',(0.,-6.29469132482479,-5.93717074369692));
#27273=CARTESIAN_POINT('Origin',(0.3,-8.55055027477236,-1.07759644317218));
#27274=CARTESIAN_POINT('',(0.6,-8.88651760185943,-2.38113521494319));
#27275=CARTESIAN_POINT('',(0.6,-8.85043686013981,-1.06934805444143));
#27276=CARTESIAN_POINT('',(0.,-8.281834200457,-2.2191107858609));
#27277=CARTESIAN_POINT('',(0.,-8.281834200457,-2.2191107858609));
#27278=CARTESIAN_POINT('',(0.,-8.25066368940492,-1.08584483190293));
#27279=CARTESIAN_POINT('Origin',(0.,-10.0881889885586,1.04083408558608E-15));
#27280=CARTESIAN_POINT('',(0.376949928312603,-10.0881889885586,1.41540096550742E-15));
#27281=CARTESIAN_POINT('',(0.6,-10.0881889885586,-0.425975344695007));
#27282=CARTESIAN_POINT('',(0.770188275695486,-10.0881889885586,-0.750996578061997));
#27283=CARTESIAN_POINT('',(6.5,-10.0881889885586,-0.425975344695008));
#27284=CARTESIAN_POINT('',(0.,-10.0881889885586,-0.425975344695008));
#27285=CARTESIAN_POINT('',(6.5,-10.0881889885586,0.42597534469501));
#27286=CARTESIAN_POINT('',(6.5,-10.0881889885586,5.20417042793042E-16));
#27287=CARTESIAN_POINT('',(0.6,-10.0881889885586,0.425975344695009));
#27288=CARTESIAN_POINT('',(0.,-10.0881889885586,0.42597534469501));
#27289=CARTESIAN_POINT('',(1.01481910015687,-10.0881889885586,1.21818629463384));
#27290=CARTESIAN_POINT('Origin',(0.,-10.35,1.26750943711751E-15));
#27291=CARTESIAN_POINT('',(0.6,-8.93111838176226,-2.30856824196456));
#27292=CARTESIAN_POINT('',(6.5,-8.88651760185943,-2.38113521494319));
#27293=CARTESIAN_POINT('',(0.,-8.88651760185943,-2.38113521494319));
#27294=CARTESIAN_POINT('',(6.5,-7.42312825609896,-4.76211903052593));
#27295=CARTESIAN_POINT('Origin',(0.3,-8.67553317494525,-2.15148163509972));
#27296=CARTESIAN_POINT('',(0.,-9.64573388756855,2.22044604925031E-15));
#27297=CARTESIAN_POINT('',(0.,-9.64573388756855,1.66533453693773E-15));
#27298=CARTESIAN_POINT('',(0.,-8.41994796812825,-1.99439502823488));
#27299=CARTESIAN_POINT('Origin',(0.3,-7.94379197587497,3.34204924257132));
#27300=CARTESIAN_POINT('',(0.6,-8.19937718269197,3.49913584943616));
#27301=CARTESIAN_POINT('',(0.,-7.68820676905796,3.18496263570648));
#27302=CARTESIAN_POINT('Origin',(40.65,0.,0.));
#27303=CARTESIAN_POINT('',(40.4,34.9678423698117,1.5));
#27304=CARTESIAN_POINT('',(40.9,34.4673758792282,1.5));
#27305=CARTESIAN_POINT('Ctrl Pts',(40.4,34.9678423698117,1.5));
#27306=CARTESIAN_POINT('Ctrl Pts',(40.5666590135434,34.801030090909,1.5));
#27307=CARTESIAN_POINT('Ctrl Pts',(40.7333430449885,34.6341905786716,1.5));
#27308=CARTESIAN_POINT('Ctrl Pts',(40.9,34.4673758792282,1.5));
#27309=CARTESIAN_POINT('',(40.9,34.4673758792282,-1.50000000000001));
#27310=CARTESIAN_POINT('Origin',(40.9,0.,0.));
#27311=CARTESIAN_POINT('',(40.4,34.9678423698117,-1.5));
#27312=CARTESIAN_POINT('Ctrl Pts',(40.9,34.4673758792282,-1.5));
#27313=CARTESIAN_POINT('Ctrl Pts',(40.7333430449627,34.6341905786974,-1.5));
#27314=CARTESIAN_POINT('Ctrl Pts',(40.5666590137774,34.8010300906748,-1.5));
#27315=CARTESIAN_POINT('Ctrl Pts',(40.4,34.9678423698117,-1.5));
#27316=CARTESIAN_POINT('Origin',(40.4,0.,0.));
#27317=CARTESIAN_POINT('Origin',(35.7,0.,0.));
#27318=CARTESIAN_POINT('',(30.5,34.9656486014478,-1.55029606206997));
#27319=CARTESIAN_POINT('Ctrl Pts',(40.3999921398529,34.9678423429768,-1.49999538724755));
#27320=CARTESIAN_POINT('Ctrl Pts',(39.2499570215113,34.9678422244593,-1.49997501500716));
#27321=CARTESIAN_POINT('Ctrl Pts',(38.0998114916604,34.9678417480135,-1.49989311899335));
#27322=CARTESIAN_POINT('Ctrl Pts',(36.9497038557168,34.9678416168427,-1.49987059349837));
#27323=CARTESIAN_POINT('Ctrl Pts',(36.785105117964,34.96784159807,-1.49986736974093));
#27324=CARTESIAN_POINT('Ctrl Pts',(36.6205071563607,34.9678415863694,-1.49986536202073));
#27325=CARTESIAN_POINT('Ctrl Pts',(36.4559233022361,34.9678415707796,-1.49986268095531));
#27326=CARTESIAN_POINT('Ctrl Pts',(36.4193640724435,34.9678415673166,-1.4998620854067));
#27327=CARTESIAN_POINT('Ctrl Pts',(36.3828055387466,34.9678415636617,-1.49986145663366));
#27328=CARTESIAN_POINT('Ctrl Pts',(36.3462474593958,34.967841559861,-1.49986080263032));
#27329=CARTESIAN_POINT('Ctrl Pts',(36.0895450699579,34.967841533173,-1.49985621036995));
#27330=CARTESIAN_POINT('Ctrl Pts',(35.8501671305851,34.9678416196704,-1.49985084735668));
#27331=CARTESIAN_POINT('Ctrl Pts',(35.6266230092018,34.9678417642539,-1.49984692867086));
#27332=CARTESIAN_POINT('Ctrl Pts',(35.5729810992077,34.9678417989483,-1.49984598833841));
#27333=CARTESIAN_POINT('Ctrl Pts',(35.5202511626857,34.9678418369404,-1.49984512300934));
#27334=CARTESIAN_POINT('Ctrl Pts',(35.4684130151836,34.9678418773881,-1.4998443492858));
#27335=CARTESIAN_POINT('Ctrl Pts',(35.3128073279263,34.9678419988026,-1.49984202675329));
#27336=CARTESIAN_POINT('Ctrl Pts',(35.1652418679138,34.9678421408902,-1.49984027810624));
#27337=CARTESIAN_POINT('Ctrl Pts',(35.0252627275547,34.967842254217,-1.49983493809963));
#27338=CARTESIAN_POINT('Ctrl Pts',(35.0082618963838,34.9678422679808,-1.49983428954192));
#27339=CARTESIAN_POINT('Ctrl Pts',(34.9913729068342,34.9678422813397,-1.49983359135557));
#27340=CARTESIAN_POINT('Ctrl Pts',(34.9745948969331,34.9678422942204,-1.49983283870325));
#27341=CARTESIAN_POINT('Ctrl Pts',(34.8399133402553,34.9678423976168,-1.49982679696251));
#27342=CARTESIAN_POINT('Ctrl Pts',(34.7123780512931,34.9678424712592,-1.49981743040037));
#27343=CARTESIAN_POINT('Ctrl Pts',(34.591404591981,34.9678425127826,-1.49980840280397));
#27344=CARTESIAN_POINT('Ctrl Pts',(34.4539348326465,34.9678425599684,-1.49979814417771));
#27345=CARTESIAN_POINT('Ctrl Pts',(34.3249390274092,34.9678425655798,-1.49978830616204));
#27346=CARTESIAN_POINT('Ctrl Pts',(34.2036312646158,34.9678425105859,-1.49978156609768));
#27347=CARTESIAN_POINT('Ctrl Pts',(34.1284740534062,34.967842476514,-1.49977739023598));
#27348=CARTESIAN_POINT('Ctrl Pts',(34.0562692606603,34.9678424188851,-1.49977435262848));
#27349=CARTESIAN_POINT('Ctrl Pts',(33.9868395791739,34.9678423310509,-1.49977272195139));
#27350=CARTESIAN_POINT('Ctrl Pts',(33.944569913827,34.9678422775764,-1.49977172917461));
#27351=CARTESIAN_POINT('Ctrl Pts',(33.903332682828,34.9678422127028,-1.49977122168105));
#27352=CARTESIAN_POINT('Ctrl Pts',(33.8632274501546,34.9678421281365,-1.49977004757329));
#27353=CARTESIAN_POINT('Ctrl Pts',(33.8167531035319,34.9678420301403,-1.49976868700542));
#27354=CARTESIAN_POINT('Ctrl Pts',(33.771789463122,34.9678419060139,-1.49976648823776));
#27355=CARTESIAN_POINT('Ctrl Pts',(33.7281109635882,34.9678417565821,-1.49976414064438));
#27356=CARTESIAN_POINT('Ctrl Pts',(33.6812712011832,34.9678415963351,-1.49976162314223));
#27357=CARTESIAN_POINT('Ctrl Pts',(33.6359095723891,34.9678414069824,-1.49975893360226));
#27358=CARTESIAN_POINT('Ctrl Pts',(33.591810246565,34.9678411881909,-1.49975667024846));
#27359=CARTESIAN_POINT('Ctrl Pts',(33.5583448079856,34.9678410221577,-1.4997549526683));
#27360=CARTESIAN_POINT('Ctrl Pts',(33.5256076932742,34.9678408391413,-1.49975347489115));
#27361=CARTESIAN_POINT('Ctrl Pts',(33.4935243452377,34.9678406385663,-1.49975241817239));
#27362=CARTESIAN_POINT('Ctrl Pts',(33.4574180647961,34.9678404128412,-1.49975122895162));
#27363=CARTESIAN_POINT('Ctrl Pts',(33.4221459355308,34.9678401647559,-1.49975055002973));
#27364=CARTESIAN_POINT('Ctrl Pts',(33.3878318916215,34.9678398888653,-1.49974977143672));
#27365=CARTESIAN_POINT('Ctrl Pts',(33.3506903036195,34.9678395902407,-1.49974892868612));
#27366=CARTESIAN_POINT('Ctrl Pts',(33.3146710708563,34.9678392590421,-1.49974796966079));
#27367=CARTESIAN_POINT('Ctrl Pts',(33.2798677329257,34.967838889585,-1.49974635090117));
#27368=CARTESIAN_POINT('Ctrl Pts',(33.2432742079925,34.9678385011241,-1.49974464887706));
#27369=CARTESIAN_POINT('Ctrl Pts',(33.2080243245406,34.9678380703783,-1.49974221953694));
#27370=CARTESIAN_POINT('Ctrl Pts',(33.1741651388244,34.9678375919209,-1.4997386537707));
#27371=CARTESIAN_POINT('Ctrl Pts',(33.137063146823,34.96783706764,-1.49973474649923));
#27372=CARTESIAN_POINT('Ctrl Pts',(33.1016306515623,34.9678364860775,-1.49972947597288));
#27373=CARTESIAN_POINT('Ctrl Pts',(33.067864102108,34.9678358413429,-1.49972253958674));
#27374=CARTESIAN_POINT('Ctrl Pts',(33.0456526984032,34.967835417241,-1.49971797687971));
#27375=CARTESIAN_POINT('Ctrl Pts',(33.0241607955796,34.9678349658306,-1.49971269819094));
#27376=CARTESIAN_POINT('Ctrl Pts',(33.0033754048768,34.9678344856631,-1.49970666036488));
#27377=CARTESIAN_POINT('Ctrl Pts',(32.9442530209621,34.9678331198648,-1.49968948625086));
#27378=CARTESIAN_POINT('Ctrl Pts',(32.8887085075052,34.9678225692834,-1.49991335207053));
#27379=CARTESIAN_POINT('Ctrl Pts',(32.8362583193005,34.9678066670084,-1.50027559162313));
#27380=CARTESIAN_POINT('Ctrl Pts',(32.7773090712614,34.9677887942955,-1.50068271598181));
#27381=CARTESIAN_POINT('Ctrl Pts',(32.7222687069615,34.9677641462319,-1.50126502290934));
#27382=CARTESIAN_POINT('Ctrl Pts',(32.6704155259712,34.9677359487883,-1.50193537623735));
#27383=CARTESIAN_POINT('Ctrl Pts',(32.6144302418907,34.9677055043322,-1.50265914902788));
#27384=CARTESIAN_POINT('Ctrl Pts',(32.562160274654,34.967670888482,-1.50348644308881));
#27385=CARTESIAN_POINT('Ctrl Pts',(32.5126575741465,34.9676341575402,-1.50436077830378));
#27386=CARTESIAN_POINT('Ctrl Pts',(32.4592478825335,34.967594527616,-1.50530412025724));
#27387=CARTESIAN_POINT('Ctrl Pts',(32.4090594121702,34.9675524017484,-1.50630310623455));
#27388=CARTESIAN_POINT('Ctrl Pts',(32.3608584151774,34.9675086790575,-1.50733170420881));
#27389=CARTESIAN_POINT('Ctrl Pts',(32.3080624384018,34.9674607883018,-1.50845835797425));
#27390=CARTESIAN_POINT('Ctrl Pts',(32.2576510584103,34.9674109512874,-1.50962133088216));
#27391=CARTESIAN_POINT('Ctrl Pts',(32.2079531230124,34.9673589385144,-1.51082436306572));
#27392=CARTESIAN_POINT('Ctrl Pts',(32.1569814991446,34.9673055927269,-1.512058227279));
#27393=CARTESIAN_POINT('Ctrl Pts',(32.1067603493757,34.9672499217566,-1.51333518230822));
#27394=CARTESIAN_POINT('Ctrl Pts',(32.0554367657631,34.9671908102208,-1.51468303813505));
#27395=CARTESIAN_POINT('Ctrl Pts',(32.0053752916507,34.9671331523098,-1.51599774854364));
#27396=CARTESIAN_POINT('Ctrl Pts',(31.9542650752308,34.9670721879268,-1.51738077462803));
#27397=CARTESIAN_POINT('Ctrl Pts',(31.9003392718784,34.9670065776396,-1.51886693662987));
#27398=CARTESIAN_POINT('Ctrl Pts',(31.8778362033488,34.9669791986726,-1.51948710736994));
#27399=CARTESIAN_POINT('Ctrl Pts',(31.8548422465647,34.9669510097079,-1.52012527669195));
#27400=CARTESIAN_POINT('Ctrl Pts',(31.8312262657831,34.9669219190816,-1.5207838890893));
#27401=CARTESIAN_POINT('Ctrl Pts',(31.7273802318769,34.9667939995094,-1.52367999092727));
#27402=CARTESIAN_POINT('Ctrl Pts',(31.6210019634564,34.9666588880294,-1.52670831990391));
#27403=CARTESIAN_POINT('Ctrl Pts',(31.5129311113832,34.9665259706005,-1.52968152042074));
#27404=CARTESIAN_POINT('Ctrl Pts',(31.4048670765154,34.9663930615562,-1.53265453338543));
#27405=CARTESIAN_POINT('Ctrl Pts',(31.295110396828,34.9662624173991,-1.53557057541609));
#27406=CARTESIAN_POINT('Ctrl Pts',(31.1845493642852,34.9661438310284,-1.53823056067695));
#27407=CARTESIAN_POINT('Ctrl Pts',(31.1321570104766,34.9660876356498,-1.53949106707516));
#27408=CARTESIAN_POINT('Ctrl Pts',(31.0795847658967,34.9660341471942,-1.54069407696177));
#27409=CARTESIAN_POINT('Ctrl Pts',(31.0269312050905,34.9659843676727,-1.54181935957432));
#27410=CARTESIAN_POINT('Ctrl Pts',(30.9325025960689,34.9658950933502,-1.5438374352796));
#27411=CARTESIAN_POINT('Ctrl Pts',(30.8378102330027,34.9658178028119,-1.54560383003055));
#27412=CARTESIAN_POINT('Ctrl Pts',(30.743359924284,34.9657577677723,-1.54697518213503));
#27413=CARTESIAN_POINT('Ctrl Pts',(30.6608249248197,34.965705306409,-1.54817353232302));
#27414=CARTESIAN_POINT('Ctrl Pts',(30.5784749808876,34.9656660234083,-1.5490700665616));
#27415=CARTESIAN_POINT('Ctrl Pts',(30.4966730088978,34.9656427667437,-1.54959005157024));
#27416=CARTESIAN_POINT('',(30.5,34.9699609326822,1.44976976333442));
#27417=CARTESIAN_POINT('Origin',(30.5,0.,0.));
#27418=CARTESIAN_POINT('Ctrl Pts',(30.5051992612603,34.9699071381489,1.44903843638966));
#27419=CARTESIAN_POINT('Ctrl Pts',(30.6030952980657,34.9698787568567,1.44976082626916));
#27420=CARTESIAN_POINT('Ctrl Pts',(30.7001121880334,34.9698264221104,1.45104998650339));
#27421=CARTESIAN_POINT('Ctrl Pts',(30.7969947619801,34.9697577270266,1.45274237549662));
#27422=CARTESIAN_POINT('Ctrl Pts',(30.8545454823776,34.9697169203945,1.45374769773142));
#27423=CARTESIAN_POINT('Ctrl Pts',(30.9120492097055,34.9696702850817,1.45489634227782));
#27424=CARTESIAN_POINT('Ctrl Pts',(30.9696671110348,34.969619048359,1.45616096255286));
#27425=CARTESIAN_POINT('Ctrl Pts',(31.0687356284601,34.969530951673,1.45833535719175));
#27426=CARTESIAN_POINT('Ctrl Pts',(31.1681385828748,34.9694292858246,1.46085179879274));
#27427=CARTESIAN_POINT('Ctrl Pts',(31.2685908593294,34.9693191238307,1.46356721252908));
#27428=CARTESIAN_POINT('Ctrl Pts',(31.3711796386287,34.9692066188196,1.46634037995083));
#27429=CARTESIAN_POINT('Ctrl Pts',(31.4748629185041,34.9690851710715,1.46932276608686));
#27430=CARTESIAN_POINT('Ctrl Pts',(31.5804543970455,34.9689598486836,1.47236951553031));
#27431=CARTESIAN_POINT('Ctrl Pts',(31.6427002532107,34.9688859715163,1.47416556508136));
#27432=CARTESIAN_POINT('Ctrl Pts',(31.7056101943778,34.9688107472907,1.47598400420438));
#27433=CARTESIAN_POINT('Ctrl Pts',(31.7693590594472,34.9687353433411,1.47779256103941));
#27434=CARTESIAN_POINT('Ctrl Pts',(31.8369567664636,34.9686553868731,1.47971030961302));
#27435=CARTESIAN_POINT('Ctrl Pts',(31.8998289473024,34.9685826953726,1.4814535614827));
#27436=CARTESIAN_POINT('Ctrl Pts',(31.9584912820088,34.9685172658125,1.48302365833457));
#27437=CARTESIAN_POINT('Ctrl Pts',(32.0219681801222,34.9684464662861,1.484722616932));
#27438=CARTESIAN_POINT('Ctrl Pts',(32.0805160965731,34.9683841232146,1.48621979971339));
#27439=CARTESIAN_POINT('Ctrl Pts',(32.1348442130199,34.9683291276834,1.48754049944246));
#27440=CARTESIAN_POINT('Ctrl Pts',(32.1955320114797,34.9682676943423,1.48901580107678));
#27441=CARTESIAN_POINT('Ctrl Pts',(32.2509543450019,34.968215382145,1.49027186778443));
#27442=CARTESIAN_POINT('Ctrl Pts',(32.3021641802425,34.9681701141151,1.491355705848));
#27443=CARTESIAN_POINT('Ctrl Pts',(32.3568725417848,34.968121753488,1.49251358898425));
#27444=CARTESIAN_POINT('Ctrl Pts',(32.4067738547302,34.9680813901957,1.49347579219525));
#27445=CARTESIAN_POINT('Ctrl Pts',(32.4532143425731,34.9680466762593,1.49429647043739));
#27446=CARTESIAN_POINT('Ctrl Pts',(32.5024778890085,34.9680098521065,1.49516703667319));
#27447=CARTESIAN_POINT('Ctrl Pts',(32.5478477692412,34.9679793561973,1.49587895592534));
#27448=CARTESIAN_POINT('Ctrl Pts',(32.590987301899,34.9679531603257,1.49648137333632));
#27449=CARTESIAN_POINT('Ctrl Pts',(32.6362425762296,34.9679256796998,1.49711333579665));
#27450=CARTESIAN_POINT('Ctrl Pts',(32.6790438910131,34.9679029082458,1.49762527612465));
#27451=CARTESIAN_POINT('Ctrl Pts',(32.7213614276251,34.9678837287556,1.49804900699199));
#27452=CARTESIAN_POINT('Ctrl Pts',(32.7633326545624,34.9678647062227,1.49846927021659));
#27453=CARTESIAN_POINT('Ctrl Pts',(32.8048283340688,34.9678491963779,1.49880319667876));
#27454=CARTESIAN_POINT('Ctrl Pts',(32.8478112859608,34.9678375791943,1.49905168880693));
#27455=CARTESIAN_POINT('Ctrl Pts',(32.8880595868429,34.9678267011163,1.49928437142879));
#27456=CARTESIAN_POINT('Ctrl Pts',(32.9296120625591,34.9678192143483,1.49944259954572));
#27457=CARTESIAN_POINT('Ctrl Pts',(32.9741124736802,34.9678170031323,1.49949475964765));
#27458=CARTESIAN_POINT('Ctrl Pts',(32.9824658917578,34.9678165880528,1.49950455090861));
#27459=CARTESIAN_POINT('Ctrl Pts',(32.9909232824608,34.9678163642397,1.49951049395371));
#27460=CARTESIAN_POINT('Ctrl Pts',(32.9994956564548,34.9678163521984,1.49951221389311));
#27461=CARTESIAN_POINT('Ctrl Pts',(33.0359167076011,34.9678163010393,1.49951952132053));
#27462=CARTESIAN_POINT('Ctrl Pts',(33.0737648470632,34.9678163144542,1.49952600456098));
#27463=CARTESIAN_POINT('Ctrl Pts',(33.1138039348095,34.9678165569183,1.49953164904713));
#27464=CARTESIAN_POINT('Ctrl Pts',(33.2457861392316,34.9678173561608,1.49955025515846));
#27465=CARTESIAN_POINT('Ctrl Pts',(33.3718058092169,34.9678177616076,1.49955552940343));
#27466=CARTESIAN_POINT('Ctrl Pts',(33.4990121011461,34.9678181023248,1.49956083536768));
#27467=CARTESIAN_POINT('Ctrl Pts',(33.6624238693916,34.967818540017,1.49956765151637));
#27468=CARTESIAN_POINT('Ctrl Pts',(33.8277938592882,34.9678188708892,1.49957452000977));
#27469=CARTESIAN_POINT('Ctrl Pts',(33.9926457806312,34.9678194856963,1.49958605843696));
#27470=CARTESIAN_POINT('Ctrl Pts',(34.3223496233171,34.9678207153105,1.49960913529135));
#27471=CARTESIAN_POINT('Ctrl Pts',(34.6499811917881,34.9678230806641,1.49965089188094));
#27472=CARTESIAN_POINT('Ctrl Pts',(34.9787437607291,34.9678240597269,1.49966841302101));
#27473=CARTESIAN_POINT('Ctrl Pts',(35.1431250451996,34.9678245492583,1.49967717359104));
#27474=CARTESIAN_POINT('Ctrl Pts',(35.3077890797877,34.967824692217,1.4996798752987));
#27475=CARTESIAN_POINT('Ctrl Pts',(35.4723919953984,34.9678249110676,1.49968390458379));
#27476=CARTESIAN_POINT('Ctrl Pts',(35.9662007422305,34.9678255676193,1.49969599243905));
#27477=CARTESIAN_POINT('Ctrl Pts',(36.459459418267,34.9678269071983,1.49972002849123));
#27478=CARTESIAN_POINT('Ctrl Pts',(36.9527108273738,34.9678287658477,1.49975356610212));
#27479=CARTESIAN_POINT('Ctrl Pts',(38.1015495523822,34.9678330948538,1.49983167901864));
#27480=CARTESIAN_POINT('Ctrl Pts',(39.2503488559568,34.9678402396984,1.49996133572172));
#27481=CARTESIAN_POINT('Ctrl Pts',(40.4000634893725,34.9678419791559,1.49999290859453));
#27482=CARTESIAN_POINT('Ctrl Pts',(6.89999999997365,9.46599415780712,5.65979197164529));
#27483=CARTESIAN_POINT('Ctrl Pts',(6.99168932310453,9.49787619923353,5.60729410195164));
#27484=CARTESIAN_POINT('Ctrl Pts',(7.08405956072215,9.52934434473075,5.55450818731572));
#27485=CARTESIAN_POINT('Ctrl Pts',(8.15473535981985,9.88659437915723,4.94320927931173));
#27486=CARTESIAN_POINT('Ctrl Pts',(9.17052309187647,10.1553288976265,4.34956920012189));
#27487=CARTESIAN_POINT('Ctrl Pts',(11.249912418623,10.5681406908193,3.24757657546859));
#27488=CARTESIAN_POINT('Ctrl Pts',(12.2613271155137,10.7096926815135,2.71507294053767));
#27489=CARTESIAN_POINT('Ctrl Pts',(14.3530613265277,10.9182780492489,1.75089621035865));
#27490=CARTESIAN_POINT('Ctrl Pts',(15.3683896576347,10.9736589531833,1.30024364084097));
#27491=CARTESIAN_POINT('Ctrl Pts',(17.4699484560063,11.0479347559914,0.51160650808575));
#27492=CARTESIAN_POINT('Ctrl Pts',(18.4899441076999,11.0518486975415,0.154966618543408));
#27493=CARTESIAN_POINT('Ctrl Pts',(19.8459385111079,11.0525063200436,-0.227738630131172));
#27494=CARTESIAN_POINT('Ctrl Pts',(20.3436052070642,11.0499443867429,-0.364012293347548));
#27495=CARTESIAN_POINT('Ctrl Pts',(21.3765735172499,11.0391187302377,-0.626365466004486));
#27496=CARTESIAN_POINT('Ctrl Pts',(22.1786513408684,11.0271780970655,-0.80148237085404));
#27497=CARTESIAN_POINT('Ctrl Pts',(22.8524711894103,11.0190184236597,-0.927590054426941));
#27498=CARTESIAN_POINT('Ctrl Pts',(23.1034772575406,11.015636270466,-0.973361071581967));
#27499=CARTESIAN_POINT('Ctrl Pts',(23.6153488598143,11.0082046691873,-1.06157978958535));
#27500=CARTESIAN_POINT('Ctrl Pts',(24.2640912191231,10.9980907558832,-1.16309571993123));
#27501=CARTESIAN_POINT('Ctrl Pts',(24.9252112071703,10.9882975006411,-1.25112898708132));
#27502=CARTESIAN_POINT('Ctrl Pts',(25.3924209938587,10.9823391891697,-1.30426168416562));
#27503=CARTESIAN_POINT('Ctrl Pts',(25.6607104515486,10.9792975977554,-1.332046615497));
#27504=CARTESIAN_POINT('Ctrl Pts',(25.7950739758558,10.9779150347045,-1.34502686686554));
#27505=CARTESIAN_POINT('Ctrl Pts',(26.2512918422651,10.9735046934062,-1.38748529291552));
#27506=CARTESIAN_POINT('Ctrl Pts',(27.3073301682004,10.9653764904263,-1.45732017866833));
#27507=CARTESIAN_POINT('Ctrl Pts',(28.3319194320811,10.9609947024269,-1.48237708919284));
#27508=CARTESIAN_POINT('Ctrl Pts',(29.1280123944214,10.9582092660149,-1.50394716937725));
#27509=CARTESIAN_POINT('Ctrl Pts',(29.4779818455993,10.9573324846489,-1.51103964894258));
#27510=CARTESIAN_POINT('Ctrl Pts',(29.9466600480359,10.9567800220405,-1.51533483257754));
#27511=CARTESIAN_POINT('Ctrl Pts',(30.4585980273686,10.956656708735,-1.51632751174059));
#27512=CARTESIAN_POINT('Ctrl Pts',(31.4732549878281,10.9572594965941,-1.51158385370563));
#27513=CARTESIAN_POINT('Ctrl Pts',(32.3455845021632,10.95879335959,-1.4999511927851));
#27514=CARTESIAN_POINT('Ctrl Pts',(33.1628510802405,10.9587933798862,-1.49997453311311));
#27515=CARTESIAN_POINT('Ctrl Pts',(33.4532441810442,10.9587933789851,-1.49997366471359));
#27516=CARTESIAN_POINT('Ctrl Pts',(33.7813843869345,10.9587933812939,-1.49997637381128));
#27517=CARTESIAN_POINT('Ctrl Pts',(34.2755379701535,10.9587933817727,-1.49997699476315));
#27518=CARTESIAN_POINT('Ctrl Pts',(34.8102302793009,10.9587933869434,-1.49998326277599));
#27519=CARTESIAN_POINT('Ctrl Pts',(35.6332452367756,10.9587933876415,-1.49998412101817));
#27520=CARTESIAN_POINT('Ctrl Pts',(36.2915450349079,10.9587933890033,-1.49998577371297));
#27521=CARTESIAN_POINT('Ctrl Pts',(38.1020137670942,10.9587933908629,-1.49998803993575));
#27522=CARTESIAN_POINT('Ctrl Pts',(39.5833333333333,10.9587934006931,-1.5));
#27523=CARTESIAN_POINT('Ctrl Pts',(40.9,10.9587934006931,-1.5));
#27524=CARTESIAN_POINT('Ctrl Pts',(6.65963435785827,13.0027682689653,8.56288377493212));
#27525=CARTESIAN_POINT('Ctrl Pts',(6.7513219377677,13.050957789036,8.49067817166156));
#27526=CARTESIAN_POINT('Ctrl Pts',(6.84370278928156,13.0985893115687,8.41801298642698));
#27527=CARTESIAN_POINT('Ctrl Pts',(7.91483960325934,13.6397807532085,7.57680655910808));
#27528=CARTESIAN_POINT('Ctrl Pts',(8.9325509112231,14.0543934435321,6.75518385076231));
#27529=CARTESIAN_POINT('Ctrl Pts',(11.0192135814157,14.7040310435558,5.22065437877307));
#27530=CARTESIAN_POINT('Ctrl Pts',(12.0340542508324,14.9356992206141,4.4769598695545));
#27531=CARTESIAN_POINT('Ctrl Pts',(14.1407660172285,15.2883456800052,3.1214593369057));
#27532=CARTESIAN_POINT('Ctrl Pts',(15.1616568764318,15.3931503655329,2.48732138966201));
#27533=CARTESIAN_POINT('Ctrl Pts',(17.287218760307,15.5446125872455,1.36959877283814));
#27534=CARTESIAN_POINT('Ctrl Pts',(18.3145546794907,15.5707395254148,0.864902786641511));
#27535=CARTESIAN_POINT('Ctrl Pts',(19.6926214867647,15.5935126543779,0.318801403605146));
#27536=CARTESIAN_POINT('Ctrl Pts',(20.1945263626901,15.5977145841048,0.125373946234778));
#27537=CARTESIAN_POINT('Ctrl Pts',(21.2420076978203,15.5972978704292,-0.248868189963681));
#27538=CARTESIAN_POINT('Ctrl Pts',(22.0575126096201,15.5901933457539,-0.499284562147392));
#27539=CARTESIAN_POINT('Ctrl Pts',(22.7441078663834,15.5856475377419,-0.679992377552244));
#27540=CARTESIAN_POINT('Ctrl Pts',(22.9980856324395,15.5834353094767,-0.745267685418833));
#27541=CARTESIAN_POINT('Ctrl Pts',(23.5177883906687,15.5778337615218,-0.871419538176181));
#27542=CARTESIAN_POINT('Ctrl Pts',(24.1766640555165,15.569151455817,-1.01665680544524));
#27543=CARTESIAN_POINT('Ctrl Pts',(24.8496697365589,15.560128822227,-1.14287321247013));
#27544=CARTESIAN_POINT('Ctrl Pts',(25.3259254544069,15.554601684436,-1.2191404135396));
#27545=CARTESIAN_POINT('Ctrl Pts',(25.5996882691236,15.5518109321211,-1.2590574298324));
#27546=CARTESIAN_POINT('Ctrl Pts',(25.7368188560809,15.550561003587,-1.27770917936971));
#27547=CARTESIAN_POINT('Ctrl Pts',(26.2030586507879,15.5466206431081,-1.33878235986071));
#27548=CARTESIAN_POINT('Ctrl Pts',(27.2845562696213,15.5388831179539,-1.43928616936987));
#27549=CARTESIAN_POINT('Ctrl Pts',(28.3146233763975,15.534108117874,-1.47473229777557));
#27550=CARTESIAN_POINT('Ctrl Pts',(29.1121433593266,15.5313810124223,-1.5053783917148));
#27551=CARTESIAN_POINT('Ctrl Pts',(29.4693616319656,15.5305221749293,-1.51558516408219));
#27552=CARTESIAN_POINT('Ctrl Pts',(29.9425518103672,15.5299808253862,-1.52169686437909));
#27553=CARTESIAN_POINT('Ctrl Pts',(30.4595136734855,15.5298599056894,-1.52312339822457));
#27554=CARTESIAN_POINT('Ctrl Pts',(31.4800666545032,15.5304501241615,-1.51634797661239));
#27555=CARTESIAN_POINT('Ctrl Pts',(32.3507119180564,15.5319509809364,-1.4999128955352));
#27556=CARTESIAN_POINT('Ctrl Pts',(33.1621363777215,15.5319505779396,-1.49995461572564));
#27557=CARTESIAN_POINT('Ctrl Pts',(33.4535196029878,15.5319505880019,-1.49995304854269));
#27558=CARTESIAN_POINT('Ctrl Pts',(33.7812306484551,15.5319505396377,-1.49995788616631));
#27559=CARTESIAN_POINT('Ctrl Pts',(34.2755524327802,15.531950526851,-1.49995898984267));
#27560=CARTESIAN_POINT('Ctrl Pts',(34.8101578274898,15.5319504091692,-1.49997016508529));
#27561=CARTESIAN_POINT('Ctrl Pts',(35.6332135248365,15.5319503927198,-1.49997169422773));
#27562=CARTESIAN_POINT('Ctrl Pts',(36.2914988048216,15.5319503616369,-1.49997464065555));
#27563=CARTESIAN_POINT('Ctrl Pts',(38.1019885414694,15.5319503187541,-1.49997868009126));
#27564=CARTESIAN_POINT('Ctrl Pts',(39.5833333333333,15.5319500929849,-1.5));
#27565=CARTESIAN_POINT('Ctrl Pts',(40.9,15.5319500929849,-1.5));
#27566=CARTESIAN_POINT('Ctrl Pts',(6.47503677058814,19.2049631177014,13.6264850125633));
#27567=CARTESIAN_POINT('Ctrl Pts',(6.56582707216344,19.2807931407427,13.5206117629928));
#27568=CARTESIAN_POINT('Ctrl Pts',(6.65722187862393,19.3557456396964,13.4141026801341));
#27569=CARTESIAN_POINT('Ctrl Pts',(7.71979853459931,20.2113974185276,12.1774082172639));
#27570=CARTESIAN_POINT('Ctrl Pts',(8.72714740265586,20.876585861408,10.9649265084515));
#27571=CARTESIAN_POINT('Ctrl Pts',(10.792252425961,21.9312131301472,8.69413764846818));
#27572=CARTESIAN_POINT('Ctrl Pts',(11.8008983729842,22.3203974544121,7.58577239973431));
#27573=CARTESIAN_POINT('Ctrl Pts',(13.892634394048,22.9231109701401,5.56042793834188));
#27574=CARTESIAN_POINT('Ctrl Pts',(14.910936596525,23.1162450123325,4.60683703173286));
#27575=CARTESIAN_POINT('Ctrl Pts',(17.0374816014601,23.4053158267904,2.91606182242837));
#27576=CARTESIAN_POINT('Ctrl Pts',(18.0678529336714,23.4724397837998,2.15006970557796));
#27577=CARTESIAN_POINT('Ctrl Pts',(19.4632774216583,23.5361137002685,1.31129970902877));
#27578=CARTESIAN_POINT('Ctrl Pts',(19.9690853949367,23.5527456051548,1.01646669656859));
#27579=CARTESIAN_POINT('Ctrl Pts',(21.0306109698709,23.5717577824589,0.441678056412672));
#27580=CARTESIAN_POINT('Ctrl Pts',(21.8626014988188,23.5739085372705,0.0543003442681426));
#27581=CARTESIAN_POINT('Ctrl Pts',(22.5665651705189,23.5761789143631,-0.226484889079843));
#27582=CARTESIAN_POINT('Ctrl Pts',(22.8246411038756,23.5761448043361,-0.326902916553465));
#27583=CARTESIAN_POINT('Ctrl Pts',(23.3554232774669,23.5740054132278,-0.522054743089693));
#27584=CARTESIAN_POINT('Ctrl Pts',(24.0293769285439,23.5680817805141,-0.747005858788648));
#27585=CARTESIAN_POINT('Ctrl Pts',(24.7209631427047,23.560586503548,-0.94339358139433));
#27586=CARTESIAN_POINT('Ctrl Pts',(25.2118242719342,23.5558940963915,-1.06233480615607));
#27587=CARTESIAN_POINT('Ctrl Pts',(25.4945546545947,23.5535795021665,-1.12470144437592));
#27588=CARTESIAN_POINT('Ctrl Pts',(25.6362544160062,23.5525764277764,-1.15385183559377));
#27589=CARTESIAN_POINT('Ctrl Pts',(26.1191683853685,23.5495095529483,-1.24953281052836));
#27590=CARTESIAN_POINT('Ctrl Pts',(27.244410780189,23.5425023713064,-1.40715534997208));
#27591=CARTESIAN_POINT('Ctrl Pts',(28.2843056152442,23.5370396227258,-1.46065929315376));
#27592=CARTESIAN_POINT('Ctrl Pts',(29.0843244121809,23.5344215873996,-1.50737208683505));
#27593=CARTESIAN_POINT('Ctrl Pts',(29.4542021761287,23.5335942286398,-1.52336782189617));
#27594=CARTESIAN_POINT('Ctrl Pts',(29.9352997409898,23.5330734925559,-1.53271512054377));
#27595=CARTESIAN_POINT('Ctrl Pts',(30.4610555884278,23.532957187389,-1.5349453613852));
#27596=CARTESIAN_POINT('Ctrl Pts',(31.4919316519535,23.5335262680548,-1.52450364515754));
#27597=CARTESIAN_POINT('Ctrl Pts',(32.3596576160514,23.5349731541844,-1.49979324124413));
#27598=CARTESIAN_POINT('Ctrl Pts',(33.1608710165812,23.5349736853906,-1.49989213988255));
#27599=CARTESIAN_POINT('Ctrl Pts',(33.4539865796869,23.5349736699323,-1.49988845489238));
#27600=CARTESIAN_POINT('Ctrl Pts',(33.780948091659,23.5349737329761,-1.49989993226727));
#27601=CARTESIAN_POINT('Ctrl Pts',(34.275564602361,23.5349737489117,-1.49990256114204));
#27602=CARTESIAN_POINT('Ctrl Pts',(34.810021467207,23.5349738998239,-1.49992910993535));
#27603=CARTESIAN_POINT('Ctrl Pts',(35.6331489543767,23.5349739207807,-1.49993274473985));
#27604=CARTESIAN_POINT('Ctrl Pts',(36.2914097700016,23.5349739606187,-1.4999397448351));
#27605=CARTESIAN_POINT('Ctrl Pts',(38.1019375614968,23.5349740154737,-1.49994934328327));
#27606=CARTESIAN_POINT('Ctrl Pts',(39.5833333333333,23.5349743044955,-1.5));
#27607=CARTESIAN_POINT('Ctrl Pts',(40.9,23.5349743044955,-1.5));
#27608=CARTESIAN_POINT('Ctrl Pts',(6.39840282685635,25.4797798158266,18.5950148818));
#27609=CARTESIAN_POINT('Ctrl Pts',(6.48879582230594,25.5825069307027,18.455456538043));
#27610=CARTESIAN_POINT('Ctrl Pts',(6.57973810483189,25.684006582131,18.3151558806717));
#27611=CARTESIAN_POINT('Ctrl Pts',(7.63881202209714,26.8457843562122,16.6821095714367));
#27612=CARTESIAN_POINT('Ctrl Pts',(8.64206536867565,27.7524045864227,15.0805562774161));
#27613=CARTESIAN_POINT('Ctrl Pts',(10.6943835463645,29.194220471563,12.08639394536));
#27614=CARTESIAN_POINT('Ctrl Pts',(11.6986850371144,29.7340826089764,10.6188960618635));
#27615=CARTESIAN_POINT('Ctrl Pts',(13.7736723466472,30.5724457120527,7.9480571508383));
#27616=CARTESIAN_POINT('Ctrl Pts',(14.7865355152845,30.8496813329458,6.68379951334874));
#27617=CARTESIAN_POINT('Ctrl Pts',(16.895644387614,31.2681094727719,4.44867953439714));
#27618=CARTESIAN_POINT('Ctrl Pts',(17.921113585793,31.3748718553479,3.42955614780409));
#27619=CARTESIAN_POINT('Ctrl Pts',(19.3111115725317,31.4778602005301,2.31180057560694));
#27620=CARTESIAN_POINT('Ctrl Pts',(19.8164097330209,31.5068304778962,1.91755167896536));
#27621=CARTESIAN_POINT('Ctrl Pts',(20.8772665291465,31.5450009606978,1.14804732053491));
#27622=CARTESIAN_POINT('Ctrl Pts',(21.7126526899651,31.5565752055434,0.625757760628938));
#27623=CARTESIAN_POINT('Ctrl Pts',(22.4233939916368,31.5658469864011,0.244774266221906));
#27624=CARTESIAN_POINT('Ctrl Pts',(22.68321700305,31.568070163829,0.109074102068986));
#27625=CARTESIAN_POINT('Ctrl Pts',(23.2191843843282,31.5695528321153,-0.155714853804433));
#27626=CARTESIAN_POINT('Ctrl Pts',(23.9014490792895,31.5665856540486,-0.461901703286707));
#27627=CARTESIAN_POINT('Ctrl Pts',(24.6052033552109,31.5607844376464,-0.730987709817266));
#27628=CARTESIAN_POINT('Ctrl Pts',(25.1069219885717,31.5570192016244,-0.89479518126793));
#27629=CARTESIAN_POINT('Ctrl Pts',(25.3966703145091,31.5552253028176,-0.980957842597307));
#27630=CARTESIAN_POINT('Ctrl Pts',(25.5420691491796,31.5544886793522,-1.02128571697646));
#27631=CARTESIAN_POINT('Ctrl Pts',(26.0386675456483,31.5523567719375,-1.15405115562806));
#27632=CARTESIAN_POINT('Ctrl Pts',(27.2041996425261,31.5461367082151,-1.37405103438868));
#27633=CARTESIAN_POINT('Ctrl Pts',(28.254481539011,31.5399727189289,-1.44553527377015));
#27634=CARTESIAN_POINT('Ctrl Pts',(29.0567817440806,31.5374655658645,-1.50856328668891));
#27635=CARTESIAN_POINT('Ctrl Pts',(29.4392037716731,31.5366692491296,-1.53093305020556));
#27636=CARTESIAN_POINT('Ctrl Pts',(29.9281985709061,31.536168682902,-1.54360558359609));
#27637=CARTESIAN_POINT('Ctrl Pts',(30.4627354290944,31.5360567738141,-1.54671304059522));
#27638=CARTESIAN_POINT('Ctrl Pts',(31.5039222132187,31.5366047697957,-1.53240580330097));
#27639=CARTESIAN_POINT('Ctrl Pts',(32.3686614831274,31.5379963364647,-1.49961223537188));
#27640=CARTESIAN_POINT('Ctrl Pts',(33.1596379899179,31.5379973429874,-1.49979803313558));
#27641=CARTESIAN_POINT('Ctrl Pts',(33.4544864001145,31.5379973136915,-1.49979103760183));
#27642=CARTESIAN_POINT('Ctrl Pts',(33.7806952343975,31.5379974331442,-1.49981257637976));
#27643=CARTESIAN_POINT('Ctrl Pts',(34.2756055948936,31.5379974633363,-1.49981748473541));
#27644=CARTESIAN_POINT('Ctrl Pts',(34.8099061252942,31.5379977492716,-1.49986722177693));
#27645=CARTESIAN_POINT('Ctrl Pts',(35.6331043028646,31.5379977889784,-1.49987402634112));
#27646=CARTESIAN_POINT('Ctrl Pts',(36.2913385913736,31.5379978644599,-1.49988713966987));
#27647=CARTESIAN_POINT('Ctrl Pts',(38.1019015852784,31.537997968394,-1.49990511666357));
#27648=CARTESIAN_POINT('Ctrl Pts',(39.5833333333333,31.5379985160061,-1.5));
#27649=CARTESIAN_POINT('Ctrl Pts',(40.9,31.5379985160061,-1.5));
#27650=CARTESIAN_POINT('Ctrl Pts',(6.37427268165564,28.1741189428499,20.7176664141567));
#27651=CARTESIAN_POINT('Ctrl Pts',(6.46448755772838,28.2883460540946,20.5636424771022));
#27652=CARTESIAN_POINT('Ctrl Pts',(6.55522687426754,28.4011972468989,20.4088293925213));
#27653=CARTESIAN_POINT('Ctrl Pts',(7.61282240204204,29.693787896276,18.6056139772311));
#27654=CARTESIAN_POINT('Ctrl Pts',(8.61454082730176,30.703424507615,16.8370699794085));
#27655=CARTESIAN_POINT('Ctrl Pts',(10.6618274824665,32.3104201819496,13.5325068155167));
#27656=CARTESIAN_POINT('Ctrl Pts',(11.6645377987076,32.9144254040795,11.9110180488694));
#27657=CARTESIAN_POINT('Ctrl Pts',(13.7331445959134,33.8529424117878,8.96386257277559));
#27658=CARTESIAN_POINT('Ctrl Pts',(14.7439932704909,34.1658004948675,7.56674532731095));
#27659=CARTESIAN_POINT('Ctrl Pts',(16.8461035490385,34.6388264066738,5.10012840374637));
#27660=CARTESIAN_POINT('Ctrl Pts',(17.8695058124616,34.7622645166785,3.97333364734334));
#27661=CARTESIAN_POINT('Ctrl Pts',(19.2561174443541,34.8817349492475,2.73821070416469));
#27662=CARTESIAN_POINT('Ctrl Pts',(19.7609345646798,34.9159214541564,2.30176586395499));
#27663=CARTESIAN_POINT('Ctrl Pts',(20.8205141053453,34.9621410370326,1.45015687002429));
#27664=CARTESIAN_POINT('Ctrl Pts',(21.6560023791939,34.9776907709078,0.871078443387));
#27665=CARTESIAN_POINT('Ctrl Pts',(22.3682688599883,34.989939594886,0.44777828592714));
#27666=CARTESIAN_POINT('Ctrl Pts',(22.6285200842947,34.9931281975259,0.297086276283266));
#27667=CARTESIAN_POINT('Ctrl Pts',(23.1658603614091,34.9961605697035,0.00273379297028335));
#27668=CARTESIAN_POINT('Ctrl Pts',(23.8505975407037,34.9944676948756,-0.338068372298848));
#27669=CARTESIAN_POINT('Ctrl Pts',(24.5583968797874,34.9894056975888,-0.638319272935672));
#27670=CARTESIAN_POINT('Ctrl Pts',(25.0640148551739,34.9860476379143,-0.821498314632837));
#27671=CARTESIAN_POINT('Ctrl Pts',(25.3563632502514,34.9844821378475,-0.917977493583088));
#27672=CARTESIAN_POINT('Ctrl Pts',(25.503160007456,34.9838621425449,-0.963163948801062));
#27673=CARTESIAN_POINT('Ctrl Pts',(26.0049713545738,34.982139121313,-1.11209382847183));
#27674=CARTESIAN_POINT('Ctrl Pts',(27.1869304722337,34.9762666166019,-1.35965020681435));
#27675=CARTESIAN_POINT('Ctrl Pts',(28.2418054197051,34.9698003983093,-1.43886806122646));
#27676=CARTESIAN_POINT('Ctrl Pts',(29.0450356043991,34.9673414359535,-1.50892754055989));
#27677=CARTESIAN_POINT('Ctrl Pts',(29.4328041419752,34.9665583691038,-1.53413528152412));
#27678=CARTESIAN_POINT('Ctrl Pts',(29.9251825362975,34.9660664512209,-1.54824951859995));
#27679=CARTESIAN_POINT('Ctrl Pts',(30.4634799414205,34.9659564211645,-1.55174636239756));
#27680=CARTESIAN_POINT('Ctrl Pts',(31.5090833787051,34.9664954410524,-1.53574598606795));
#27681=CARTESIAN_POINT('Ctrl Pts',(32.3725304400172,34.9678633362529,-1.49952340891733));
#27682=CARTESIAN_POINT('Ctrl Pts',(33.1591152593399,34.9678645826042,-1.49975189997365));
#27683=CARTESIAN_POINT('Ctrl Pts',(33.4547063903441,34.9678645463389,-1.49974326694615));
#27684=CARTESIAN_POINT('Ctrl Pts',(33.7805921021893,34.9678646942577,-1.49976974530861));
#27685=CARTESIAN_POINT('Ctrl Pts',(34.2756282408745,34.9678647316484,-1.49977576894615));
#27686=CARTESIAN_POINT('Ctrl Pts',(34.8098603973427,34.967865085736,-1.49983687714898));
#27687=CARTESIAN_POINT('Ctrl Pts',(35.6330886763766,34.9678651349076,-1.49984523535833));
#27688=CARTESIAN_POINT('Ctrl Pts',(36.2913112329655,34.9678652283802,-1.49986134640235));
#27689=CARTESIAN_POINT('Ctrl Pts',(38.1018888107018,34.9678653570876,-1.49988343135295));
#27690=CARTESIAN_POINT('Ctrl Pts',(39.5833333333333,34.9678660352249,-1.5));
#27691=CARTESIAN_POINT('Ctrl Pts',(40.9,34.9678660352249,-1.5));
#27692=CARTESIAN_POINT('',(40.9,32.9658914637539,-1.50000000000001));
#27693=CARTESIAN_POINT('Ctrl Pts',(40.9,32.9658914637539,-1.50000000000001));
#27694=CARTESIAN_POINT('Ctrl Pts',(40.9,33.466386268912,-1.50000000000001));
#27695=CARTESIAN_POINT('Ctrl Pts',(40.9,33.9668810740701,-1.50000000000001));
#27696=CARTESIAN_POINT('Ctrl Pts',(40.9,34.4673758792282,-1.50000000000001));
#27697=CARTESIAN_POINT('',(38.,32.9658914637539,-1.5));
#27698=CARTESIAN_POINT('Ctrl Pts',(38.,32.9658914637539,-1.5));
#27699=CARTESIAN_POINT('Ctrl Pts',(38.9666666666667,32.9658914637539,-1.5));
#27700=CARTESIAN_POINT('Ctrl Pts',(39.9333333333333,32.9658914637539,-1.5));
#27701=CARTESIAN_POINT('Ctrl Pts',(40.9,32.9658914637539,-1.5));
#27702=CARTESIAN_POINT('',(37.5,32.3652591523689,-1.49999999999999));
#27703=CARTESIAN_POINT('Ctrl Pts',(37.4997714574611,32.3652585803353,-1.49990106437152));
#27704=CARTESIAN_POINT('Ctrl Pts',(37.6667294826964,32.5658056765353,-1.4999047077905));
#27705=CARTESIAN_POINT('Ctrl Pts',(37.8334450600884,32.7660568372679,-1.49990923999261));
#27706=CARTESIAN_POINT('Ctrl Pts',(37.9998166694663,32.9658909678229,-1.49991439209149));
#27707=CARTESIAN_POINT('Ctrl Pts',(20.644698628669,15.8947820241755,4.30211422042248E-15));
#27708=CARTESIAN_POINT('Ctrl Pts',(21.3839825863869,16.36544922962,-0.225731928831263));
#27709=CARTESIAN_POINT('Ctrl Pts',(22.0257484868013,16.806097479622,-0.406661554463689));
#27710=CARTESIAN_POINT('Ctrl Pts',(22.5801728644232,17.2054177529787,-0.547761868179738));
#27711=CARTESIAN_POINT('Ctrl Pts',(23.3331120273116,17.7477169095115,-0.739383947548498));
#27712=CARTESIAN_POINT('Ctrl Pts',(23.9218122708631,18.2069240887503,-0.875125428914569));
#27713=CARTESIAN_POINT('Ctrl Pts',(24.4823254534451,18.6644103290309,-0.991025114746261));
#27714=CARTESIAN_POINT('Ctrl Pts',(24.9418997081724,19.0395110482618,-1.0860532307557));
#27715=CARTESIAN_POINT('Ctrl Pts',(25.3626371148051,19.3999354975894,-1.16248640886278));
#27716=CARTESIAN_POINT('Ctrl Pts',(25.7525302890143,19.7463071016619,-1.22321331868058));
#27717=CARTESIAN_POINT('Ctrl Pts',(26.1776080056329,20.123935796648,-1.28942031554581));
#27718=CARTESIAN_POINT('Ctrl Pts',(26.5661459571655,20.485239616978,-1.3329732143938));
#27719=CARTESIAN_POINT('Ctrl Pts',(26.9267016831473,20.8313979297641,-1.36638815233963));
#27720=CARTESIAN_POINT('Ctrl Pts',(27.1778777842812,21.0725442744629,-1.38966620127371));
#27721=CARTESIAN_POINT('Ctrl Pts',(27.415486111974,21.306416246323,-1.40780557011307));
#27722=CARTESIAN_POINT('Ctrl Pts',(27.6422281942519,21.533988872658,-1.42326116565051));
#27723=CARTESIAN_POINT('Ctrl Pts',(27.8555559933386,21.7480980800036,-1.43780239305062));
#27724=CARTESIAN_POINT('Ctrl Pts',(28.1190837193165,22.0160369614212,-1.45368682614543));
#27725=CARTESIAN_POINT('Ctrl Pts',(28.4603051775928,22.3749799381825,-1.47251023690728));
#27726=CARTESIAN_POINT('Ctrl Pts',(28.6017730832564,22.5237950550031,-1.48031428449378));
#27727=CARTESIAN_POINT('Ctrl Pts',(28.7540286646466,22.6856884569089,-1.48853267939435));
#27728=CARTESIAN_POINT('Ctrl Pts',(28.9157341130969,22.8599017516109,-1.49763121638955));
#27729=CARTESIAN_POINT('Ctrl Pts',(29.4787137469343,23.4664276157722,-1.52930789194508));
#27730=CARTESIAN_POINT('Ctrl Pts',(30.1711677436424,24.2477248210898,-1.53976925233531));
#27731=CARTESIAN_POINT('Ctrl Pts',(30.8055547543771,24.9885333989172,-1.53340754825751));
#27732=CARTESIAN_POINT('Ctrl Pts',(31.1893125644442,25.4366684847488,-1.52955918190719));
#27733=CARTESIAN_POINT('Ctrl Pts',(31.5650207099053,25.8828713567937,-1.52122455967934));
#27734=CARTESIAN_POINT('Ctrl Pts',(31.9311744366546,26.3192346641773,-1.51382648741803));
#27735=CARTESIAN_POINT('Ctrl Pts',(32.1142513000292,26.5374163178691,-1.51012745128737));
#27736=CARTESIAN_POINT('Ctrl Pts',(32.2949430642633,26.7531357746899,-1.50666813405654));
#27737=CARTESIAN_POINT('Ctrl Pts',(32.4730466959744,26.9654180603387,-1.50413682057756));
#27738=CARTESIAN_POINT('Ctrl Pts',(32.5932788659896,27.108723166552,-1.50242801032117));
#27739=CARTESIAN_POINT('Ctrl Pts',(32.7123311761215,27.2504621964592,-1.50114220273815));
#27740=CARTESIAN_POINT('Ctrl Pts',(32.8301302693916,27.3903440145187,-1.50048655910759));
#27741=CARTESIAN_POINT('Ctrl Pts',(32.8868306160054,27.457673459498,-1.50017097755194));
#27742=CARTESIAN_POINT('Ctrl Pts',(32.9387123022831,27.5192120661962,-1.5));
#27743=CARTESIAN_POINT('Ctrl Pts',(33.,27.5917792275077,-1.5));
#27744=CARTESIAN_POINT('Ctrl Pts',(33.0955022515694,27.704857831427,-1.5));
#27745=CARTESIAN_POINT('Ctrl Pts',(33.2417478452381,27.8775886864723,-1.5));
#27746=CARTESIAN_POINT('Ctrl Pts',(33.3688392457043,28.0268611297194,-1.5));
#27747=CARTESIAN_POINT('Ctrl Pts',(34.266193218837,29.0808287430714,-1.5));
#27748=CARTESIAN_POINT('Ctrl Pts',(35.2319960543079,30.1809662912372,-1.49999999999999));
#27749=CARTESIAN_POINT('Ctrl Pts',(36.3004607333105,31.2401426718444,-1.49999999999999));
#27750=CARTESIAN_POINT('Ctrl Pts',(36.6891719086848,31.6254747318792,-1.49999999999999));
#27751=CARTESIAN_POINT('Ctrl Pts',(37.0893059758979,32.0028866146556,-1.49999999999999));
#27752=CARTESIAN_POINT('Ctrl Pts',(37.5,32.3652591523689,-1.49999999999999));
#27753=CARTESIAN_POINT('',(6.9,24.7737885487526,16.9192021366758));
#27754=CARTESIAN_POINT('Ctrl Pts',(6.9,24.7737885487526,16.9192021366758));
#27755=CARTESIAN_POINT('Ctrl Pts',(6.9,22.6454446228759,15.3881766950258));
#27756=CARTESIAN_POINT('Ctrl Pts',(6.90000000000115,20.4978726403359,13.8353835251886));
#27757=CARTESIAN_POINT('Ctrl Pts',(6.90000000000115,15.662481608859,10.3082122779765));
#27758=CARTESIAN_POINT('Ctrl Pts',(6.9,12.4764228571341,7.95935811114668));
#27759=CARTESIAN_POINT('Ctrl Pts',(6.9,9.46599415782504,5.6597919716369));
#27760=CARTESIAN_POINT('',(22.9245129145126,31.7706052331164,0.));
#27761=CARTESIAN_POINT('Ctrl Pts',(22.9245129145126,31.7706052331164,-4.30711063480545E-15));
#27762=CARTESIAN_POINT('Ctrl Pts',(22.7202811020963,31.7014549124251,0.0979233563002647));
#27763=CARTESIAN_POINT('Ctrl Pts',(22.5089075447093,31.6320805544326,0.203440182623873));
#27764=CARTESIAN_POINT('Ctrl Pts',(22.2913349439917,31.5632247707622,0.316637134194167));
#27765=CARTESIAN_POINT('Ctrl Pts',(21.4451770585291,31.2954389184983,0.756869465221241));
#27766=CARTESIAN_POINT('Ctrl Pts',(20.5220951556665,31.047510614715,1.35418571023244));
#27767=CARTESIAN_POINT('Ctrl Pts',(19.7671428819535,30.8612920963157,1.89915402350731));
#27768=CARTESIAN_POINT('Ctrl Pts',(19.5194773058389,30.8002022522971,2.0779333927085));
#27769=CARTESIAN_POINT('Ctrl Pts',(19.286571638609,30.7444068279677,2.25204835959331));
#27770=CARTESIAN_POINT('Ctrl Pts',(19.0728538401323,30.6939488833522,2.41532203906683));
#27771=CARTESIAN_POINT('Ctrl Pts',(18.7028555998035,30.6065937315988,2.69798906318813));
#27772=CARTESIAN_POINT('Ctrl Pts',(18.4144703596235,30.539966063932,2.93373938287718));
#27773=CARTESIAN_POINT('Ctrl Pts',(18.0642874871537,30.4582462938821,3.23398234069995));
#27774=CARTESIAN_POINT('Ctrl Pts',(17.4420927116721,30.3130489756353,3.76744532366923));
#27775=CARTESIAN_POINT('Ctrl Pts',(16.7224564418218,30.1446863488622,4.43872907330234));
#27776=CARTESIAN_POINT('Ctrl Pts',(15.9202806616111,29.9321297384067,5.24401550821529));
#27777=CARTESIAN_POINT('Ctrl Pts',(15.4090529834515,29.7966671314303,5.75722561070153));
#27778=CARTESIAN_POINT('Ctrl Pts',(14.8739602945708,29.6418940055913,6.33424649579734));
#27779=CARTESIAN_POINT('Ctrl Pts',(14.3169794331144,29.4557634846119,6.96996102647337));
#27780=CARTESIAN_POINT('Ctrl Pts',(13.8864206762829,29.3118803976566,7.46138268378477));
#27781=CARTESIAN_POINT('Ctrl Pts',(13.3867890027799,29.1311705407937,8.05270459512057));
#27782=CARTESIAN_POINT('Ctrl Pts',(12.8146824059514,28.8915984033895,8.75043091662868));
#27783=CARTESIAN_POINT('Ctrl Pts',(12.2526665517595,28.6562518085588,9.4358508309389));
#27784=CARTESIAN_POINT('Ctrl Pts',(11.6379478462804,28.3625845909803,10.231366276768));
#27785=CARTESIAN_POINT('Ctrl Pts',(10.9739250490309,27.981021293096,11.1267230319105));
#27786=CARTESIAN_POINT('Ctrl Pts',(10.5683455447964,27.747965660321,11.6735993596027));
#27787=CARTESIAN_POINT('Ctrl Pts',(10.1437415406956,27.4801235315866,12.2581093618546));
#27788=CARTESIAN_POINT('Ctrl Pts',(9.74137929176525,27.2046666925187,12.8142541611144));
#27789=CARTESIAN_POINT('Ctrl Pts',(8.72285779294234,26.5073877769786,14.2220538143138));
#27790=CARTESIAN_POINT('Ctrl Pts',(7.81323138778195,25.7100913255874,15.580948814124));
#27791=CARTESIAN_POINT('Ctrl Pts',(6.9,24.7737885487526,16.9192021366758));
#27792=CARTESIAN_POINT('Ctrl Pts',(30.5,34.9656486014478,-1.55029606206997));
#27793=CARTESIAN_POINT('Ctrl Pts',(29.9560179420817,34.7222276068062,-1.55343104498103));
#27794=CARTESIAN_POINT('Ctrl Pts',(29.4152668325132,34.4790656554127,-1.54030953139106));
#27795=CARTESIAN_POINT('Ctrl Pts',(28.8740459957565,34.2361296888632,-1.49470250846617));
#27796=CARTESIAN_POINT('Ctrl Pts',(28.3535277923439,34.0024864433252,-1.4508400330705));
#27797=CARTESIAN_POINT('Ctrl Pts',(27.8179515912466,33.7608540997398,-1.40923473841146));
#27798=CARTESIAN_POINT('Ctrl Pts',(27.2695051149491,33.5168388499063,-1.33972398862116));
#27799=CARTESIAN_POINT('Ctrl Pts',(26.9554553615883,33.3771115796287,-1.29992095446742));
#27800=CARTESIAN_POINT('Ctrl Pts',(26.6378099296971,33.2369493090937,-1.25106463707208));
#27801=CARTESIAN_POINT('Ctrl Pts',(26.3179304017917,33.0983258448229,-1.18777049128279));
#27802=CARTESIAN_POINT('Ctrl Pts',(26.1078196745982,33.0072719500184,-1.14619615520081));
#27803=CARTESIAN_POINT('Ctrl Pts',(25.8967402232745,32.9168907470981,-1.09839525532296));
#27804=CARTESIAN_POINT('Ctrl Pts',(25.6850706236774,32.8277596053404,-1.04282885388104));
#27805=CARTESIAN_POINT('Ctrl Pts',(25.6562210027417,32.8156114288513,-1.03525540156946));
#27806=CARTESIAN_POINT('Ctrl Pts',(25.6277737638215,32.8036595933923,-1.02765061224339));
#27807=CARTESIAN_POINT('Ctrl Pts',(25.5983858063598,32.7913423709803,-1.01964325944536));
#27808=CARTESIAN_POINT('Ctrl Pts',(25.1249357452756,32.5929076988546,-0.890642063078171));
#27809=CARTESIAN_POINT('Ctrl Pts',(24.1510084067019,32.1858811669087,-0.588069770626602));
#27810=CARTESIAN_POINT('Ctrl Pts',(22.9245129145126,31.7706052331164,-4.30711063480545E-15));
#27811=CARTESIAN_POINT('Origin',(40.65,0.,0.));
#27812=CARTESIAN_POINT('',(40.4,29.5330398077868,18.7829592905825));
#27813=CARTESIAN_POINT('',(40.9,29.0996231131986,18.5327260452907));
#27814=CARTESIAN_POINT('Ctrl Pts',(40.4,29.5330398077868,18.7829592905825));
#27815=CARTESIAN_POINT('Ctrl Pts',(40.5666590139515,29.3885761362401,18.6995531509269));
#27816=CARTESIAN_POINT('Ctrl Pts',(40.7333430451841,29.2440888804717,18.6161333949145));
#27817=CARTESIAN_POINT('Ctrl Pts',(40.9,29.0996231131986,18.5327260452907));
#27818=CARTESIAN_POINT('',(40.9,30.5996231131986,15.9346498339374));
#27819=CARTESIAN_POINT('Origin',(40.9,0.,0.));
#27820=CARTESIAN_POINT('',(40.4,31.0330398077868,16.1848830792292));
#27821=CARTESIAN_POINT('Ctrl Pts',(40.9,30.5996231131986,15.9346498339374));
#27822=CARTESIAN_POINT('Ctrl Pts',(40.7333430442943,30.744088881243,16.0180571840065));
#27823=CARTESIAN_POINT('Ctrl Pts',(40.5666590123842,30.8885761375987,16.101476940358));
#27824=CARTESIAN_POINT('Ctrl Pts',(40.4,31.0330398077868,16.1848830792292));
#27825=CARTESIAN_POINT('Origin',(40.4,0.,0.));
#27826=CARTESIAN_POINT('Origin',(35.7,0.,0.));
#27827=CARTESIAN_POINT('',(30.5,31.0562879796886,16.1402285275843));
#27828=CARTESIAN_POINT('Ctrl Pts',(40.3999012894849,31.0330346270951,16.1848928782182));
#27829=CARTESIAN_POINT('Ctrl Pts',(39.2494626810401,31.0330116996609,16.1849362443212));
#27830=CARTESIAN_POINT('Ctrl Pts',(38.0976708836828,31.0329190263647,16.1851115327779));
#27831=CARTESIAN_POINT('Ctrl Pts',(36.9467340384723,31.0328856894588,16.1851746119074));
#27832=CARTESIAN_POINT('Ctrl Pts',(36.745427730736,31.032879858618,16.1851856448557));
#27833=CARTESIAN_POINT('Ctrl Pts',(36.5441475779313,31.0328758430124,16.1851932450653));
#27834=CARTESIAN_POINT('Ctrl Pts',(36.3429119519248,31.0328722727086,16.1852000001162));
#27835=CARTESIAN_POINT('Ctrl Pts',(36.2102758775794,31.0328699194916,16.1852044524265));
#27836=CARTESIAN_POINT('Ctrl Pts',(36.0822774296293,31.0328678560427,16.1852084224022));
#27837=CARTESIAN_POINT('Ctrl Pts',(35.9587202262686,31.0328657167445,16.1852125810274));
#27838=CARTESIAN_POINT('Ctrl Pts',(35.7925662245335,31.0328628399153,16.1852181733537));
#27839=CARTESIAN_POINT('Ctrl Pts',(35.6344388155487,31.0328598211429,16.1852241162452));
#27840=CARTESIAN_POINT('Ctrl Pts',(35.4837714463449,31.032856216152,16.1852312078526));
#27841=CARTESIAN_POINT('Ctrl Pts',(35.3175474553595,31.0328522389406,16.1852390316786));
#27842=CARTESIAN_POINT('Ctrl Pts',(35.1604041224851,31.0328475520712,16.1852482463284));
#27843=CARTESIAN_POINT('Ctrl Pts',(35.011642794874,31.0328419178902,16.1852592402397));
#27844=CARTESIAN_POINT('Ctrl Pts',(34.9979272091186,31.0328413984266,16.1852602538629));
#27845=CARTESIAN_POINT('Ctrl Pts',(34.9842829110392,31.0328408711132,16.1852612822246));
#27846=CARTESIAN_POINT('Ctrl Pts',(34.9707093736272,31.0328403358797,16.1852623254084));
#27847=CARTESIAN_POINT('Ctrl Pts',(34.8522491799023,31.0328356647415,16.1852714295754));
#27848=CARTESIAN_POINT('Ctrl Pts',(34.7391835006529,31.0328304196803,16.1852816068676));
#27849=CARTESIAN_POINT('Ctrl Pts',(34.6312849042887,31.0328252639047,16.1852915612823));
#27850=CARTESIAN_POINT('Ctrl Pts',(34.5096795260851,31.0328194531708,16.1853027802453));
#27851=CARTESIAN_POINT('Ctrl Pts',(34.3946370581326,31.0328137541413,16.1853137193614));
#27852=CARTESIAN_POINT('Ctrl Pts',(34.2857585821188,31.0328086821746,16.1853233495613));
#27853=CARTESIAN_POINT('Ctrl Pts',(34.1786801908151,31.0328036940625,16.1853328205454));
#27854=CARTESIAN_POINT('Ctrl Pts',(34.0775620514827,31.0327993031901,16.185341043166));
#27855=CARTESIAN_POINT('Ctrl Pts',(33.9819758246427,31.0327957057952,16.1853475980775));
#27856=CARTESIAN_POINT('Ctrl Pts',(33.9184449689727,31.0327933148067,16.1853519547631));
#27857=CARTESIAN_POINT('Ctrl Pts',(33.8573517602305,31.0327912624254,16.1853555977387));
#27858=CARTESIAN_POINT('Ctrl Pts',(33.7984399511826,31.0327894081824,16.1853587887284));
#27859=CARTESIAN_POINT('Ctrl Pts',(33.7337970612213,31.0327873735543,16.1853622901453));
#27860=CARTESIAN_POINT('Ctrl Pts',(33.6717809742681,31.0327855776264,16.1853652470742));
#27861=CARTESIAN_POINT('Ctrl Pts',(33.6121191806454,31.0327838881567,16.1853678991828));
#27862=CARTESIAN_POINT('Ctrl Pts',(33.5695978710648,31.0327826840617,16.1853697893561));
#27863=CARTESIAN_POINT('Ctrl Pts',(33.5282738752657,31.0327815352149,16.185371522363));
#27864=CARTESIAN_POINT('Ctrl Pts',(33.4880643388298,31.032780407062,16.1853731585247));
#27865=CARTESIAN_POINT('Ctrl Pts',(33.4508270573206,31.0327793623013,16.1853746737428));
#27866=CARTESIAN_POINT('Ctrl Pts',(33.4145509216558,31.0327783314862,16.1853761126592));
#27867=CARTESIAN_POINT('Ctrl Pts',(33.3793439789548,31.0327771639657,16.1853777420673));
#27868=CARTESIAN_POINT('Ctrl Pts',(33.3411337035362,31.0327758968498,16.1853795104722));
#27869=CARTESIAN_POINT('Ctrl Pts',(33.3041826660689,31.0327744688781,16.1853815029502));
#27870=CARTESIAN_POINT('Ctrl Pts',(33.2685652776782,31.0327727495066,16.1853839484229));
#27871=CARTESIAN_POINT('Ctrl Pts',(33.231009447455,31.0327709365599,16.1853865269881));
#27872=CARTESIAN_POINT('Ctrl Pts',(33.1949357943681,31.0327688002292,16.185389608116));
#27873=CARTESIAN_POINT('Ctrl Pts',(33.1603699172393,31.0327662471215,16.1853933524012));
#27874=CARTESIAN_POINT('Ctrl Pts',(33.1223715679418,31.0327634404841,16.1853974685027));
#27875=CARTESIAN_POINT('Ctrl Pts',(33.0861949166475,31.0327601306123,16.1854023852333));
#27876=CARTESIAN_POINT('Ctrl Pts',(33.0518089354073,31.0327562557942,16.1854082033113));
#27877=CARTESIAN_POINT('Ctrl Pts',(33.0341030813059,31.0327542605926,16.1854111991264));
#27878=CARTESIAN_POINT('Ctrl Pts',(33.0168710360021,31.032752116523,16.1854144322605));
#27879=CARTESIAN_POINT('Ctrl Pts',(33.0001033802535,31.0327498200704,16.1854179076007));
#27880=CARTESIAN_POINT('Ctrl Pts',(32.9420348133412,31.0327418671573,16.1854299431544));
#27881=CARTESIAN_POINT('Ctrl Pts',(32.8874145324497,31.0328461364757,16.1852296143114));
#27882=CARTESIAN_POINT('Ctrl Pts',(32.8357863520582,31.0330149777623,16.1849068811705));
#27883=CARTESIAN_POINT('Ctrl Pts',(32.7779739682632,31.0332040434467,16.1845454899291));
#27884=CARTESIAN_POINT('Ctrl Pts',(32.7239136589685,31.0334742654593,16.1840302574575));
#27885=CARTESIAN_POINT('Ctrl Pts',(32.6729278684755,31.033785409572,16.1834371021678));
#27886=CARTESIAN_POINT('Ctrl Pts',(32.6180801336262,31.0341201214522,16.1827990180322));
#27887=CARTESIAN_POINT('Ctrl Pts',(32.5667902508433,31.0345025939175,16.1820699950122));
#27888=CARTESIAN_POINT('Ctrl Pts',(32.5181731636799,31.034906696383,16.1812992842338));
#27889=CARTESIAN_POINT('Ctrl Pts',(32.4659536029869,31.0353407424038,16.1804714646211));
#27890=CARTESIAN_POINT('Ctrl Pts',(32.416817513625,31.0358001425894,16.1795947944396));
#27891=CARTESIAN_POINT('Ctrl Pts',(32.3696233879015,31.0362725138779,16.1786925325962));
#27892=CARTESIAN_POINT('Ctrl Pts',(32.3182581618433,31.0367866341767,16.1777105272546));
#27893=CARTESIAN_POINT('Ctrl Pts',(32.2691934412649,31.0373164741888,16.1766975364929));
#27894=CARTESIAN_POINT('Ctrl Pts',(32.2209064724825,31.0378627004433,16.1756521425246));
#27895=CARTESIAN_POINT('Ctrl Pts',(32.1715370438648,31.0384211715746,16.1745833137248));
#27896=CARTESIAN_POINT('Ctrl Pts',(32.1229805798605,31.0389971805319,16.1734798401021));
#27897=CARTESIAN_POINT('Ctrl Pts',(32.0735591134784,31.039601856364,16.1723205501867));
#27898=CARTESIAN_POINT('Ctrl Pts',(32.0254239419648,31.0401907942692,16.1711914331653));
#27899=CARTESIAN_POINT('Ctrl Pts',(31.976468287942,31.04080728099,16.1700086968177));
#27900=CARTESIAN_POINT('Ctrl Pts',(31.9250947921535,31.041465759884,16.1687449477339));
#27901=CARTESIAN_POINT('Ctrl Pts',(31.8952919104891,31.0418477578044,16.1680118194191));
#27902=CARTESIAN_POINT('Ctrl Pts',(31.8646744620485,31.0422439429541,16.1672513233696));
#27903=CARTESIAN_POINT('Ctrl Pts',(31.8329224323944,31.0426570718779,16.1664582369103));
#27904=CARTESIAN_POINT('Ctrl Pts',(31.7319354368356,31.0439710240642,16.1639358337881));
#27905=CARTESIAN_POINT('Ctrl Pts',(31.6284526822057,31.0453389332579,16.1613063818566));
#27906=CARTESIAN_POINT('Ctrl Pts',(31.5232336354319,31.0466795487252,16.1587277943726));
#27907=CARTESIAN_POINT('Ctrl Pts',(31.418880786625,31.0480091278028,16.156170434673));
#27908=CARTESIAN_POINT('Ctrl Pts',(31.3128198672023,31.0493111005243,16.1536645426213));
#27909=CARTESIAN_POINT('Ctrl Pts',(31.2058402970406,31.0505011542277,16.1513736799427));
#27910=CARTESIAN_POINT('Ctrl Pts',(31.1464339374051,31.0511619977718,16.1501015509562));
#27911=CARTESIAN_POINT('Ctrl Pts',(31.0867451889514,31.051788304276,16.1488957763821));
#27912=CARTESIAN_POINT('Ctrl Pts',(31.0269161235859,31.052366291213,16.1477831210734));
#27913=CARTESIAN_POINT('Ctrl Pts',(30.9223727403119,31.0533762469848,16.1458389029967));
#27914=CARTESIAN_POINT('Ctrl Pts',(30.8173993541569,31.0542375463396,16.1441811147896));
#27915=CARTESIAN_POINT('Ctrl Pts',(30.7129204018003,31.0548748925162,16.1429541726495));
#27916=CARTESIAN_POINT('Ctrl Pts',(30.6397146645874,31.0553214647269,16.1420944855847));
#27917=CARTESIAN_POINT('Ctrl Pts',(30.5667525557982,31.0556583368409,16.1414458510595));
#27918=CARTESIAN_POINT('Ctrl Pts',(30.4943593393942,31.0558660149161,16.1410459118957));
#27919=CARTESIAN_POINT('',(30.5,29.559989655385,18.7405179110273));
#27920=CARTESIAN_POINT('Origin',(30.5,0.,0.));
#27921=CARTESIAN_POINT('Ctrl Pts',(30.5049791805002,29.5605178050972,18.7395177484757));
#27922=CARTESIAN_POINT('Ctrl Pts',(30.5973676827742,29.5601622646428,18.7400797009802));
#27923=CARTESIAN_POINT('Ctrl Pts',(30.6891105694844,29.5595425101548,18.7410567560112));
#27924=CARTESIAN_POINT('Ctrl Pts',(30.7806774793078,29.5587264396734,18.7423441244047));
#27925=CARTESIAN_POINT('Ctrl Pts',(30.8441888930627,29.5581604077946,18.7432370516297));
#27926=CARTESIAN_POINT('Ctrl Pts',(30.9076166453415,29.5574994222391,18.7442800408075));
#27927=CARTESIAN_POINT('Ctrl Pts',(30.9711288096738,29.5567612578199,18.745445599991));
#27928=CARTESIAN_POINT('Ctrl Pts',(31.0735567068109,29.5555707987954,18.7473253308647));
#27929=CARTESIAN_POINT('Ctrl Pts',(31.1762019082913,29.5541800414697,18.749523155664));
#27930=CARTESIAN_POINT('Ctrl Pts',(31.2798872709468,29.5526737444514,18.7519033574721));
#27931=CARTESIAN_POINT('Ctrl Pts',(31.3828989348253,29.5511772346434,18.7542680938471));
#27932=CARTESIAN_POINT('Ctrl Pts',(31.4869372222095,29.5495656759357,18.7568144117909));
#27933=CARTESIAN_POINT('Ctrl Pts',(31.5928574097401,29.5479181178243,18.7594156373082));
#27934=CARTESIAN_POINT('Ctrl Pts',(31.6516459294275,29.5470036792765,18.7608593866171));
#27935=CARTESIAN_POINT('Ctrl Pts',(31.71101503912,29.5460781618906,18.762320034785));
#27936=CARTESIAN_POINT('Ctrl Pts',(31.7711176725242,29.5451562912554,18.7637740491309));
#27937=CARTESIAN_POINT('Ctrl Pts',(31.8409082760364,29.5440858238841,18.7654624366935));
#27938=CARTESIAN_POINT('Ctrl Pts',(31.9056373311746,29.5431152615714,18.766993363124));
#27939=CARTESIAN_POINT('Ctrl Pts',(31.9658882086281,29.5422441375118,18.768367583494));
#27940=CARTESIAN_POINT('Ctrl Pts',(32.0341093482754,29.5412577771693,18.7699235920324));
#27941=CARTESIAN_POINT('Ctrl Pts',(32.0965888127921,29.5403982847665,18.7712796560442));
#27942=CARTESIAN_POINT('Ctrl Pts',(32.1542362617659,29.5396480149484,18.7724634074922));
#27943=CARTESIAN_POINT('Ctrl Pts',(32.2151538519828,29.5388551849074,18.773714309083));
#27944=CARTESIAN_POINT('Ctrl Pts',(32.2706761902186,29.5381836213573,18.7747738843964));
#27945=CARTESIAN_POINT('Ctrl Pts',(32.3219402247756,29.5376060245817,18.7756849339008));
#27946=CARTESIAN_POINT('Ctrl Pts',(32.3761674213252,29.5369950415769,18.7766486438579));
#27947=CARTESIAN_POINT('Ctrl Pts',(32.4256304058852,29.5364887148647,18.7774469218491));
#27948=CARTESIAN_POINT('Ctrl Pts',(32.4717350314086,29.5360572749796,18.7781265619113));
#27949=CARTESIAN_POINT('Ctrl Pts',(32.5214923281269,29.535591653968,18.7788600469326));
#27950=CARTESIAN_POINT('Ctrl Pts',(32.5673384642538,29.5352128774492,18.7794559410666));
#27951=CARTESIAN_POINT('Ctrl Pts',(32.6111004962939,29.5348934788927,18.7799576530151));
#27952=CARTESIAN_POINT('Ctrl Pts',(32.6551147163185,29.5345722397343,18.780462256185));
#27953=CARTESIAN_POINT('Ctrl Pts',(32.6970214084873,29.5343108907557,18.7808718608788));
#27954=CARTESIAN_POINT('Ctrl Pts',(32.7387279964579,29.5340950825231,18.7812095285094));
#27955=CARTESIAN_POINT('Ctrl Pts',(32.7800761354879,29.533881129063,18.781544294042));
#27956=CARTESIAN_POINT('Ctrl Pts',(32.8212277342352,29.5337116838823,18.7818087481602));
#27957=CARTESIAN_POINT('Ctrl Pts',(32.8640829337527,29.5335890251803,18.782000095504));
#27958=CARTESIAN_POINT('Ctrl Pts',(32.9037320332527,29.5334755428694,18.7821771276951));
#27959=CARTESIAN_POINT('Ctrl Pts',(32.9448394203909,29.5334018918636,18.782291920091));
#27960=CARTESIAN_POINT('Ctrl Pts',(32.9889438598236,29.5333868654405,18.7823158450367));
#27961=CARTESIAN_POINT('Ctrl Pts',(32.9925102269246,29.533385650376,18.7823177796523));
#27962=CARTESIAN_POINT('Ctrl Pts',(32.9960962106235,29.5333848297967,18.7823191027632));
#27963=CARTESIAN_POINT('Ctrl Pts',(32.9997026353888,29.5333844198653,18.7823197895505));
#27964=CARTESIAN_POINT('Ctrl Pts',(33.0361388185045,29.5333802782742,18.7823267282529));
#27965=CARTESIAN_POINT('Ctrl Pts',(33.0740002606604,29.5333765562528,18.7823330770045));
#27966=CARTESIAN_POINT('Ctrl Pts',(33.1140504028667,29.5333733966325,18.7823389179975));
#27967=CARTESIAN_POINT('Ctrl Pts',(33.2460690464807,29.5333629814689,18.7823581718611));
#27968=CARTESIAN_POINT('Ctrl Pts',(33.3720922029406,29.5333587011923,18.7823661897829));
#27969=CARTESIAN_POINT('Ctrl Pts',(33.4992849360725,29.5333546566755,18.7823737360729));
#27970=CARTESIAN_POINT('Ctrl Pts',(33.6626792864137,29.5333494610078,18.7823834301893));
#27971=CARTESIAN_POINT('Ctrl Pts',(33.8280037294636,29.5333446544025,18.7823923459959));
#27972=CARTESIAN_POINT('Ctrl Pts',(33.9928746198634,29.5333373313072,18.7824059536077));
#27973=CARTESIAN_POINT('Ctrl Pts',(34.322616400663,29.5333226851164,18.7824331688313));
#27974=CARTESIAN_POINT('Ctrl Pts',(34.650543970862,29.5332979729651,18.7824791512758));
#27975=CARTESIAN_POINT('Ctrl Pts',(34.979144925286,29.5332814027048,18.7825099763789));
#27976=CARTESIAN_POINT('Ctrl Pts',(35.30774587971,29.5332648324445,18.782540801482));
#27977=CARTESIAN_POINT('Ctrl Pts',(35.6370202183589,29.5332564040751,18.7825564692435));
#27978=CARTESIAN_POINT('Ctrl Pts',(35.9661418060973,29.5332492722834,18.7825697306317));
#27979=CARTESIAN_POINT('Ctrl Pts',(36.2952633938357,29.5332421404917,18.7825829920199));
#27980=CARTESIAN_POINT('Ctrl Pts',(36.6242322306637,29.5332363052776,18.7825938470347));
#27981=CARTESIAN_POINT('Ctrl Pts',(36.9531363303404,29.533224710841,18.782615411986));
#27982=CARTESIAN_POINT('Ctrl Pts',(38.1022190076918,29.5331842036954,18.7826907528288));
#27983=CARTESIAN_POINT('Ctrl Pts',(39.2505115204485,29.5330734009978,18.782896816333));
#27984=CARTESIAN_POINT('Ctrl Pts',(40.400093943525,29.533045998731,18.7829477771169));
#27985=CARTESIAN_POINT('Ctrl Pts',(6.89999999997365,5.3678954269134,9.63452070648359));
#27986=CARTESIAN_POINT('Ctrl Pts',(6.99168932310453,5.42175501956,9.60499723839754));
#27987=CARTESIAN_POINT('Ctrl Pts',(7.08383915760479,5.47527828673705,9.57508016834563));
#27988=CARTESIAN_POINT('Ctrl Pts',(8.15762752947027,6.09209251732962,9.22342495405908));
#27989=CARTESIAN_POINT('Ctrl Pts',(9.16608342448599,6.61836595106258,8.84591675027099));
#27990=CARTESIAN_POINT('Ctrl Pts',(11.2535425311854,7.53037930120419,8.09542754093137));
#27991=CARTESIAN_POINT('Ctrl Pts',(12.2577133097064,7.91666449612081,7.70725001371761));
#27992=CARTESIAN_POINT('Ctrl Pts',(14.356433377742,8.58141250110813,6.97440810645327));
#27993=CARTESIAN_POINT('Ctrl Pts',(15.3659105035251,8.85322312286061,6.61345583116597));
#27994=CARTESIAN_POINT('Ctrl Pts',(17.4728641219044,9.31281879192962,5.96623757129008));
#27995=CARTESIAN_POINT('Ctrl Pts',(18.4890996814195,9.49384943617778,5.66020885204394));
#27996=CARTESIAN_POINT('Ctrl Pts',(19.8476172011441,9.68599953593307,5.32865724601649));
#27997=CARTESIAN_POINT('Ctrl Pts',(20.3454889307686,9.75195458239818,5.2093054291626));
#27998=CARTESIAN_POINT('Ctrl Pts',(21.3782040612024,9.87366876552718,4.97678151322347));
#27999=CARTESIAN_POINT('Ctrl Pts',(22.1792648896895,9.95072592994714,4.81935607344487));
#28000=CARTESIAN_POINT('Ctrl Pts',(22.8542621828909,10.0067883222623,4.70591921690555));
#28001=CARTESIAN_POINT('Ctrl Pts',(23.1054579010968,10.0267605301623,4.66456206383029));
#28002=CARTESIAN_POINT('Ctrl Pts',(23.6171513959785,10.0644076466806,4.58448144656259));
#28003=CARTESIAN_POINT('Ctrl Pts',(24.1360713221937,10.0979855598765,4.51012725444835));
#28004=CARTESIAN_POINT('Ctrl Pts',(24.6624927871864,10.1277002159266,4.44285620865166));
#28005=CARTESIAN_POINT('Ctrl Pts',(25.1928168818088,10.154786256444,4.38095271718121));
#28006=CARTESIAN_POINT('Ctrl Pts',(25.5948982287615,10.1721457030179,4.34117176259644));
#28007=CARTESIAN_POINT('Ctrl Pts',(26.1232031889651,10.1922876384417,4.29604941535507));
#28008=CARTESIAN_POINT('Ctrl Pts',(27.1768897027567,10.2241871753182,4.22326129112041));
#28009=CARTESIAN_POINT('Ctrl Pts',(28.2111297865347,10.2325109692973,4.19969555688314));
#28010=CARTESIAN_POINT('Ctrl Pts',(29.1277555719713,10.2421056253618,4.17661492679514));
#28011=CARTESIAN_POINT('Ctrl Pts',(29.4767605677587,10.2448788784735,4.1700561490002));
#28012=CARTESIAN_POINT('Ctrl Pts',(30.1601418995912,10.2473221772452,4.16421367130872));
#28013=CARTESIAN_POINT('Ctrl Pts',(31.3500242312262,10.2457563290907,4.16794387579264));
#28014=CARTESIAN_POINT('Ctrl Pts',(32.3461596131128,10.2405791191157,4.18040640609127));
#28015=CARTESIAN_POINT('Ctrl Pts',(33.1614718826738,10.2405840900447,4.18039330945985));
#28016=CARTESIAN_POINT('Ctrl Pts',(33.4925794155279,10.2405841444578,4.18039253080268));
#28017=CARTESIAN_POINT('Ctrl Pts',(34.1499904318886,10.2405848392549,4.18039030822715));
#28018=CARTESIAN_POINT('Ctrl Pts',(34.9738731541179,10.2405865289644,4.18038393925505));
#28019=CARTESIAN_POINT('Ctrl Pts',(35.9612754428242,10.2405873001735,4.18038119412749));
#28020=CARTESIAN_POINT('Ctrl Pts',(37.936646788162,10.2405882857915,4.18037753677864));
#28021=CARTESIAN_POINT('Ctrl Pts',(39.5833333333333,10.2405934798255,4.18035859466987));
#28022=CARTESIAN_POINT('Ctrl Pts',(40.9,10.2405934798255,4.18035859466987));
#28023=CARTESIAN_POINT('Ctrl Pts',(6.71972576838711,6.5764381714634,12.8464244365415));
#28024=CARTESIAN_POINT('Ctrl Pts',(6.81144220747046,6.6482837686261,12.8102053989753));
#28025=CARTESIAN_POINT('Ctrl Pts',(6.90362823998598,6.71971524922859,12.7734498343709));
#28026=CARTESIAN_POINT('Ctrl Pts',(7.97787811486329,7.54294881554193,12.3410744046091));
#28027=CARTESIAN_POINT('Ctrl Pts',(8.98681832185142,8.24809748747637,11.871220138602));
#28028=CARTESIAN_POINT('Ctrl Pts',(11.0806583453373,9.47774891389534,10.9274240314556));
#28029=CARTESIAN_POINT('Ctrl Pts',(12.0862475175457,10.0005505115845,10.4368998098018));
#28030=CARTESIAN_POINT('Ctrl Pts',(14.197639322261,10.906656993414,9.50280276487818));
#28031=CARTESIAN_POINT('Ctrl Pts',(15.2100862637122,11.2785931828498,9.0420363325472));
#28032=CARTESIAN_POINT('Ctrl Pts',(17.3364698493954,11.9121957711898,8.20932952666153));
#28033=CARTESIAN_POINT('Ctrl Pts',(18.357279581038,12.1627870018009,7.81594677169139));
#28034=CARTESIAN_POINT('Ctrl Pts',(19.7331217809845,12.4307568384137,7.38628119283516));
#28035=CARTESIAN_POINT('Ctrl Pts',(20.2341927100358,12.5225360922774,7.23233618870704));
#28036=CARTESIAN_POINT('Ctrl Pts',(21.2777139275316,12.6928916013278,6.93114017240205));
#28037=CARTESIAN_POINT('Ctrl Pts',(22.0885637816418,12.8012350092453,6.72673758680647));
#28038=CARTESIAN_POINT('Ctrl Pts',(22.7734874647764,12.8801738355232,6.57909772915772));
#28039=CARTESIAN_POINT('Ctrl Pts',(23.0269571312139,12.9082278965574,6.52549682636868));
#28040=CARTESIAN_POINT('Ctrl Pts',(23.5444618566097,12.9612738268023,6.42148511325403));
#28041=CARTESIAN_POINT('Ctrl Pts',(24.0694383156461,13.0087020921734,6.32485290039694));
#28042=CARTESIAN_POINT('Ctrl Pts',(24.6027295908464,13.0507741241225,6.23730008137711));
#28043=CARTESIAN_POINT('Ctrl Pts',(25.1403192523141,13.0891677302172,6.15667530541499));
#28044=CARTESIAN_POINT('Ctrl Pts',(25.5484689870706,13.1137995888261,6.10479659087691));
#28045=CARTESIAN_POINT('Ctrl Pts',(26.0852808149067,13.1423647911197,6.04589855121055));
#28046=CARTESIAN_POINT('Ctrl Pts',(27.1586857291269,13.1877077660314,5.95074158602808));
#28047=CARTESIAN_POINT('Ctrl Pts',(28.1995312980844,13.1995114624862,5.92039197700573));
#28048=CARTESIAN_POINT('Ctrl Pts',(29.1157533315888,13.2130297822556,5.89061060808306));
#28049=CARTESIAN_POINT('Ctrl Pts',(29.4698938670486,13.2169740538762,5.88204921070823));
#28050=CARTESIAN_POINT('Ctrl Pts',(30.1587234046998,13.220429005539,5.8744768355958));
#28051=CARTESIAN_POINT('Ctrl Pts',(31.355731195606,13.2182120926509,5.87931523414859));
#28052=CARTESIAN_POINT('Ctrl Pts',(32.350180243561,13.2109234983782,5.89537176970751));
#28053=CARTESIAN_POINT('Ctrl Pts',(33.1605031382466,13.2109314016452,5.89535013085609));
#28054=CARTESIAN_POINT('Ctrl Pts',(33.4922179295252,13.2109314596682,5.89534881762645));
#28055=CARTESIAN_POINT('Ctrl Pts',(34.1493400019899,13.2109325467447,5.89534512891168));
#28056=CARTESIAN_POINT('Ctrl Pts',(34.9735241318652,13.2109351472382,5.8953345252407));
#28057=CARTESIAN_POINT('Ctrl Pts',(35.9608954520827,13.2109363413972,5.89532995964262));
#28058=CARTESIAN_POINT('Ctrl Pts',(37.9363824842976,13.2109378608691,5.8953238722353));
#28059=CARTESIAN_POINT('Ctrl Pts',(39.5833333333333,13.2109458830841,5.89529235427929));
#28060=CARTESIAN_POINT('Ctrl Pts',(40.9,13.2109458830841,5.89529235427929));
#28061=CARTESIAN_POINT('Ctrl Pts',(6.48177011792015,9.40621265917915,20.336764848396));
#28062=CARTESIAN_POINT('Ctrl Pts',(6.57271435585529,9.51911083717171,20.2851799357091));
#28063=CARTESIAN_POINT('Ctrl Pts',(6.66411141569866,9.63139437446865,20.2327517601296));
#28064=CARTESIAN_POINT('Ctrl Pts',(7.73048017258431,10.9276768808967,19.614616528956));
#28065=CARTESIAN_POINT('Ctrl Pts',(8.73292722985418,12.0456324995184,18.9319609573801));
#28066=CARTESIAN_POINT('Ctrl Pts',(10.8102906905198,14.0013807284478,17.5485371602851));
#28067=CARTESIAN_POINT('Ctrl Pts',(11.8125687231201,14.8418955382559,16.8218444562665));
#28068=CARTESIAN_POINT('Ctrl Pts',(13.9177445864075,16.3050153868123,15.4271303717406));
#28069=CARTESIAN_POINT('Ctrl Pts',(14.9296562678442,16.9116612373854,14.7350649820735));
#28070=CARTESIAN_POINT('Ctrl Pts',(17.0680844879216,17.9535844659564,13.4708635112562));
#28071=CARTESIAN_POINT('Ctrl Pts',(18.0932339179161,18.3688941094638,12.8729609429));
#28072=CARTESIAN_POINT('Ctrl Pts',(19.4933464326809,18.8183285494774,12.2099892645604));
#28073=CARTESIAN_POINT('Ctrl Pts',(19.9993272808496,18.971430097181,11.9744841299437));
#28074=CARTESIAN_POINT('Ctrl Pts',(21.0600020168761,19.2581324129063,11.5100300116438));
#28075=CARTESIAN_POINT('Ctrl Pts',(21.8888875769483,19.4420158954032,11.1928649299996));
#28076=CARTESIAN_POINT('Ctrl Pts',(22.5933490549503,19.5764520117208,10.962505511385));
#28077=CARTESIAN_POINT('Ctrl Pts',(22.8513437851799,19.6238525927722,10.8796937171906));
#28078=CARTESIAN_POINT('Ctrl Pts',(23.3805933886566,19.7139851739534,10.7182299385361));
#28079=CARTESIAN_POINT('Ctrl Pts',(23.9182257576785,19.7948254980796,10.5680285062335));
#28080=CARTESIAN_POINT('Ctrl Pts',(24.4662138806868,19.8668205194741,10.4315004891655));
#28081=CARTESIAN_POINT('Ctrl Pts',(25.0195744741822,19.9326328666884,10.3055778221167));
#28082=CARTESIAN_POINT('Ctrl Pts',(25.4412458088222,19.9749776253082,10.2242864909386));
#28083=CARTESIAN_POINT('Ctrl Pts',(25.9971983460992,20.0240850656221,10.131797107587));
#28084=CARTESIAN_POINT('Ctrl Pts',(27.1157050405652,20.102368552767,9.98182332250462));
#28085=CARTESIAN_POINT('Ctrl Pts',(28.1723100127449,20.1222437541335,9.93573708068025));
#28086=CARTESIAN_POINT('Ctrl Pts',(29.0876106506766,20.1449463132817,9.89029022572785));
#28087=CARTESIAN_POINT('Ctrl Pts',(29.4537207931442,20.1517438988729,9.87684873205164));
#28088=CARTESIAN_POINT('Ctrl Pts',(30.1552759232946,20.1576060163182,9.86516345924738));
#28089=CARTESIAN_POINT('Ctrl Pts',(31.368924127636,20.1538463873917,9.87263514017793));
#28090=CARTESIAN_POINT('Ctrl Pts',(32.3594787154311,20.1416711708076,9.89702302165624));
#28091=CARTESIAN_POINT('Ctrl Pts',(33.1581760188914,20.1416983285705,9.89696607979067));
#28092=CARTESIAN_POINT('Ctrl Pts',(33.4913102145729,20.1416998058431,9.89696201382195));
#28093=CARTESIAN_POINT('Ctrl Pts',(34.1477617736107,20.1417043298969,9.89695193052414));
#28094=CARTESIAN_POINT('Ctrl Pts',(34.9726616332633,20.1417171222835,9.89692218573783));
#28095=CARTESIAN_POINT('Ctrl Pts',(35.9599657908142,20.1417226604566,9.89690948638393));
#28096=CARTESIAN_POINT('Ctrl Pts',(37.9357298104643,20.1417300151411,9.89689244880616));
#28097=CARTESIAN_POINT('Ctrl Pts',(39.5833333333333,20.1417681573542,9.89680446003461));
#28098=CARTESIAN_POINT('Ctrl Pts',(40.9,20.1417681573542,9.89680446003461));
#28099=CARTESIAN_POINT('Ctrl Pts',(6.40644620858992,12.3446157076951,27.7818319413302));
#28100=CARTESIAN_POINT('Ctrl Pts',(6.49686818484384,12.4976194141968,27.7146057723315));
#28101=CARTESIAN_POINT('Ctrl Pts',(6.58771883172007,12.6497754970257,27.6462615383487));
#28102=CARTESIAN_POINT('Ctrl Pts',(7.64885870107047,14.4089312086777,26.8389674658771));
#28103=CARTESIAN_POINT('Ctrl Pts',(8.64786699401839,15.9309901815184,25.9406999974138));
#28104=CARTESIAN_POINT('Ctrl Pts',(10.7071344443812,18.5841088194585,24.1258468463739));
#28105=CARTESIAN_POINT('Ctrl Pts',(11.7059636153277,19.7351568023896,23.1640388241121));
#28106=CARTESIAN_POINT('Ctrl Pts',(13.7894167134297,21.7274097031724,21.32755345859));
#28107=CARTESIAN_POINT('Ctrl Pts',(14.7964804448639,22.5625068415354,20.40896606215));
#28108=CARTESIAN_POINT('Ctrl Pts',(16.9150096963281,23.9923642448819,18.734786787185));
#28109=CARTESIAN_POINT('Ctrl Pts',(17.9356563974909,24.568778311437,17.9376031564435));
#28110=CARTESIAN_POINT('Ctrl Pts',(19.3316378726113,25.1942531765859,17.0495061236355));
#28111=CARTESIAN_POINT('Ctrl Pts',(19.8373783148988,25.4080883980548,16.733671277521));
#28112=CARTESIAN_POINT('Ctrl Pts',(20.8986146451321,25.8097110946141,16.1088561234904));
#28113=CARTESIAN_POINT('Ctrl Pts',(21.7322089233615,26.0695581056351,15.6790344990822));
#28114=CARTESIAN_POINT('Ctrl Pts',(22.4452152218927,26.2607608176432,15.3644450466695));
#28115=CARTESIAN_POINT('Ctrl Pts',(22.7053175952387,26.3278633535721,15.2520352575855));
#28116=CARTESIAN_POINT('Ctrl Pts',(23.2405350109147,26.4560495577169,15.0319031635372));
#28117=CARTESIAN_POINT('Ctrl Pts',(23.7856351879594,26.5714803865859,14.8265027181049));
#28118=CARTESIAN_POINT('Ctrl Pts',(24.3434088150882,26.6748081507042,14.6389049166987));
#28119=CARTESIAN_POINT('Ctrl Pts',(24.9080926446007,26.7695587595052,14.4653482504621));
#28120=CARTESIAN_POINT('Ctrl Pts',(25.3404979553364,26.8308622015487,14.3526452692475));
#28121=CARTESIAN_POINT('Ctrl Pts',(25.9125607075504,26.9021372597287,14.2239063651395));
#28122=CARTESIAN_POINT('Ctrl Pts',(27.0720378258712,27.0165941086124,14.0136986134135));
#28123=CARTESIAN_POINT('Ctrl Pts',(28.1454151442859,27.0445191043407,13.9518646781025));
#28124=CARTESIAN_POINT('Ctrl Pts',(29.0596751952944,27.0764264216485,13.890725520751));
#28125=CARTESIAN_POINT('Ctrl Pts',(29.4376599373188,27.0863532011149,13.8719255145712));
#28126=CARTESIAN_POINT('Ctrl Pts',(30.1519376760718,27.0947220176404,13.855954576287));
#28127=CARTESIAN_POINT('Ctrl Pts',(31.3821999577689,27.0893514143296,13.8661782937677));
#28128=CARTESIAN_POINT('Ctrl Pts',(32.3688386893657,27.0723527225427,13.8987881217581));
#28129=CARTESIAN_POINT('Ctrl Pts',(33.1558986739574,27.0724155351932,13.8986675947835));
#28130=CARTESIAN_POINT('Ctrl Pts',(33.49045038666,27.072419804706,13.8986584195583));
#28131=CARTESIAN_POINT('Ctrl Pts',(34.1462287076184,27.0724307945236,13.8986367255003));
#28132=CARTESIAN_POINT('Ctrl Pts',(34.9718350023128,27.0724629552156,13.8985720488061));
#28133=CARTESIAN_POINT('Ctrl Pts',(35.9590682028415,27.0724767217601,13.8985445297568));
#28134=CARTESIAN_POINT('Ctrl Pts',(37.9351039480424,27.072495155898,13.8985075170899));
#28135=CARTESIAN_POINT('Ctrl Pts',(39.5833333333333,27.0725904316243,13.8983165657899));
#28136=CARTESIAN_POINT('Ctrl Pts',(40.9,27.0725904316243,13.8983165657899));
#28137=CARTESIAN_POINT('Ctrl Pts',(6.37427268165564,14.0406695266741,32.0290848932163));
#28138=CARTESIAN_POINT('Ctrl Pts',(6.46448755772839,14.2166050753401,31.9528098065586));
#28139=CARTESIAN_POINT('Ctrl Pts',(6.55512327887566,14.3915605358513,31.8752581000468));
#28140=CARTESIAN_POINT('Ctrl Pts',(7.61410360785656,16.4151695040826,30.958672886913));
#28141=CARTESIAN_POINT('Ctrl Pts',(8.61142775869687,18.1677152487792,29.9361952854453));
#28142=CARTESIAN_POINT('Ctrl Pts',(10.6634825022472,21.2183968262284,27.8730682250753));
#28143=CARTESIAN_POINT('Ctrl Pts',(11.6607542873627,22.5462154536683,26.7761583709752));
#28144=CARTESIAN_POINT('Ctrl Pts',(13.7353039743977,24.8383185913233,24.6873364683673));
#28145=CARTESIAN_POINT('Ctrl Pts',(14.7402095633116,25.802985911944,23.6392130729629));
#28146=CARTESIAN_POINT('Ctrl Pts',(16.8490881066137,27.450307490631,21.733995182915));
#28147=CARTESIAN_POINT('Ctrl Pts',(17.8672038783315,28.117536242687,20.8239061433235));
#28148=CARTESIAN_POINT('Ctrl Pts',(19.2585933984997,28.8404836901117,19.811022849419));
#28149=CARTESIAN_POINT('Ctrl Pts',(19.7636418533908,29.0884650342026,19.4499572035579));
#28150=CARTESIAN_POINT('Ctrl Pts',(20.8231816497994,29.5540603372584,18.7357747989968));
#28151=CARTESIAN_POINT('Ctrl Pts',(21.6568670511735,29.8562628482713,18.2431916560479));
#28152=CARTESIAN_POINT('Ctrl Pts',(22.3720072062877,30.0792593376712,17.8815051531588));
#28153=CARTESIAN_POINT('Ctrl Pts',(22.6326824787813,30.1574913312728,17.7523977438431));
#28154=CARTESIAN_POINT('Ctrl Pts',(23.1697036949937,30.3071564102286,17.4991937768336));
#28155=CARTESIAN_POINT('Ctrl Pts',(23.7174377716562,30.4422233412819,17.2625030946595));
#28156=CARTESIAN_POINT('Ctrl Pts',(24.2790946262572,30.5634410393028,17.0457855087881));
#28157=CARTESIAN_POINT('Ctrl Pts',(24.8485847331463,30.6748008187179,16.8449230908939));
#28158=CARTESIAN_POINT('Ctrl Pts',(25.2859632686137,30.7471152582869,16.714000734413));
#28159=CARTESIAN_POINT('Ctrl Pts',(25.8659001690755,30.8313513860032,16.5640760155963));
#28160=CARTESIAN_POINT('Ctrl Pts',(27.0467877055032,30.9672841404844,16.3181083484215));
#28161=CARTESIAN_POINT('Ctrl Pts',(28.1301993946288,30.9999203594232,16.2470842981322));
#28162=CARTESIAN_POINT('Ctrl Pts',(29.0438132065911,31.0370949113971,16.1769735529556));
#28163=CARTESIAN_POINT('Ctrl Pts',(29.4285323170642,31.0489002942269,16.1549555741443));
#28164=CARTESIAN_POINT('Ctrl Pts',(30.1500796604944,31.0587367393328,16.1364761766636));
#28165=CARTESIAN_POINT('Ctrl Pts',(31.3898224001987,31.0524272220083,16.1483068856791));
#28166=CARTESIAN_POINT('Ctrl Pts',(32.3742147772173,31.0327017051641,16.1855693458549));
#28167=CARTESIAN_POINT('Ctrl Pts',(33.1546196294426,31.0327939306214,16.1853991323255));
#28168=CARTESIAN_POINT('Ctrl Pts',(33.4899805045662,31.0328008093452,16.185385634532));
#28169=CARTESIAN_POINT('Ctrl Pts',(34.1453728987309,31.0328173216774,16.1853546639146));
#28170=CARTESIAN_POINT('Ctrl Pts',(34.9713787068036,31.0328663827335,16.1852616946182));
#28171=CARTESIAN_POINT('Ctrl Pts',(35.9585696612047,31.0328872804502,16.1852222245757));
#28172=CARTESIAN_POINT('Ctrl Pts',(37.9347583211501,31.0329153648958,16.1851690519237));
#28173=CARTESIAN_POINT('Ctrl Pts',(39.5833333333333,31.0330603026358,16.1848949119358));
#28174=CARTESIAN_POINT('Ctrl Pts',(40.9,31.0330603026358,16.1848949119358));
#28175=CARTESIAN_POINT('',(40.9,29.2992994660114,15.1839076262003));
#28176=CARTESIAN_POINT('Ctrl Pts',(40.9,29.2992994660114,15.1839076262003));
#28177=CARTESIAN_POINT('Ctrl Pts',(40.9,29.7327406817405,15.4341550287793));
#28178=CARTESIAN_POINT('Ctrl Pts',(40.9,30.1661818974696,15.6844024313584));
#28179=CARTESIAN_POINT('Ctrl Pts',(40.9,30.5996231131986,15.9346498339374));
#28180=CARTESIAN_POINT('',(38.,29.2992994660114,15.1839076262003));
#28181=CARTESIAN_POINT('Ctrl Pts',(38.,29.2992994660114,15.1839076262003));
#28182=CARTESIAN_POINT('Ctrl Pts',(38.9666666666667,29.2992994660114,15.1839076262003));
#28183=CARTESIAN_POINT('Ctrl Pts',(39.9333333333333,29.2992994660114,15.1839076262003));
#28184=CARTESIAN_POINT('Ctrl Pts',(40.9,29.2992994660114,15.1839076262003));
#28185=CARTESIAN_POINT('Ctrl Pts',(37.4974382384971,28.7790269720418,14.8838038109906));
#28186=CARTESIAN_POINT('Ctrl Pts',(37.6645213547146,28.9527098777879,14.9840691120819));
#28187=CARTESIAN_POINT('Ctrl Pts',(37.8313739960416,29.1261374112004,15.084184715056));
#28188=CARTESIAN_POINT('Ctrl Pts',(37.9978889629903,29.2992044501375,15.1840905833949));
#28189=CARTESIAN_POINT('',(6.9,12.9951291628659,27.0393531365015));
#28190=CARTESIAN_POINT('Ctrl Pts',(6.9,12.9951291628659,27.0393531365015));
#28191=CARTESIAN_POINT('Ctrl Pts',(6.9,11.9174419758914,24.649274247254));
#28192=CARTESIAN_POINT('Ctrl Pts',(6.90000000000115,10.8339866674746,22.230729924082));
#28193=CARTESIAN_POINT('Ctrl Pts',(6.90000000000115,8.41000082059024,16.7584145047598));
#28194=CARTESIAN_POINT('Ctrl Pts',(6.9,6.82522008706163,13.1312177506378));
#28195=CARTESIAN_POINT('Ctrl Pts',(6.9,5.36789542693312,9.63452070648529));
#28196=CARTESIAN_POINT('',(22.9245129145126,27.5141512254856,15.8853026165582));
#28197=CARTESIAN_POINT('Ctrl Pts',(22.9245129145126,27.5141512254856,15.8853026165582));
#28198=CARTESIAN_POINT('Ctrl Pts',(22.7202811020963,27.405303612937,15.9355315703924));
#28199=CARTESIAN_POINT('Ctrl Pts',(22.5089075447093,27.2924652433825,15.9922246435191));
#28200=CARTESIAN_POINT('Ctrl Pts',(22.2913349439917,27.1762359097412,16.0558281873748));
#28201=CARTESIAN_POINT('Ctrl Pts',(21.4451770585293,26.7242103933933,16.3031876434794));
#28202=CARTESIAN_POINT('Ctrl Pts',(20.522095155667,26.2108400614943,16.6965145338605));
#28203=CARTESIAN_POINT('Ctrl Pts',(19.7671428819541,25.777085937268,17.0753616782143));
#28204=CARTESIAN_POINT('Ctrl Pts',(19.5194773058393,25.634790895834,17.1996442316059));
#28205=CARTESIAN_POINT('Ctrl Pts',(19.2865716386092,25.4994131575073,17.3225345039426));
#28206=CARTESIAN_POINT('Ctrl Pts',(19.0728538401323,25.3740784559106,17.4387046858284));
#28207=CARTESIAN_POINT('Ctrl Pts',(18.7028555998037,25.1570931632801,17.6398239336528));
#28208=CARTESIAN_POINT('Ctrl Pts',(18.4144703596238,24.9815167506413,17.8106758656204));
#28209=CARTESIAN_POINT('Ctrl Pts',(18.0642874871542,24.7606238748754,18.0298340093772));
#28210=CARTESIAN_POINT('Ctrl Pts',(17.4420927116724,24.3681478172276,18.4192278454838));
#28211=CARTESIAN_POINT('Ctrl Pts',(16.722456441822,23.8866996305776,18.9163953124274));
#28212=CARTESIAN_POINT('Ctrl Pts',(15.9202806616111,23.2999769887242,19.5075155171573));
#28213=CARTESIAN_POINT('Ctrl Pts',(15.4090529834523,22.9260578785773,19.8842371999004));
#28214=CARTESIAN_POINT('Ctrl Pts',(14.8739602945725,22.5035099772305,20.3065653819873));
#28215=CARTESIAN_POINT('Ctrl Pts',(14.3169794331172,22.0244589523056,20.7640450546171));
#28216=CARTESIAN_POINT('Ctrl Pts',(13.8864206762848,21.6541417151711,21.1176871503417));
#28217=CARTESIAN_POINT('Ctrl Pts',(13.3867890027812,21.2019814327451,21.5394320189419));
#28218=CARTESIAN_POINT('Ctrl Pts',(12.8146824059514,20.6456427149589,22.0238946695559));
#28219=CARTESIAN_POINT('Ctrl Pts',(12.2526665517595,20.0991166279862,22.499812430193));
#28220=CARTESIAN_POINT('Ctrl Pts',(11.6379478462803,19.44703563439,23.0419154065947));
#28221=CARTESIAN_POINT('Ctrl Pts',(10.9739250490308,18.6689137476991,23.6265354530559));
#28222=CARTESIAN_POINT('Ctrl Pts',(10.5683455447963,18.1936434853748,23.9836164291782));
#28223=CARTESIAN_POINT('Ctrl Pts',(10.1437415406956,17.6694303965612,24.3558958755273));
#28224=CARTESIAN_POINT('Ctrl Pts',(9.74137929176525,17.1528053766524,24.6998029803349));
#28225=CARTESIAN_POINT('Ctrl Pts',(8.72285779294234,15.8450442956717,25.5703537856744));
#28226=CARTESIAN_POINT('Ctrl Pts',(7.81323138778194,14.4751178145147,26.3485431508902));
#28227=CARTESIAN_POINT('Ctrl Pts',(6.9,12.9951291628659,27.0393531365015));
#28228=CARTESIAN_POINT('Ctrl Pts',(30.5,31.0562879796886,16.1402285275843));
#28229=CARTESIAN_POINT('Ctrl Pts',(29.9560179420817,30.8470467059701,16.0158030554221));
#28230=CARTESIAN_POINT('Ctrl Pts',(29.4152668325132,30.6299015220344,15.9055856438304));
#28231=CARTESIAN_POINT('Ctrl Pts',(28.8740459957565,30.3967092920472,15.8236145009996));
#28232=CARTESIAN_POINT('Ctrl Pts',(28.353527792344,30.1724370682909,15.7447788961961));
#28233=CARTESIAN_POINT('Ctrl Pts',(27.8179515912467,29.9423746730404,15.65999396651));
#28234=CARTESIAN_POINT('Ctrl Pts',(27.2695051149491,29.6962958928787,15.5981844167478));
#28235=CARTESIAN_POINT('Ctrl Pts',(26.9554553615883,29.5553870101399,15.5627912203338));
#28236=CARTESIAN_POINT('Ctrl Pts',(26.6378099296971,29.4095747645068,15.5350208970661));
#28237=CARTESIAN_POINT('Ctrl Pts',(26.3179304017917,29.2578762499931,15.520523503095));
#28238=CARTESIAN_POINT('Ctrl Pts',(26.1078196745982,29.1582340959378,15.5110009868852));
#28239=CARTESIAN_POINT('Ctrl Pts',(25.8967402232745,29.0560612282453,15.5072071790431));
#28240=CARTESIAN_POINT('Ctrl Pts',(25.6850706236774,28.9510881944939,15.5107635234098));
#28241=CARTESIAN_POINT('Ctrl Pts',(25.6562210027417,28.9367808388889,15.5112482372614));
#28242=CARTESIAN_POINT('Ctrl Pts',(25.6277737638215,28.9226278510966,15.5118582602788));
#28243=CARTESIAN_POINT('Ctrl Pts',(25.5983858063598,28.9079571471847,15.5126342200129));
#28244=CARTESIAN_POINT('Ctrl Pts',(25.1249357452756,28.6716070819486,15.5251351971226));
#28245=CARTESIAN_POINT('Ctrl Pts',(24.1510084067019,28.1678256190434,15.583657222894));
#28246=CARTESIAN_POINT('Ctrl Pts',(22.9245129145126,27.5141512254856,15.8853026165582));
#28247=CARTESIAN_POINT('Origin',(40.65,0.,0.));
#28248=CARTESIAN_POINT('',(40.4,16.1848830792292,31.0330398077868));
#28249=CARTESIAN_POINT('',(40.9,15.9346498339374,30.5996231131986));
#28250=CARTESIAN_POINT('Ctrl Pts',(40.4,16.1848830792292,31.0330398077868));
#28251=CARTESIAN_POINT('Ctrl Pts',(40.5666590127278,16.101476940186,30.8885761373009));
#28252=CARTESIAN_POINT('Ctrl Pts',(40.7333430445956,16.0180571838558,30.7440888809818));
#28253=CARTESIAN_POINT('Ctrl Pts',(40.9,15.9346498339374,30.5996231131986));
#28254=CARTESIAN_POINT('',(40.9,18.5327260452908,29.0996231131986));
#28255=CARTESIAN_POINT('Origin',(40.9,0.,0.));
#28256=CARTESIAN_POINT('',(40.4,18.7829592905825,29.5330398077868));
#28257=CARTESIAN_POINT('Ctrl Pts',(40.9,18.5327260452907,29.0996231131986));
#28258=CARTESIAN_POINT('Ctrl Pts',(40.7333430449886,18.6161333950124,29.2440888806411));
#28259=CARTESIAN_POINT('Ctrl Pts',(40.5666590138314,18.699553150987,29.3885761363442));
#28260=CARTESIAN_POINT('Ctrl Pts',(40.4,18.7829592905825,29.5330398077868));
#28261=CARTESIAN_POINT('Origin',(40.4,0.,0.));
#28262=CARTESIAN_POINT('Origin',(35.7,0.,0.));
#28263=CARTESIAN_POINT('',(30.5,18.8254200738635,29.5059919176187));
#28264=CARTESIAN_POINT('Ctrl Pts',(40.3998805977105,18.7829479019259,29.5330468723878));
#28265=CARTESIAN_POINT('Ctrl Pts',(39.2493532038275,18.7828975281295,29.5330781201994));
#28266=CARTESIAN_POINT('Ctrl Pts',(38.0972325173599,18.7826942098824,29.5332042421555));
#28267=CARTESIAN_POINT('Ctrl Pts',(36.9466403234098,18.782625610211,29.5332467931397));
#28268=CARTESIAN_POINT('Ctrl Pts',(36.745394297411,18.7826136116842,29.5332542355824));
#28269=CARTESIAN_POINT('Ctrl Pts',(36.5441950314761,18.7826057345052,29.5332591213989));
#28270=CARTESIAN_POINT('Ctrl Pts',(36.3429831482489,18.7825981392881,29.5332638326403));
#28271=CARTESIAN_POINT('Ctrl Pts',(36.2103627229667,18.7825931332173,29.5332669378586));
#28272=CARTESIAN_POINT('Ctrl Pts',(36.0823539051257,18.7825884046849,29.5332699079689));
#28273=CARTESIAN_POINT('Ctrl Pts',(35.9587472612939,18.782583031639,29.5332733040083));
#28274=CARTESIAN_POINT('Ctrl Pts',(35.7554552091559,18.7825741947555,29.5332788893702));
#28275=CARTESIAN_POINT('Ctrl Pts',(35.5640774639574,18.7825638026986,29.5332855100023));
#28276=CARTESIAN_POINT('Ctrl Pts',(35.3838244596789,18.7825536728019,29.5332919882553));
#28277=CARTESIAN_POINT('Ctrl Pts',(35.2391029657187,18.7825455397126,29.5332971895137));
#28278=CARTESIAN_POINT('Ctrl Pts',(35.1015509582107,18.7825375448577,29.5333023181014));
#28279=CARTESIAN_POINT('Ctrl Pts',(34.9707359993668,18.7825301857251,29.53330703978));
#28280=CARTESIAN_POINT('Ctrl Pts',(34.8578981782319,18.7825238379151,29.5333111125858));
#28281=CARTESIAN_POINT('Ctrl Pts',(34.7500670454682,18.7825179390022,29.5333148977088));
#28282=CARTESIAN_POINT('Ctrl Pts',(34.6468496336312,18.7825123391989,29.5333184739616));
#28283=CARTESIAN_POINT('Ctrl Pts',(34.5887227637979,18.7825091856706,29.5333204879278));
#28284=CARTESIAN_POINT('Ctrl Pts',(34.5320601650638,18.7825061280823,29.5333224349598));
#28285=CARTESIAN_POINT('Ctrl Pts',(34.4767987085459,18.7825031467929,29.5333243245742));
#28286=CARTESIAN_POINT('Ctrl Pts',(34.3959515551432,18.7824987851858,29.5333270890679));
#28287=CARTESIAN_POINT('Ctrl Pts',(34.3181086379449,18.7824945796072,29.533329735068));
#28288=CARTESIAN_POINT('Ctrl Pts',(34.2432236356779,18.7824903289018,29.5333323757534));
#28289=CARTESIAN_POINT('Ctrl Pts',(34.1622675304667,18.7824857335818,29.5333352305253));
#28290=CARTESIAN_POINT('Ctrl Pts',(34.0847679660317,18.7824810863437,29.5333380785848));
#28291=CARTESIAN_POINT('Ctrl Pts',(34.0106064145688,18.7824762391415,29.533340998409));
#28292=CARTESIAN_POINT('Ctrl Pts',(34.0011740964176,18.7824756226447,29.53334136977));
#28293=CARTESIAN_POINT('Ctrl Pts',(33.9917957065817,18.7824750030335,29.5333417422189));
#28294=CARTESIAN_POINT('Ctrl Pts',(33.9824709442606,18.7824743801028,29.5333421158564));
#28295=CARTESIAN_POINT('Ctrl Pts',(33.9223617768599,18.7824703645751,29.533344524394));
#28296=CARTESIAN_POINT('Ctrl Pts',(33.8644761964479,18.7824662176988,29.5333469783448));
#28297=CARTESIAN_POINT('Ctrl Pts',(33.8085662292048,18.7824621301166,29.5333493560321));
#28298=CARTESIAN_POINT('Ctrl Pts',(33.747423701629,18.7824576599816,29.533351956245));
#28299=CARTESIAN_POINT('Ctrl Pts',(33.6886441629997,18.782453260435,29.5333544654464));
#28300=CARTESIAN_POINT('Ctrl Pts',(33.6319696815839,18.7824490897764,29.5333567795391));
#28301=CARTESIAN_POINT('Ctrl Pts',(33.5826925637838,18.7824454634877,29.5333587915877));
#28302=CARTESIAN_POINT('Ctrl Pts',(33.535008342921,18.7824420082021,29.5333606573655));
#28303=CARTESIAN_POINT('Ctrl Pts',(33.4887791610839,18.7824387840041,29.5333623350385));
#28304=CARTESIAN_POINT('Ctrl Pts',(33.4518540160536,18.7824362087047,29.5333636750648));
#28305=CARTESIAN_POINT('Ctrl Pts',(33.4158630419527,18.7824337707087,29.5333649012377));
#28306=CARTESIAN_POINT('Ctrl Pts',(33.3809178974527,18.7824311830501,29.5333661853037));
#28307=CARTESIAN_POINT('Ctrl Pts',(33.3430135142413,18.7824283762623,29.5333675781075));
#28308=CARTESIAN_POINT('Ctrl Pts',(33.3063394414416,18.7824253936822,29.5333690388471));
#28309=CARTESIAN_POINT('Ctrl Pts',(33.2709744550635,18.7824219844966,29.5333707164935));
#28310=CARTESIAN_POINT('Ctrl Pts',(33.2337091834358,18.7824183921235,29.5333724842856));
#28311=CARTESIAN_POINT('Ctrl Pts',(33.1978968817731,18.7824143271502,29.5333744922618));
#28312=CARTESIAN_POINT('Ctrl Pts',(33.1635680440817,18.7824096073364,29.5333768470679));
#28313=CARTESIAN_POINT('Ctrl Pts',(33.1258517953345,18.7824044217933,29.5333794342353));
#28314=CARTESIAN_POINT('Ctrl Pts',(33.0899258347186,18.7823984465448,29.5333824396031));
#28315=CARTESIAN_POINT('Ctrl Pts',(33.0557653925385,18.7823915567442,29.5333859335397));
#28316=CARTESIAN_POINT('Ctrl Pts',(33.0368719877468,18.7823877461438,29.5333878659608));
#28317=CARTESIAN_POINT('Ctrl Pts',(33.0185175727354,18.7823836577058,29.5333899466652));
#28318=CARTESIAN_POINT('Ctrl Pts',(33.0006913489163,18.7823792820484,29.5333921804186));
#28319=CARTESIAN_POINT('Ctrl Pts',(32.9433364918127,18.7823652036207,29.5333993673924));
#28320=CARTESIAN_POINT('Ctrl Pts',(32.889323201888,18.78254762761,29.5332829792211));
#28321=CARTESIAN_POINT('Ctrl Pts',(32.8382230276383,18.7828441879673,29.5330947066102));
#28322=CARTESIAN_POINT('Ctrl Pts',(32.7810653124614,18.7831759033221,29.5328841156987));
#28323=CARTESIAN_POINT('Ctrl Pts',(32.7275524567343,18.7836507315896,29.5325833908465));
#28324=CARTESIAN_POINT('Ctrl Pts',(32.6770430180207,18.7841988326963,29.532236338609));
#28325=CARTESIAN_POINT('Ctrl Pts',(32.6227203152385,18.7847883132819,29.5318630852917));
#28326=CARTESIAN_POINT('Ctrl Pts',(32.5718714572482,18.785463223046,29.5314358211882));
#28327=CARTESIAN_POINT('Ctrl Pts',(32.5236533105898,18.7861776883227,29.5309832901274));
#28328=CARTESIAN_POINT('Ctrl Pts',(32.4718100172058,18.7869458686764,29.5304967367823));
#28329=CARTESIAN_POINT('Ctrl Pts',(32.4230076638019,18.7877604440451,29.5299805544879));
#28330=CARTESIAN_POINT('Ctrl Pts',(32.3761512174013,18.7885990068259,29.5294487410664));
#28331=CARTESIAN_POINT('Ctrl Pts',(32.3248096593255,18.789517837062,29.5288660223209));
#28332=CARTESIAN_POINT('Ctrl Pts',(32.2758043952282,18.7904660501636,29.5282641699575));
#28333=CARTESIAN_POINT('Ctrl Pts',(32.2276418902258,18.7914438969209,29.5276429421487));
#28334=CARTESIAN_POINT('Ctrl Pts',(32.1780484881801,18.7924507952825,29.5270032578033));
#28335=CARTESIAN_POINT('Ctrl Pts',(32.1293485209749,18.7934898292201,29.5263425802702));
#28336=CARTESIAN_POINT('Ctrl Pts',(32.0798596724235,18.7945806304077,29.525648507911));
#28337=CARTESIAN_POINT('Ctrl Pts',(32.0310319729845,18.7956568589742,29.5249637080513));
#28338=CARTESIAN_POINT('Ctrl Pts',(31.9814363681892,18.7967841298918,29.5242459916461));
#28339=CARTESIAN_POINT('Ctrl Pts',(31.9294088358077,18.7979897030586,29.5234781935337));
#28340=CARTESIAN_POINT('Ctrl Pts',(31.8980169364549,18.7987171108326,29.523014926491));
#28341=CARTESIAN_POINT('Ctrl Pts',(31.8657387727397,18.7994731540541,29.5225333463335));
#28342=CARTESIAN_POINT('Ctrl Pts',(31.8321995512669,18.8002637764333,29.5220297160307));
#28343=CARTESIAN_POINT('Ctrl Pts',(31.7313430764711,18.8026412730643,29.5205152391074));
#28344=CARTESIAN_POINT('Ctrl Pts',(31.6280303047182,18.8051208626313,29.5189339807854));
#28345=CARTESIAN_POINT('Ctrl Pts',(31.5230436279567,18.8075570028382,29.5173797885034));
#28346=CARTESIAN_POINT('Ctrl Pts',(31.4165412786076,18.8100283131358,29.5158031586445));
#28347=CARTESIAN_POINT('Ctrl Pts',(31.3083161729143,18.8124535008248,29.5142552682412));
#28348=CARTESIAN_POINT('Ctrl Pts',(31.1992361814709,18.8146708543331,29.512840201736));
#28349=CARTESIAN_POINT('Ctrl Pts',(31.1417800745717,18.8158388091388,29.5120948385276));
#28350=CARTESIAN_POINT('Ctrl Pts',(31.0840876480107,18.8169490689289,29.5113863465313));
#28351=CARTESIAN_POINT('Ctrl Pts',(31.0262914639722,18.8179790482415,29.5107292749178));
#28352=CARTESIAN_POINT('Ctrl Pts',(30.9238422544136,18.8198047841132,29.5095645532577));
#28353=CARTESIAN_POINT('Ctrl Pts',(30.8210652532058,18.8213763539421,29.5085625948816));
#28354=CARTESIAN_POINT('Ctrl Pts',(30.7187655074561,18.8225556950176,29.507810834769));
#28355=CARTESIAN_POINT('Ctrl Pts',(30.6466529343875,18.82338702963,29.5072809081729));
#28356=CARTESIAN_POINT('Ctrl Pts',(30.5747782907563,18.8240238717387,29.5068750504575));
#28357=CARTESIAN_POINT('Ctrl Pts',(30.5034323951389,18.8244289981691,29.5066169468345));
#28358=CARTESIAN_POINT('Ctrl Pts',(30.5006731185506,18.8244446662866,29.5066069647706));
#28359=CARTESIAN_POINT('Ctrl Pts',(30.497914633606,18.8244599892393,29.5065972028236));
#28360=CARTESIAN_POINT('Ctrl Pts',(30.4951569527683,18.8244749650172,29.5065876622663));
#28361=CARTESIAN_POINT('',(30.5,16.229443021655,31.0097594187194));
#28362=CARTESIAN_POINT('Origin',(30.5,0.,0.));
#28363=CARTESIAN_POINT('Ctrl Pts',(30.5049076308142,16.2304573503027,31.009123868732));
#28364=CARTESIAN_POINT('Ctrl Pts',(30.5973062294347,16.2298682766553,31.0094328533549));
#28365=CARTESIAN_POINT('Ctrl Pts',(30.6890591585862,16.2288427503287,31.009969267703));
#28366=CARTESIAN_POINT('Ctrl Pts',(30.7806364364921,16.2274919709622,31.0106763092386));
#28367=CARTESIAN_POINT('Ctrl Pts',(30.8441456090294,16.2265552005995,31.0111666450937));
#28368=CARTESIAN_POINT('Ctrl Pts',(30.9075713010185,16.2254611740685,31.0117394593185));
#28369=CARTESIAN_POINT('Ctrl Pts',(30.9710816356705,16.2242390174925,31.012379837551));
#28370=CARTESIAN_POINT('Ctrl Pts',(31.0734991469997,16.2222681534488,31.0134125190073));
#28371=CARTESIAN_POINT('Ctrl Pts',(31.1761345288069,16.2199648111637,31.0146205155169));
#28372=CARTESIAN_POINT('Ctrl Pts',(31.2798100568472,16.2174702047239,31.0159286966546));
#28373=CARTESIAN_POINT('Ctrl Pts',(31.3828326297121,16.2149913094767,31.017228638783));
#28374=CARTESIAN_POINT('Ctrl Pts',(31.4868822244314,16.2123218973816,31.0186283615543));
#28375=CARTESIAN_POINT('Ctrl Pts',(31.5928140565566,16.2095937955792,31.0200576696061));
#28376=CARTESIAN_POINT('Ctrl Pts',(31.6516194621086,16.2080793581371,31.0208511142012));
#28377=CARTESIAN_POINT('Ctrl Pts',(31.711005767608,16.2065468518029,31.0216536678952));
#28378=CARTESIAN_POINT('Ctrl Pts',(31.771125977653,16.205020814195,31.0224523036439));
#28379=CARTESIAN_POINT('Ctrl Pts',(31.8409078613428,16.2032495333099,31.023379284885));
#28380=CARTESIAN_POINT('Ctrl Pts',(31.9056298453965,16.2016434584278,31.0242198767435));
#28381=CARTESIAN_POINT('Ctrl Pts',(31.9658749467866,16.2002018139143,31.0249744961548));
#28382=CARTESIAN_POINT('Ctrl Pts',(32.0341046687229,16.198569100183,31.025829129501));
#28383=CARTESIAN_POINT('Ctrl Pts',(32.0965918298942,16.1971462744692,31.0265740158192));
#28384=CARTESIAN_POINT('Ctrl Pts',(32.1542461945015,16.195904238954,31.0272242625031));
#28385=CARTESIAN_POINT('Ctrl Pts',(32.2151665953518,16.1945918439259,31.0279113447198));
#28386=CARTESIAN_POINT('Ctrl Pts',(32.2706916712559,16.1934801514052,31.0284933558529));
#28387=CARTESIAN_POINT('Ctrl Pts',(32.3219582775156,16.1925241206213,31.0289937114783));
#28388=CARTESIAN_POINT('Ctrl Pts',(32.3761916324766,16.1915127652647,31.0295230221977));
#28389=CARTESIAN_POINT('Ctrl Pts',(32.4256599862214,16.1906748064837,31.0299613681538));
#28390=CARTESIAN_POINT('Ctrl Pts',(32.4717693483768,16.1899610544419,31.0303343957025));
#28391=CARTESIAN_POINT('Ctrl Pts',(32.5215332003052,16.1891907325538,31.030736988296));
#28392=CARTESIAN_POINT('Ctrl Pts',(32.5673849287937,16.1885644631732,31.0310638203077));
#28393=CARTESIAN_POINT('Ctrl Pts',(32.6111519417706,16.1880367365759,31.0313387615315));
#28394=CARTESIAN_POINT('Ctrl Pts',(32.655174121074,16.1875059332765,31.0316153056917));
#28395=CARTESIAN_POINT('Ctrl Pts',(32.6970878717828,16.1870745377529,31.0318395012597));
#28396=CARTESIAN_POINT('Ctrl Pts',(32.7388013470518,16.18671857384,31.0320241553174));
#28397=CARTESIAN_POINT('Ctrl Pts',(32.7801521457877,16.1863657048444,31.032207203906));
#28398=CARTESIAN_POINT('Ctrl Pts',(32.8213062770016,16.186086545466,31.0323516104908));
#28399=CARTESIAN_POINT('Ctrl Pts',(32.8641640035295,16.1858844594635,31.0324560971771));
#28400=CARTESIAN_POINT('Ctrl Pts',(32.9038200784534,16.1856974701314,31.0325527782704));
#28401=CARTESIAN_POINT('Ctrl Pts',(32.9449347772907,16.1855761117062,31.0326154655021));
#28402=CARTESIAN_POINT('Ctrl Pts',(32.9890474705827,16.1855509840874,31.0326287580454));
#28403=CARTESIAN_POINT('Ctrl Pts',(32.9926089293378,16.1855489553974,31.032629831225));
#28404=CARTESIAN_POINT('Ctrl Pts',(32.9961899495412,16.1855475722578,31.0326305730129));
#28405=CARTESIAN_POINT('Ctrl Pts',(32.9997913521116,16.185546860962,31.0326309700539));
#28406=CARTESIAN_POINT('Ctrl Pts',(33.0362292496773,16.1855396642873,31.0326349871948));
#28407=CARTESIAN_POINT('Ctrl Pts',(33.0740922921121,16.1855331333215,31.0326386992186));
#28408=CARTESIAN_POINT('Ctrl Pts',(33.1141439185632,16.1855273500632,31.032642249087));
#28409=CARTESIAN_POINT('Ctrl Pts',(33.2461674547435,16.1855082865123,31.0326539506384));
#28410=CARTESIAN_POINT('Ctrl Pts',(33.3721931286569,16.1855003220479,31.0326588963954));
#28411=CARTESIAN_POINT('Ctrl Pts',(33.499387920745,16.185492813855,31.0326635427517));
#28412=CARTESIAN_POINT('Ctrl Pts',(33.6627849160626,16.185483168679,31.0326695115548));
#28413=CARTESIAN_POINT('Ctrl Pts',(33.828111247454,16.1854742764645,31.0326749862724));
#28414=CARTESIAN_POINT('Ctrl Pts',(33.9929845306744,16.1854606405094,31.0326833946006));
#28415=CARTESIAN_POINT('Ctrl Pts',(34.3227310971152,16.1854333685993,31.032700211257));
#28416=CARTESIAN_POINT('Ctrl Pts',(34.650665470872,16.185387121727,31.0327287623561));
#28417=CARTESIAN_POINT('Ctrl Pts',(34.9792693636211,16.1853559472169,31.0327480042371));
#28418=CARTESIAN_POINT('Ctrl Pts',(35.3078732563702,16.1853247727069,31.0327672461181));
#28419=CARTESIAN_POINT('Ctrl Pts',(35.6371466681117,16.185308670559,31.0327771787811));
#28420=CARTESIAN_POINT('Ctrl Pts',(35.9662682695209,16.1852951338217,31.0327855310263));
#28421=CARTESIAN_POINT('Ctrl Pts',(36.2953898709301,16.1852815970843,31.0327938832715));
#28422=CARTESIAN_POINT('Ctrl Pts',(36.624359662007,16.1852706257574,31.0328006550989));
#28423=CARTESIAN_POINT('Ctrl Pts',(36.9532592751493,16.185248102247,31.032814555176));
#28424=CARTESIAN_POINT('Ctrl Pts',(38.1023262780261,16.1851694125147,31.0328631174706));
#28425=CARTESIAN_POINT('Ctrl Pts',(39.2505367075415,16.184949719878,31.0329986853002));
#28426=CARTESIAN_POINT('Ctrl Pts',(40.4000986012038,16.1848953623403,31.0330322281526));
#28427=CARTESIAN_POINT('Ctrl Pts',(6.89999999997365,-0.168526548676479,
11.0276873985587));
#28428=CARTESIAN_POINT('Ctrl Pts',(6.99168932310453,-0.107121039164011,
11.0290491215116));
#28429=CARTESIAN_POINT('Ctrl Pts',(7.08383940291242,-0.0458098125994647,
11.0299018391088));
#28430=CARTESIAN_POINT('Ctrl Pts',(8.15761824498006,0.664186592400573,11.0337651740187));
#28431=CARTESIAN_POINT('Ctrl Pts',(9.166078574375,1.30870352701556,10.9699676285446));
#28432=CARTESIAN_POINT('Ctrl Pts',(11.2535171643192,2.47376106241927,10.7760330567599));
#28433=CARTESIAN_POINT('Ctrl Pts',(12.2576790632369,3.00237606292525,10.6330057282434));
#28434=CARTESIAN_POINT('Ctrl Pts',(14.3563663857894,3.94447005883399,10.3307260661656));
#28435=CARTESIAN_POINT('Ctrl Pts',(15.3658129161116,4.36032593857961,10.1540434041659));
#28436=CARTESIAN_POINT('Ctrl Pts',(17.4727193021212,5.08193366885831,9.82334300624282));
#28437=CARTESIAN_POINT('Ctrl Pts',(18.4888802671461,5.39169279079135,9.64884225911208));
#28438=CARTESIAN_POINT('Ctrl Pts',(19.8473882183425,5.72385817850076,9.45778984314826));
#28439=CARTESIAN_POINT('Ctrl Pts',(20.3451395577183,5.84063156394591,9.38741838105893));
#28440=CARTESIAN_POINT('Ctrl Pts',(21.1198641211409,6.00690103675047,9.28201599203949));
#28441=CARTESIAN_POINT('Ctrl Pts',(21.9116430735678,6.15921075032181,9.18172875488036));
#28442=CARTESIAN_POINT('Ctrl Pts',(22.4533884343746,6.25063668203687,9.12054551137775));
#28443=CARTESIAN_POINT('Ctrl Pts',(22.8546099577479,6.3132089675058,9.07881438233611));
#28444=CARTESIAN_POINT('Ctrl Pts',(23.1058218650381,6.35118260107244,9.05298395410355));
#28445=CARTESIAN_POINT('Ctrl Pts',(23.6175153199788,6.42382403760964,9.00245668094438));
#28446=CARTESIAN_POINT('Ctrl Pts',(24.1364702886545,6.49007583237978,8.95485371029555));
#28447=CARTESIAN_POINT('Ctrl Pts',(24.6629181373247,6.5494442392928,8.91145225308146));
#28448=CARTESIAN_POINT('Ctrl Pts',(25.0606678571037,6.59024788291776,8.88140293076166));
#28449=CARTESIAN_POINT('Ctrl Pts',(25.3945416155883,6.62099228309711,8.85873533710266));
#28450=CARTESIAN_POINT('Ctrl Pts',(25.6627586119465,6.64352323130155,8.84221409068035));
#28451=CARTESIAN_POINT('Ctrl Pts',(25.7972076165426,6.65408072739388,8.83452216013017));
#28452=CARTESIAN_POINT('Ctrl Pts',(26.3824137782947,6.69837697633854,8.80240169886325));
#28453=CARTESIAN_POINT('Ctrl Pts',(27.4369717967155,6.74704662082202,8.76563881905854));
#28454=CARTESIAN_POINT('Ctrl Pts',(28.4593635146676,6.76713562537253,8.74917816753948));
#28455=CARTESIAN_POINT('Ctrl Pts',(29.042748146989,6.7797450529872,8.73952198264541));
#28456=CARTESIAN_POINT('Ctrl Pts',(29.2174939164951,6.7830642423932,8.73701514175015));
#28457=CARTESIAN_POINT('Ctrl Pts',(29.5607048332278,6.78786835107259,8.7333656848919));
#28458=CARTESIAN_POINT('Ctrl Pts',(29.9899637006213,6.79106253935675,8.73093988338426));
#28459=CARTESIAN_POINT('Ctrl Pts',(30.5003627545717,6.79139754852946,8.7306825539187));
#28460=CARTESIAN_POINT('Ctrl Pts',(31.5152290141054,6.78728755019408,8.73381293113857));
#28461=CARTESIAN_POINT('Ctrl Pts',(32.346385618228,6.77838967797265,8.74063107149334));
#28462=CARTESIAN_POINT('Ctrl Pts',(33.1616392309915,6.77840182636605,8.74062146997073));
#28463=CARTESIAN_POINT('Ctrl Pts',(33.4928689770884,6.7784028418104,8.74062052628883));
#28464=CARTESIAN_POINT('Ctrl Pts',(33.9856875201801,6.77840526161274,8.74061852020512));
#28465=CARTESIAN_POINT('Ctrl Pts',(34.479956929609,6.7784068708528,8.74061713883255));
#28466=CARTESIAN_POINT('Ctrl Pts',(35.1382080085716,6.778409075901,8.74061527897129));
#28467=CARTESIAN_POINT('Ctrl Pts',(35.9613703496106,6.7784121544085,8.74061266742265));
#28468=CARTESIAN_POINT('Ctrl Pts',(37.9364530322258,6.77841531264166,8.74060999527038));
#28469=CARTESIAN_POINT('Ctrl Pts',(39.5833333333333,6.77843480602319,8.74059347982545));
#28470=CARTESIAN_POINT('Ctrl Pts',(40.9,6.77843480602319,8.74059347982545));
#28471=CARTESIAN_POINT('Ctrl Pts',(6.71972576838711,-0.727849695365753,
14.4135489955738));
#28472=CARTESIAN_POINT('Ctrl Pts',(6.81144220747046,-0.647520064289724,
14.4181051875223));
#28473=CARTESIAN_POINT('Ctrl Pts',(6.90362846895808,-0.567280569774696,
14.4219897194692));
#28474=CARTESIAN_POINT('Ctrl Pts',(7.97787094717212,0.361837668282342,14.4591555519285));
#28475=CARTESIAN_POINT('Ctrl Pts',(8.98682261267022,1.20743712855002,14.4048184698324));
#28476=CARTESIAN_POINT('Ctrl Pts',(11.0806424583842,2.7442230049829,14.2022941804566));
#28477=CARTESIAN_POINT('Ctrl Pts',(12.0862214600972,3.4422325745447,14.038891127913));
#28478=CARTESIAN_POINT('Ctrl Pts',(14.1975721203649,4.69396502652543,13.6830024292515));
#28479=CARTESIAN_POINT('Ctrl Pts',(15.2099789251839,5.24642829788654,13.4699449244818));
#28480=CARTESIAN_POINT('Ctrl Pts',(17.3362999248755,6.21145869787376,13.0656161985035));
#28481=CARTESIAN_POINT('Ctrl Pts',(18.357013455463,6.62511541331197,12.8502526120859));
#28482=CARTESIAN_POINT('Ctrl Pts',(19.7328409259837,7.07198752003368,12.6121436508471));
#28483=CARTESIAN_POINT('Ctrl Pts',(20.2337632876373,7.2284111452015,12.5247332071257));
#28484=CARTESIAN_POINT('Ctrl Pts',(21.0166345413949,7.45203181169806,12.3929576501156));
#28485=CARTESIAN_POINT('Ctrl Pts',(21.8175391230323,7.65714338227214,12.2672157657621));
#28486=CARTESIAN_POINT('Ctrl Pts',(22.3668263920487,7.7805494741423,12.190248920123));
#28487=CARTESIAN_POINT('Ctrl Pts',(22.7739396967848,7.8650629816421,12.1377120270328));
#28488=CARTESIAN_POINT('Ctrl Pts',(23.0274297041713,7.91615663273499,12.1053188608807));
#28489=CARTESIAN_POINT('Ctrl Pts',(23.5449351393661,8.01409846114017,12.0417665186343));
#28490=CARTESIAN_POINT('Ctrl Pts',(24.0699575659665,8.1034816713378,11.9817953425795));
#28491=CARTESIAN_POINT('Ctrl Pts',(24.6032835407751,8.18369268569516,11.9270075754273));
#28492=CARTESIAN_POINT('Ctrl Pts',(25.0064847905103,8.2388595218387,11.8890391550575));
#28493=CARTESIAN_POINT('Ctrl Pts',(25.3452465270806,8.28045801654028,11.8603696837558));
#28494=CARTESIAN_POINT('Ctrl Pts',(25.6175460563752,8.31095886138246,11.8394640015962));
#28495=CARTESIAN_POINT('Ctrl Pts',(25.7540942648801,8.3252551228897,11.829728241242));
#28496=CARTESIAN_POINT('Ctrl Pts',(26.3487780629201,8.38525559473469,11.7890598714194));
#28497=CARTESIAN_POINT('Ctrl Pts',(27.420647343066,8.4511591136706,11.7424863739248));
#28498=CARTESIAN_POINT('Ctrl Pts',(28.4470245212717,8.47809267828293,11.7218144944205));
#28499=CARTESIAN_POINT('Ctrl Pts',(29.0301431861017,8.49498332574133,11.7097207064843));
#28500=CARTESIAN_POINT('Ctrl Pts',(29.2075511609936,8.49948124637053,11.7065424548688));
#28501=CARTESIAN_POINT('Ctrl Pts',(29.5540559241345,8.50596054299456,11.7019389390663));
#28502=CARTESIAN_POINT('Ctrl Pts',(29.9873899374288,8.51027178683719,11.6988759349841));
#28503=CARTESIAN_POINT('Ctrl Pts',(30.5010585876109,8.51072031244604,11.698553559564));
#28504=CARTESIAN_POINT('Ctrl Pts',(31.520398261889,8.50519297418973,11.7024891534661));
#28505=CARTESIAN_POINT('Ctrl Pts',(32.3504760849347,8.49329404471494,11.7110091605269));
#28506=CARTESIAN_POINT('Ctrl Pts',(33.1607219786944,8.49331406281709,11.7109930603161));
#28507=CARTESIAN_POINT('Ctrl Pts',(33.4925972550183,8.49331574772296,11.7109914601493));
#28508=CARTESIAN_POINT('Ctrl Pts',(33.9851239882619,8.49331974280041,11.7109880844892));
#28509=CARTESIAN_POINT('Ctrl Pts',(34.4795557496198,8.49332240354984,11.7109857543654));
#28510=CARTESIAN_POINT('Ctrl Pts',(35.1377808103951,8.49332604669792,11.7109826209376));
#28511=CARTESIAN_POINT('Ctrl Pts',(35.9610196518539,8.49333113419868,11.7109782193289));
#28512=CARTESIAN_POINT('Ctrl Pts',(37.9361278153251,8.49333635287233,11.7109737164008));
#28513=CARTESIAN_POINT('Ctrl Pts',(39.5833333333333,8.49336856563261,11.7109458830841));
#28514=CARTESIAN_POINT('Ctrl Pts',(40.9,8.49336856563261,11.7109458830841));
#28515=CARTESIAN_POINT('Ctrl Pts',(6.48175880232276,-2.0223358101383,22.3152648782349));
#28516=CARTESIAN_POINT('Ctrl Pts',(6.5727030402579,-1.89877066361229,22.3270401223923));
#28517=CARTESIAN_POINT('Ctrl Pts',(6.66410021308729,-1.77531589258794,22.3377778183098));
#28518=CARTESIAN_POINT('Ctrl Pts',(7.73046719612231,-0.343647388924402,
22.4505948584363));
#28519=CARTESIAN_POINT('Ctrl Pts',(8.73293490974101,0.965853752252133,22.4183684385317));
#28520=CARTESIAN_POINT('Ctrl Pts',(10.8102891123216,3.35126151217316,22.1981640385547));
#28521=CARTESIAN_POINT('Ctrl Pts',(11.8125652928685,4.44249581664875,21.9890905805955));
#28522=CARTESIAN_POINT('Ctrl Pts',(13.9177091187558,6.40690464277104,21.5128074248294));
#28523=CARTESIAN_POINT('Ctrl Pts',(14.9295907318602,7.27826244175742,21.2167997396941));
#28524=CARTESIAN_POINT('Ctrl Pts',(17.0679705254901,8.81262608188775,20.6429560449296));
#28525=CARTESIAN_POINT('Ctrl Pts',(18.0930327325161,9.47115000177602,20.3328482957164));
#28526=CARTESIAN_POINT('Ctrl Pts',(19.493165165493,10.1918150595347,19.9834260609174));
#28527=CARTESIAN_POINT('Ctrl Pts',(19.9989304172551,10.4420751188792,19.8560672526628));
#28528=CARTESIAN_POINT('Ctrl Pts',(20.7948115947079,10.8025573386247,19.6618467626018));
#28529=CARTESIAN_POINT('Ctrl Pts',(21.6117660259797,11.134285926341,19.4754657432765));
#28530=CARTESIAN_POINT('Ctrl Pts',(22.1753497026275,11.3349591405941,19.3605546952356));
#28531=CARTESIAN_POINT('Ctrl Pts',(22.5940479063322,11.47260657239,19.2819382297017));
#28532=CARTESIAN_POINT('Ctrl Pts',(22.8520812047022,11.5550617085391,19.2339198113556));
#28533=CARTESIAN_POINT('Ctrl Pts',(23.3813360719091,11.7138435277865,19.1391573021403));
#28534=CARTESIAN_POINT('Ctrl Pts',(23.9190563543678,11.8589452906513,19.0494991042743));
#28535=CARTESIAN_POINT('Ctrl Pts',(24.4671051082233,11.989559546254,18.9672572385016));
#28536=CARTESIAN_POINT('Ctrl Pts',(24.8821466483762,12.0795190000423,18.9101500634532));
#28537=CARTESIAN_POINT('Ctrl Pts',(25.2317043848842,12.1474851335067,18.8669280179622));
#28538=CARTESIAN_POINT('Ctrl Pts',(25.513095090024,12.1973721681455,18.8353673631032));
#28539=CARTESIAN_POINT('Ctrl Pts',(25.6543465475615,12.2207724172662,18.8206563371688));
#28540=CARTESIAN_POINT('Ctrl Pts',(26.2703768283174,12.3190725812828,18.7591443923488));
#28541=CARTESIAN_POINT('Ctrl Pts',(27.3823409200252,12.4269409232394,18.6887004197342));
#28542=CARTESIAN_POINT('Ctrl Pts',(28.4180912195453,12.4698946357076,18.6581821178487));
#28543=CARTESIAN_POINT('Ctrl Pts',(29.0006188348746,12.4967855079752,18.6404003655932));
#28544=CARTESIAN_POINT('Ctrl Pts',(29.1842244806991,12.5041566301776,18.6355848623939));
#28545=CARTESIAN_POINT('Ctrl Pts',(29.5384110471464,12.5146498740616,18.6286952117012));
#28546=CARTESIAN_POINT('Ctrl Pts',(29.9812601150293,12.5216494975055,18.6240999155071));
#28547=CARTESIAN_POINT('Ctrl Pts',(30.5025631839301,12.5223645690812,18.6236255844565));
#28548=CARTESIAN_POINT('Ctrl Pts',(31.5323495650756,12.5134871029148,18.6294670720537));
#28549=CARTESIAN_POINT('Ctrl Pts',(32.3599484134841,12.4946603930139,18.6419219593216));
#28550=CARTESIAN_POINT('Ctrl Pts',(33.1585258504257,12.4947174829697,18.6418830267369));
#28551=CARTESIAN_POINT('Ctrl Pts',(33.4919095878066,12.4947228565318,18.6418790995137));
#28552=CARTESIAN_POINT('Ctrl Pts',(33.9837592380106,12.4947346270607,18.6418708983646));
#28553=CARTESIAN_POINT('Ctrl Pts',(34.4785726427749,12.4947426563109,18.6418652189505));
#28554=CARTESIAN_POINT('Ctrl Pts',(35.1367406589071,12.4947535178469,18.6418575939256));
#28555=CARTESIAN_POINT('Ctrl Pts',(35.9601632093982,12.4947687456191,18.641846877137));
#28556=CARTESIAN_POINT('Ctrl Pts',(37.9353361278946,12.4947843377882,18.6418359163297));
#28557=CARTESIAN_POINT('Ctrl Pts',(39.5833333333333,12.4948806713879,18.6417681573542));
#28558=CARTESIAN_POINT('Ctrl Pts',(40.9,12.4948806713879,18.6417681573542));
#28559=CARTESIAN_POINT('Ctrl Pts',(6.40644620858992,-3.20016516784476,30.2320800787095));
#28560=CARTESIAN_POINT('Ctrl Pts',(6.49686818484384,-3.03404698664168,30.2503623618083));
#28561=CARTESIAN_POINT('Ctrl Pts',(6.58771890650217,-2.86810360702044,30.2672526113879));
#28562=CARTESIAN_POINT('Ctrl Pts',(7.64885862899863,-0.940991822615552,
30.4476905739237));
#28563=CARTESIAN_POINT('Ctrl Pts',(8.64788707329235,0.826287776604457,30.430792173042));
#28564=CARTESIAN_POINT('Ctrl Pts',(10.707154859542,4.03135720303698,30.1856445659011));
#28565=CARTESIAN_POINT('Ctrl Pts',(11.7059935225822,5.50908116677457,29.9282222211751));
#28566=CARTESIAN_POINT('Ctrl Pts',(13.7894394913649,8.15261547988189,29.3339211293756));
#28567=CARTESIAN_POINT('Ctrl Pts',(14.7965025532944,9.33507154947814,28.9559671306032));
#28568=CARTESIAN_POINT('Ctrl Pts',(16.9150296648081,11.4103698853377,28.2210428396417));
#28569=CARTESIAN_POINT('Ctrl Pts',(17.9356459667172,12.3080290796725,27.8189128366825));
#28570=CARTESIAN_POINT('Ctrl Pts',(19.3316976380886,13.2937048286053,27.3625462801585));
#28571=CARTESIAN_POINT('Ctrl Pts',(19.8372125803626,13.6366910969767,27.1960046691454));
#28572=CARTESIAN_POINT('Ctrl Pts',(20.6335801906183,14.1320040365234,26.9406914971977));
#28573=CARTESIAN_POINT('Ctrl Pts',(21.4537597225929,14.5899345529251,26.6943052661746));
#28574=CARTESIAN_POINT('Ctrl Pts',(22.0223258890083,14.8686659459061,26.5413031957662));
#28575=CARTESIAN_POINT('Ctrl Pts',(22.4461030502075,15.0605640384028,26.436200781156));
#28576=CARTESIAN_POINT('Ctrl Pts',(22.7062608359972,15.1748824403433,26.3723989822776));
#28577=CARTESIAN_POINT('Ctrl Pts',(23.2414929286472,15.3959532265256,26.2458547955408));
#28578=CARTESIAN_POINT('Ctrl Pts',(23.7867279834487,15.5986167246948,26.1256827576298));
#28579=CARTESIAN_POINT('Ctrl Pts',(24.3445890668936,15.7819085569279,26.0148742888258));
#28580=CARTESIAN_POINT('Ctrl Pts',(24.7681394700222,15.9085256074862,25.9376795444546));
#28581=CARTESIAN_POINT('Ctrl Pts',(25.1260106169384,16.0045350828092,25.8790242908719));
#28582=CARTESIAN_POINT('Ctrl Pts',(25.4147345926425,16.0751760807979,25.8360764159908));
#28583=CARTESIAN_POINT('Ctrl Pts',(25.5598889289847,16.1083660281042,25.8160190309821));
#28584=CARTESIAN_POINT('Ctrl Pts',(26.1939339115031,16.2480157393789,25.7320023110876));
#28585=CARTESIAN_POINT('Ctrl Pts',(27.3441597812047,16.4017510524694,25.6354753903564));
#28586=CARTESIAN_POINT('Ctrl Pts',(28.3894038584673,16.4608066876633,25.5950614103761));
#28587=CARTESIAN_POINT('Ctrl Pts',(28.9713246547181,16.4977059168026,25.5715886293348));
#28588=CARTESIAN_POINT('Ctrl Pts',(29.1610585442185,16.5082319208974,25.5649734110424));
#28589=CARTESIAN_POINT('Ctrl Pts',(29.5228882487203,16.5229807852931,25.555658015613));
#28590=CARTESIAN_POINT('Ctrl Pts',(29.9752283100297,16.5328527231063,25.5494240137561));
#28591=CARTESIAN_POINT('Ctrl Pts',(30.5041683224499,16.5338357099673,25.5487969550271));
#28592=CARTESIAN_POINT('Ctrl Pts',(31.5443819697417,16.521500293953,25.5566068476797));
#28593=CARTESIAN_POINT('Ctrl Pts',(32.369479464394,16.4958953935747,25.5729102090687));
#28594=CARTESIAN_POINT('Ctrl Pts',(33.1563754893963,16.4960222658506,25.5728296448089));
#28595=CARTESIAN_POINT('Ctrl Pts',(33.4912658278754,16.4960347835491,25.572821407314));
#28596=CARTESIAN_POINT('Ctrl Pts',(33.9824352992262,16.4960613233721,25.5728043629855));
#28597=CARTESIAN_POINT('Ctrl Pts',(34.4776280283123,16.4960796138348,25.5727925244551));
#28598=CARTESIAN_POINT('Ctrl Pts',(35.1357360035508,16.4961042295225,25.5727766538609));
#28599=CARTESIAN_POINT('Ctrl Pts',(35.9593379975622,16.4961387987433,25.5727543372373));
#28600=CARTESIAN_POINT('Ctrl Pts',(37.9345713338106,16.4961741679457,25.5727315175493));
#28601=CARTESIAN_POINT('Ctrl Pts',(39.5833333333333,16.4963927771432,25.5725904316243));
#28602=CARTESIAN_POINT('Ctrl Pts',(40.9,16.4963927771432,25.5725904316243));
#28603=CARTESIAN_POINT('Ctrl Pts',(6.37427268165564,-3.85496595036638,34.7583359408307));
#28604=CARTESIAN_POINT('Ctrl Pts',(6.46448755772839,-3.664463752464,34.7802475524424));
#28605=CARTESIAN_POINT('Ctrl Pts',(6.55512331969025,-3.47417181608894,34.8005635888992));
#28606=CARTESIAN_POINT('Ctrl Pts',(7.61410548625795,-1.26339052014806,35.0185788676572));
#28607=CARTESIAN_POINT('Ctrl Pts',(8.61145388480625,0.765602457207675,35.0093532870147));
#28608=CARTESIAN_POINT('Ctrl Pts',(10.6635149436019,4.43910992978123,34.747974440135));
#28609=CARTESIAN_POINT('Ctrl Pts',(11.6608017032625,6.13747453196183,34.4619345886989));
#28610=CARTESIAN_POINT('Ctrl Pts',(13.7353542747945,9.16685810272321,33.7990269238398));
#28611=CARTESIAN_POINT('Ctrl Pts',(14.7402715202385,10.5262979552789,33.3736740493576));
#28612=CARTESIAN_POINT('Ctrl Pts',(16.8491677832146,12.9054531131771,32.5473921410153));
#28613=CARTESIAN_POINT('Ctrl Pts',(17.8672809631135,13.938220333161,32.0928860415559));
#28614=CARTESIAN_POINT('Ctrl Pts',(19.2587625104672,15.0707179501981,31.5771798698669));
#28615=CARTESIAN_POINT('Ctrl Pts',(19.7635899403542,15.4658689812883,31.3885503410944));
#28616=CARTESIAN_POINT('Ctrl Pts',(20.5586991602296,16.0362969262866,31.0991569516509));
#28617=CARTESIAN_POINT('Ctrl Pts',(21.3785272493018,16.5645337867929,30.819343278526));
#28618=CARTESIAN_POINT('Ctrl Pts',(21.9479176287994,16.8867906552356,30.6451300260617));
#28619=CARTESIAN_POINT('Ctrl Pts',(22.3729695502115,17.1090467735267,30.5252344400129));
#28620=CARTESIAN_POINT('Ctrl Pts',(22.6337096028248,17.2413581349254,30.45253373981));
#28621=CARTESIAN_POINT('Ctrl Pts',(23.170751986421,17.4975676797996,30.3080867629257));
#28622=CARTESIAN_POINT('Ctrl Pts',(23.7186485394885,17.7328951431605,30.1706268071311));
#28623=CARTESIAN_POINT('Ctrl Pts',(24.2804077704386,17.9462491604951,30.0435395405948));
#28624=CARTESIAN_POINT('Ctrl Pts',(24.7075732751059,18.093896808302,29.9548357769836));
#28625=CARTESIAN_POINT('Ctrl Pts',(25.0692008252976,18.2061112471098,29.8872739715488));
#28626=CARTESIAN_POINT('Ctrl Pts',(25.3613771492326,18.2888047627701,29.8377189043885));
#28627=CARTESIAN_POINT('Ctrl Pts',(25.5084154817281,18.3277015544067,29.8145466170754));
#28628=CARTESIAN_POINT('Ctrl Pts',(26.1512870025444,18.4915385207408,29.7173716879778));
#28629=CARTESIAN_POINT('Ctrl Pts',(27.3223884400173,18.6726738474942,29.6052740416531));
#28630=CARTESIAN_POINT('Ctrl Pts',(28.373139604832,18.7409825767551,29.559177524821));
#28631=CARTESIAN_POINT('Ctrl Pts',(28.9547046473314,18.7836137746098,29.5324480977278));
#28632=CARTESIAN_POINT('Ctrl Pts',(29.1479037067737,18.7960320303041,29.5247529606443));
#28633=CARTESIAN_POINT('Ctrl Pts',(29.514080236792,18.8132921881813,29.51400582112));
#28634=CARTESIAN_POINT('Ctrl Pts',(29.9718311305157,18.8248686377542,29.5067996680496));
#28635=CARTESIAN_POINT('Ctrl Pts',(30.5051365276118,18.8260067178222,29.5060845192011));
#28636=CARTESIAN_POINT('Ctrl Pts',(31.551298475448,18.8116639693828,29.5150383037988));
#28637=CARTESIAN_POINT('Ctrl Pts',(32.3749555043413,18.7822473977007,29.5335081969198));
#28638=CARTESIAN_POINT('Ctrl Pts',(33.1551698865007,18.7824304492383,29.5333957726549));
#28639=CARTESIAN_POINT('Ctrl Pts',(33.4909201969602,18.782448957068,29.5333841560219));
#28640=CARTESIAN_POINT('Ctrl Pts',(33.981699427726,18.7824875453787,29.5333602907362));
#28641=CARTESIAN_POINT('Ctrl Pts',(34.4771077390558,18.7825142819534,29.533343676228));
#28642=CARTESIAN_POINT('Ctrl Pts',(35.1351798881798,18.7825501686284,29.5333214285967));
#28643=CARTESIAN_POINT('Ctrl Pts',(35.958882261465,18.7826006107083,29.5332901329543));
#28644=CARTESIAN_POINT('Ctrl Pts',(37.9341479260215,18.7826521993715,29.5332581373787));
#28645=CARTESIAN_POINT('Ctrl Pts',(39.5833333333333,18.7829711232891,29.5330603026358));
#28646=CARTESIAN_POINT('Ctrl Pts',(40.9,18.7829711232891,29.5330603026358));
#28647=CARTESIAN_POINT('',(40.9,17.7819838375536,27.7992994660114));
#28648=CARTESIAN_POINT('Ctrl Pts',(40.9,17.7819838375536,27.7992994660114));
#28649=CARTESIAN_POINT('Ctrl Pts',(40.9,18.0322312401327,28.2327406817405));
#28650=CARTESIAN_POINT('Ctrl Pts',(40.9,18.2824786427117,28.6661818974695));
#28651=CARTESIAN_POINT('Ctrl Pts',(40.9,18.5327260452908,29.0996231131986));
#28652=CARTESIAN_POINT('',(38.,17.7819838375536,27.7992994660114));
#28653=CARTESIAN_POINT('Ctrl Pts',(38.,17.7819838375536,27.7992994660114));
#28654=CARTESIAN_POINT('Ctrl Pts',(38.9666666666667,17.7819838375536,27.7992994660114));
#28655=CARTESIAN_POINT('Ctrl Pts',(39.9333333333333,17.7819838375536,27.7992994660114));
#28656=CARTESIAN_POINT('Ctrl Pts',(40.9,17.7819838375536,27.7992994660114));
#28657=CARTESIAN_POINT('Ctrl Pts',(37.4972421947179,17.4814252073799,27.2792895089189));
#28658=CARTESIAN_POINT('Ctrl Pts',(37.6643036200225,17.5817077438357,27.4529624980705));
#28659=CARTESIAN_POINT('Ctrl Pts',(37.8311445342373,17.6818443698597,27.6263779214721));
#28660=CARTESIAN_POINT('Ctrl Pts',(37.9976555467136,17.7817739539416,27.7994312893194));
#28661=CARTESIAN_POINT('',(6.9,-2.26556458774885,29.9143312995417));
#28662=CARTESIAN_POINT('Ctrl Pts',(6.9,-2.26556458774884,29.9143312995417));
#28663=CARTESIAN_POINT('Ctrl Pts',(6.9,-2.00382962437803,27.3056186709172));
#28664=CARTESIAN_POINT('Ctrl Pts',(6.90000000000115,-1.73285728374609,24.6693701926632));
#28665=CARTESIAN_POINT('Ctrl Pts',(6.90000000000115,-1.09593289590079,18.7182130985667));
#28666=CARTESIAN_POINT('Ctrl Pts',(6.9,-0.654794893503693,14.7845781982083));
#28667=CARTESIAN_POINT('Ctrl Pts',(6.9,-0.168526548660249,11.02768739857));
#28668=CARTESIAN_POINT('',(22.9245129145126,15.8853026165582,27.5141512254856));
#28669=CARTESIAN_POINT('Ctrl Pts',(22.9245129145126,15.8853026165582,27.5141512254856));
#28670=CARTESIAN_POINT('Ctrl Pts',(22.7202811020963,15.7659233420327,27.5032269692373));
#28671=CARTESIAN_POINT('Ctrl Pts',(22.5089075447093,15.6398559109135,27.4959054260063));
#28672=CARTESIAN_POINT('Ctrl Pts',(22.2913349439917,15.5073965833875,27.4928730439354));
#28673=CARTESIAN_POINT('Ctrl Pts',(21.4451770585292,14.9922512750189,27.4810798586143));
#28674=CARTESIAN_POINT('Ctrl Pts',(20.5220951556666,14.3509960808545,27.5650257717264));
#28675=CARTESIAN_POINT('Ctrl Pts',(19.7671428819537,13.7859304181012,27.6762399607749));
#28676=CARTESIAN_POINT('Ctrl Pts',(19.519477305839,13.6005580206911,27.7127242885422));
#28677=CARTESIAN_POINT('Ctrl Pts',(19.286571638609,13.421872324025,27.7514615171004));
#28678=CARTESIAN_POINT('Ctrl Pts',(19.0728538401323,13.2552441975238,27.7894004949774));
#28679=CARTESIAN_POINT('Ctrl Pts',(18.7028555998035,12.9667697979459,27.8550822264681));
#28680=CARTESIAN_POINT('Ctrl Pts',(18.4144703596235,12.7292901983115,27.9152561335183));
#28681=CARTESIAN_POINT('Ctrl Pts',(18.0642874871537,12.4284122845046,27.9946062155751));
#28682=CARTESIAN_POINT('Ctrl Pts',(17.4420927116721,11.8938211301512,28.1355931408966));
#28683=CARTESIAN_POINT('Ctrl Pts',(16.7224564418218,11.2282910364347,28.3254287038798));
#28684=CARTESIAN_POINT('Ctrl Pts',(15.9202806616111,10.4246142212493,28.5439924969395));
#28685=CARTESIAN_POINT('Ctrl Pts',(15.409052983451,9.91242993152873,28.6832834892783));
#28686=CARTESIAN_POINT('Ctrl Pts',(14.8739602945697,9.33532862360144,28.8377564730268));
#28687=CARTESIAN_POINT('Ctrl Pts',(14.3169794331127,8.69171842999057,28.9944199787771));
#28688=CARTESIAN_POINT('Ctrl Pts',(13.8864206762817,8.19419324731197,29.1155243989544));
#28689=CARTESIAN_POINT('Ctrl Pts',(13.3867890027792,7.59173852184979,29.2546860278647));
#28690=CARTESIAN_POINT('Ctrl Pts',(12.8146824059514,6.86770373383357,29.3960736315876));
#28691=CARTESIAN_POINT('Ctrl Pts',(12.2526665517594,6.15643937836573,29.5349674589251));
#28692=CARTESIAN_POINT('Ctrl Pts',(11.6379478462802,5.32066918438549,29.678401911158));
#28693=CARTESIAN_POINT('Ctrl Pts',(10.9739250490306,4.35448584003976,29.7956367796097));
#28694=CARTESIAN_POINT('Ctrl Pts',(10.5683455447962,3.76434923114256,29.8672428449776));
#28695=CARTESIAN_POINT('Ctrl Pts',(10.1437415406955,3.12422765605926,29.9275397584159));
#28696=CARTESIAN_POINT('Ctrl Pts',(9.74137929176525,2.50486371218384,29.9670595377668));
#28697=CARTESIAN_POINT('Ctrl Pts',(8.72285779294234,0.937033991304201,30.0670981099855));
#28698=CARTESIAN_POINT('Ctrl Pts',(7.81323138778195,-0.63845182530268,30.0560666286387));
#28699=CARTESIAN_POINT('Ctrl Pts',(6.9,-2.26556458774884,29.9143312995417));
#28700=CARTESIAN_POINT('Ctrl Pts',(30.5,18.8254200738635,29.5059919176187));
#28701=CARTESIAN_POINT('Ctrl Pts',(29.9560179420816,18.7064245513841,29.293615660989));
#28702=CARTESIAN_POINT('Ctrl Pts',(29.4152668325132,18.5734800115823,29.0895919906434));
#28703=CARTESIAN_POINT('Ctrl Pts',(28.8740459957565,18.4125151878636,28.9020067835811));
#28704=CARTESIAN_POINT('Ctrl Pts',(28.353527792344,18.2577075471291,28.7215970352204));
#28705=CARTESIAN_POINT('Ctrl Pts',(27.8179515912466,18.1008601332297,28.5331399346289));
#28706=CARTESIAN_POINT('Ctrl Pts',(27.2695051149491,17.9186544331585,28.3565719042575));
#28707=CARTESIAN_POINT('Ctrl Pts',(26.9554553615883,17.8143203592948,28.2554660556725));
#28708=CARTESIAN_POINT('Ctrl Pts',(26.637809929697,17.7019284120276,28.1585101274348));
#28709=CARTESIAN_POINT('Ctrl Pts',(26.3179304017917,17.5778023417279,28.0701057587103));
#28710=CARTESIAN_POINT('Ctrl Pts',(26.1078196745982,17.4962709631331,28.012037940737));
#28711=CARTESIAN_POINT('Ctrl Pts',(25.8967402232745,17.409683568055,27.9576659729224));
#28712=CARTESIAN_POINT('Ctrl Pts',(25.6850706236774,17.3169960819306,27.9082593406129));
#28713=CARTESIAN_POINT('Ctrl Pts',(25.6562210027417,17.3043631915899,27.9015254373195));
#28714=CARTESIAN_POINT('Ctrl Pts',(25.6277737638215,17.2918013331136,27.8949772388532));
#28715=CARTESIAN_POINT('Ctrl Pts',(25.5983858063598,17.2787081509674,27.8883138877393));
#28716=CARTESIAN_POINT('Ctrl Pts',(25.1249357452756,17.067772501732,27.7809650188704));
#28717=CARTESIAN_POINT('Ctrl Pts',(24.1510084067019,16.6022239440147,27.5797558484168));
#28718=CARTESIAN_POINT('Ctrl Pts',(22.9245129145126,15.8853026165582,27.5141512254856));
#28719=CARTESIAN_POINT('Origin',(40.65,0.,0.));
#28720=CARTESIAN_POINT('',(40.4,-1.5,34.9678423698117));
#28721=CARTESIAN_POINT('',(40.9,-1.5,34.4673758792282));
#28722=CARTESIAN_POINT('Ctrl Pts',(40.4,-1.5,34.9678423698117));
#28723=CARTESIAN_POINT('Ctrl Pts',(40.5666590135434,-1.5,34.801030090909));
#28724=CARTESIAN_POINT('Ctrl Pts',(40.7333430449885,-1.5,34.6341905786716));
#28725=CARTESIAN_POINT('Ctrl Pts',(40.9,-1.5,34.4673758792282));
#28726=CARTESIAN_POINT('',(40.9,1.50000000000002,34.4673758792282));
#28727=CARTESIAN_POINT('Origin',(40.9,0.,0.));
#28728=CARTESIAN_POINT('',(40.4,1.5,34.9678423698117));
#28729=CARTESIAN_POINT('Ctrl Pts',(40.9,1.5,34.4673758792282));
#28730=CARTESIAN_POINT('Ctrl Pts',(40.7333430449643,1.5,34.6341905786958));
#28731=CARTESIAN_POINT('Ctrl Pts',(40.566659013779,1.5,34.8010300906732));
#28732=CARTESIAN_POINT('Ctrl Pts',(40.4,1.5,34.9678423698117));
#28733=CARTESIAN_POINT('Origin',(40.4,0.,0.));
#28734=CARTESIAN_POINT('Origin',(35.7,0.,0.));
#28735=CARTESIAN_POINT('',(30.5,1.55029606206997,34.9656486014478));
#28736=CARTESIAN_POINT('Ctrl Pts',(40.3999921398529,1.49999538724755,34.9678423429768));
#28737=CARTESIAN_POINT('Ctrl Pts',(39.2499570215113,1.49997501500716,34.9678422244593));
#28738=CARTESIAN_POINT('Ctrl Pts',(38.0998114916604,1.49989311899335,34.9678417480135));
#28739=CARTESIAN_POINT('Ctrl Pts',(36.9497038557168,1.49987059349837,34.9678416168427));
#28740=CARTESIAN_POINT('Ctrl Pts',(36.785105117964,1.49986736974093,34.96784159807));
#28741=CARTESIAN_POINT('Ctrl Pts',(36.6205071563607,1.49986536202073,34.9678415863694));
#28742=CARTESIAN_POINT('Ctrl Pts',(36.4559233022361,1.49986268095531,34.9678415707796));
#28743=CARTESIAN_POINT('Ctrl Pts',(36.4193640724435,1.4998620854067,34.9678415673166));
#28744=CARTESIAN_POINT('Ctrl Pts',(36.3828055387466,1.49986145663366,34.9678415636617));
#28745=CARTESIAN_POINT('Ctrl Pts',(36.3462474593958,1.49986080263033,34.967841559861));
#28746=CARTESIAN_POINT('Ctrl Pts',(36.0895450699579,1.49985621036995,34.967841533173));
#28747=CARTESIAN_POINT('Ctrl Pts',(35.8501671305851,1.49985084735668,34.9678416196704));
#28748=CARTESIAN_POINT('Ctrl Pts',(35.6266230092018,1.49984692867086,34.9678417642539));
#28749=CARTESIAN_POINT('Ctrl Pts',(35.5729810992077,1.49984598833841,34.9678417989483));
#28750=CARTESIAN_POINT('Ctrl Pts',(35.5202511626857,1.49984512300934,34.9678418369404));
#28751=CARTESIAN_POINT('Ctrl Pts',(35.4684130151836,1.4998443492858,34.9678418773881));
#28752=CARTESIAN_POINT('Ctrl Pts',(35.3128073279263,1.49984202675329,34.9678419988026));
#28753=CARTESIAN_POINT('Ctrl Pts',(35.1652418679138,1.49984027810624,34.9678421408902));
#28754=CARTESIAN_POINT('Ctrl Pts',(35.0252627275547,1.49983493809963,34.967842254217));
#28755=CARTESIAN_POINT('Ctrl Pts',(35.0082618963838,1.49983428954192,34.9678422679808));
#28756=CARTESIAN_POINT('Ctrl Pts',(34.9913729068342,1.49983359135557,34.9678422813397));
#28757=CARTESIAN_POINT('Ctrl Pts',(34.9745948969331,1.49983283870325,34.9678422942204));
#28758=CARTESIAN_POINT('Ctrl Pts',(34.8399133402553,1.49982679696251,34.9678423976168));
#28759=CARTESIAN_POINT('Ctrl Pts',(34.7123780512931,1.49981743040037,34.9678424712592));
#28760=CARTESIAN_POINT('Ctrl Pts',(34.591404591981,1.49980840280397,34.9678425127827));
#28761=CARTESIAN_POINT('Ctrl Pts',(34.4539348326462,1.49979814417772,34.9678425599684));
#28762=CARTESIAN_POINT('Ctrl Pts',(34.3249390274086,1.49978830616204,34.9678425655798));
#28763=CARTESIAN_POINT('Ctrl Pts',(34.203631264615,1.49978156609768,34.9678425105859));
#28764=CARTESIAN_POINT('Ctrl Pts',(34.1284740534057,1.49977739023598,34.967842476514));
#28765=CARTESIAN_POINT('Ctrl Pts',(34.0562692606601,1.49977435262848,34.9678424188851));
#28766=CARTESIAN_POINT('Ctrl Pts',(33.9868395791739,1.49977272195139,34.9678423310509));
#28767=CARTESIAN_POINT('Ctrl Pts',(33.944569913827,1.49977172917462,34.9678422775764));
#28768=CARTESIAN_POINT('Ctrl Pts',(33.903332682828,1.49977122168105,34.9678422127028));
#28769=CARTESIAN_POINT('Ctrl Pts',(33.8632274501546,1.49977004757329,34.9678421281365));
#28770=CARTESIAN_POINT('Ctrl Pts',(33.8167531035319,1.49976868700542,34.9678420301403));
#28771=CARTESIAN_POINT('Ctrl Pts',(33.771789463122,1.49976648823776,34.9678419060139));
#28772=CARTESIAN_POINT('Ctrl Pts',(33.7281109635882,1.49976414064438,34.9678417565821));
#28773=CARTESIAN_POINT('Ctrl Pts',(33.6812712011832,1.49976162314223,34.9678415963351));
#28774=CARTESIAN_POINT('Ctrl Pts',(33.6359095723891,1.49975893360226,34.9678414069824));
#28775=CARTESIAN_POINT('Ctrl Pts',(33.591810246565,1.49975667024847,34.9678411881909));
#28776=CARTESIAN_POINT('Ctrl Pts',(33.5583448079856,1.4997549526683,34.9678410221577));
#28777=CARTESIAN_POINT('Ctrl Pts',(33.5256076932742,1.49975347489115,34.9678408391413));
#28778=CARTESIAN_POINT('Ctrl Pts',(33.4935243452377,1.49975241817239,34.9678406385663));
#28779=CARTESIAN_POINT('Ctrl Pts',(33.4574180647961,1.49975122895162,34.9678404128412));
#28780=CARTESIAN_POINT('Ctrl Pts',(33.4221459355308,1.49975055002974,34.9678401647559));
#28781=CARTESIAN_POINT('Ctrl Pts',(33.3878318916215,1.49974977143672,34.9678398888653));
#28782=CARTESIAN_POINT('Ctrl Pts',(33.3506903036195,1.49974892868613,34.9678395902407));
#28783=CARTESIAN_POINT('Ctrl Pts',(33.3146710708563,1.49974796966079,34.9678392590421));
#28784=CARTESIAN_POINT('Ctrl Pts',(33.2798677329257,1.49974635090117,34.967838889585));
#28785=CARTESIAN_POINT('Ctrl Pts',(33.2432742079925,1.49974464887706,34.9678385011241));
#28786=CARTESIAN_POINT('Ctrl Pts',(33.2080243245406,1.49974221953694,34.9678380703783));
#28787=CARTESIAN_POINT('Ctrl Pts',(33.1741651388244,1.49973865377071,34.9678375919209));
#28788=CARTESIAN_POINT('Ctrl Pts',(33.137063146823,1.49973474649923,34.96783706764));
#28789=CARTESIAN_POINT('Ctrl Pts',(33.1016306515623,1.49972947597288,34.9678364860775));
#28790=CARTESIAN_POINT('Ctrl Pts',(33.0678641021079,1.49972253958675,34.967835841343));
#28791=CARTESIAN_POINT('Ctrl Pts',(33.0456526984032,1.49971797687971,34.967835417241));
#28792=CARTESIAN_POINT('Ctrl Pts',(33.0241607955796,1.49971269819094,34.9678349658306));
#28793=CARTESIAN_POINT('Ctrl Pts',(33.0033754048768,1.49970666036489,34.9678344856631));
#28794=CARTESIAN_POINT('Ctrl Pts',(32.9442530209621,1.49968948625086,34.9678331198648));
#28795=CARTESIAN_POINT('Ctrl Pts',(32.8887085075052,1.49991335207053,34.9678225692835));
#28796=CARTESIAN_POINT('Ctrl Pts',(32.8362583193005,1.50027559162313,34.9678066670084));
#28797=CARTESIAN_POINT('Ctrl Pts',(32.7773090712613,1.50068271598182,34.9677887942955));
#28798=CARTESIAN_POINT('Ctrl Pts',(32.7222687069613,1.50126502290935,34.9677641462319));
#28799=CARTESIAN_POINT('Ctrl Pts',(32.6704155259709,1.50193537623736,34.9677359487883));
#28800=CARTESIAN_POINT('Ctrl Pts',(32.6144302418904,1.50265914902788,34.9677055043322));
#28801=CARTESIAN_POINT('Ctrl Pts',(32.5621602746537,1.50348644308882,34.967670888482));
#28802=CARTESIAN_POINT('Ctrl Pts',(32.512657574146,1.50436077830379,34.9676341575402));
#28803=CARTESIAN_POINT('Ctrl Pts',(32.4592478825331,1.50530412025725,34.967594527616));
#28804=CARTESIAN_POINT('Ctrl Pts',(32.4090594121698,1.50630310623457,34.9675524017484));
#28805=CARTESIAN_POINT('Ctrl Pts',(32.360858415177,1.50733170420882,34.9675086790575));
#28806=CARTESIAN_POINT('Ctrl Pts',(32.308062438401,1.50845835797427,34.9674607883018));
#28807=CARTESIAN_POINT('Ctrl Pts',(32.2576510584091,1.50962133088219,34.9674109512874));
#28808=CARTESIAN_POINT('Ctrl Pts',(32.2079531230108,1.51082436306576,34.9673589385144));
#28809=CARTESIAN_POINT('Ctrl Pts',(32.1569814991429,1.51205822727904,34.9673055927269));
#28810=CARTESIAN_POINT('Ctrl Pts',(32.1067603493739,1.51333518230827,34.9672499217566));
#28811=CARTESIAN_POINT('Ctrl Pts',(32.0554367657612,1.5146830381351,34.9671908102209));
#28812=CARTESIAN_POINT('Ctrl Pts',(32.0053752916488,1.5159977485437,34.9671331523098));
#28813=CARTESIAN_POINT('Ctrl Pts',(31.954265075229,1.51738077462808,34.9670721879268));
#28814=CARTESIAN_POINT('Ctrl Pts',(31.9003392718766,1.51886693662993,34.9670065776396));
#28815=CARTESIAN_POINT('Ctrl Pts',(31.8778362033475,1.51948710736998,34.9669791986726));
#28816=CARTESIAN_POINT('Ctrl Pts',(31.8548422465641,1.52012527669197,34.9669510097079));
#28817=CARTESIAN_POINT('Ctrl Pts',(31.8312262657831,1.52078388908931,34.9669219190816));
#28818=CARTESIAN_POINT('Ctrl Pts',(31.7273802318769,1.52367999092728,34.9667939995094));
#28819=CARTESIAN_POINT('Ctrl Pts',(31.6210019634565,1.52670831990391,34.9666588880294));
#28820=CARTESIAN_POINT('Ctrl Pts',(31.5129311113833,1.52968152042074,34.9665259706005));
#28821=CARTESIAN_POINT('Ctrl Pts',(31.4048670765162,1.53265453338541,34.9663930615562));
#28822=CARTESIAN_POINT('Ctrl Pts',(31.2951103968296,1.53557057541605,34.9662624173991));
#28823=CARTESIAN_POINT('Ctrl Pts',(31.1845493642875,1.5382305606769,34.9661438310284));
#28824=CARTESIAN_POINT('Ctrl Pts',(31.1321570104782,1.53949106707513,34.9660876356498));
#28825=CARTESIAN_POINT('Ctrl Pts',(31.0795847658975,1.54069407696176,34.9660341471942));
#28826=CARTESIAN_POINT('Ctrl Pts',(31.0269312050905,1.54181935957432,34.9659843676727));
#28827=CARTESIAN_POINT('Ctrl Pts',(30.9325025960689,1.5438374352796,34.9658950933502));
#28828=CARTESIAN_POINT('Ctrl Pts',(30.8378102330027,1.54560383003055,34.9658178028119));
#28829=CARTESIAN_POINT('Ctrl Pts',(30.7433599242841,1.54697518213503,34.9657577677723));
#28830=CARTESIAN_POINT('Ctrl Pts',(30.6608249248197,1.54817353232302,34.965705306409));
#28831=CARTESIAN_POINT('Ctrl Pts',(30.5784749808876,1.5490700665616,34.9656660234083));
#28832=CARTESIAN_POINT('Ctrl Pts',(30.4966730088978,1.54959005157024,34.9656427667437));
#28833=CARTESIAN_POINT('',(30.5,-1.44976976333441,34.9699609326822));
#28834=CARTESIAN_POINT('Origin',(30.5,0.,0.));
#28835=CARTESIAN_POINT('Ctrl Pts',(30.5054746968959,-1.44895568092928,34.9699078679682));
#28836=CARTESIAN_POINT('Ctrl Pts',(30.6033610779518,-1.44967958189436,34.9698794984549));
#28837=CARTESIAN_POINT('Ctrl Pts',(30.700368212004,-1.45097025371839,34.9698271758096));
#28838=CARTESIAN_POINT('Ctrl Pts',(30.7972404545925,-1.4526642529085,34.9697584928139));
#28839=CARTESIAN_POINT('Ctrl Pts',(30.8547901090085,-1.45367062031951,34.9697176897669));
#28840=CARTESIAN_POINT('Ctrl Pts',(30.912292559737,-1.45482036974536,34.9696710570157));
#28841=CARTESIAN_POINT('Ctrl Pts',(30.9699089182993,-1.45608616697457,34.9696198221059));
#28842=CARTESIAN_POINT('Ctrl Pts',(31.0689868417091,-1.45826285019539,34.9695317178142));
#28843=CARTESIAN_POINT('Ctrl Pts',(31.1683984987081,-1.4607818754806,34.969430038865));
#28844=CARTESIAN_POINT('Ctrl Pts',(31.2688593849665,-1.46350004288006,34.9693198609858));
#28845=CARTESIAN_POINT('Ctrl Pts',(31.3714336749603,-1.46627539258549,34.9692073652856));
#28846=CARTESIAN_POINT('Ctrl Pts',(31.47510187112,-1.4692600451563,34.9690859279462));
#28847=CARTESIAN_POINT('Ctrl Pts',(31.580677770035,-1.47230911796257,34.9689606163935));
#28848=CARTESIAN_POINT('Ctrl Pts',(31.6429045255873,-1.47410625073745,34.9688867573836));
#28849=CARTESIAN_POINT('Ctrl Pts',(31.705794981891,-1.47592578560654,34.9688115519007));
#28850=CARTESIAN_POINT('Ctrl Pts',(31.7695239145147,-1.477735460163,34.9687361665656));
#28851=CARTESIAN_POINT('Ctrl Pts',(31.8371287126756,-1.47965519548713,34.968656196446));
#28852=CARTESIAN_POINT('Ctrl Pts',(31.9000064968246,-1.48140024645571,34.9685834938761));
#28853=CARTESIAN_POINT('Ctrl Pts',(31.9586732749497,-1.48297195975084,34.968518055841));
#28854=CARTESIAN_POINT('Ctrl Pts',(32.0221536851646,-1.48467263273653,34.9684472485894));
#28855=CARTESIAN_POINT('Ctrl Pts',(32.0807039557236,-1.48617132572194,34.968384900435));
#28856=CARTESIAN_POINT('Ctrl Pts',(32.1350336259587,-1.48749336426716,34.9683299017682));
#28857=CARTESIAN_POINT('Ctrl Pts',(32.1957172192665,-1.48897001687831,34.9682684709384));
#28858=CARTESIAN_POINT('Ctrl Pts',(32.2511353794558,-1.49022726489916,34.9682161618562));
#28859=CARTESIAN_POINT('Ctrl Pts',(32.3023412619544,-1.49131215660691,34.9681708970554));
#28860=CARTESIAN_POINT('Ctrl Pts',(32.3570408527793,-1.49247106901321,34.9681225438983));
#28861=CARTESIAN_POINT('Ctrl Pts',(32.4069344452281,-1.49343418875215,34.9680821868754));
#28862=CARTESIAN_POINT('Ctrl Pts',(32.4533681563833,-1.49425570426041,34.9680474782494));
#28863=CARTESIAN_POINT('Ctrl Pts',(32.5026204371887,-1.49512708652756,34.9680106627774));
#28864=CARTESIAN_POINT('Ctrl Pts',(32.5479807574602,-1.49583975877307,34.9679801734415));
#28865=CARTESIAN_POINT('Ctrl Pts',(32.5911118987537,-1.4964428881441,34.9679539828988));
#28866=CARTESIAN_POINT('Ctrl Pts',(32.636353739081,-1.49707553272253,34.9679265106753));
#28867=CARTESIAN_POINT('Ctrl Pts',(32.6791434072979,-1.49758813414905,34.9679037453221));
#28868=CARTESIAN_POINT('Ctrl Pts',(32.721449867613,-1.4980125210104,34.9678845705529));
#28869=CARTESIAN_POINT('Ctrl Pts',(32.7634085003555,-1.49843341872493,34.9678655534314));
#28870=CARTESIAN_POINT('Ctrl Pts',(32.804892182072,-1.498767980885,34.9678500473991));
#28871=CARTESIAN_POINT('Ctrl Pts',(32.8478623301446,-1.49901713688919,34.9678384322062));
#28872=CARTESIAN_POINT('Ctrl Pts',(32.8880980033236,-1.49925043744794,34.9678275561649));
#28873=CARTESIAN_POINT('Ctrl Pts',(32.9296371024713,-1.4994093100348,34.9678200697633));
#28874=CARTESIAN_POINT('Ctrl Pts',(32.974122177228,-1.49946218333186,34.9678178555004));
#28875=CARTESIAN_POINT('Ctrl Pts',(32.9824896509787,-1.49947212859839,34.967817439006));
#28876=CARTESIAN_POINT('Ctrl Pts',(32.9909614502058,-1.49947821255296,34.9678172144271));
#28877=CARTESIAN_POINT('Ctrl Pts',(32.9995486448024,-1.49948005835563,34.967817202377));
#28878=CARTESIAN_POINT('Ctrl Pts',(33.0359672905901,-1.49948788648071,34.9678171512721));
#28879=CARTESIAN_POINT('Ctrl Pts',(33.0738131854325,-1.49949485271612,34.9678171646432));
#28880=CARTESIAN_POINT('Ctrl Pts',(33.113850191809,-1.49950094200878,34.9678174069563));
#28881=CARTESIAN_POINT('Ctrl Pts',(33.2458255353411,-1.49952101435093,34.9678182057012));
#28882=CARTESIAN_POINT('Ctrl Pts',(33.3718416807702,-1.49952700620476,34.9678186096024));
#28883=CARTESIAN_POINT('Ctrl Pts',(33.4990450828556,-1.49953291477053,34.9678189489946));
#28884=CARTESIAN_POINT('Ctrl Pts',(33.6624531387496,-1.49954050503329,34.9678193849847));
#28885=CARTESIAN_POINT('Ctrl Pts',(33.8278204637282,-1.49954795785001,34.9678197145189));
#28886=CARTESIAN_POINT('Ctrl Pts',(33.9926680821625,-1.4995605226248,34.9678203238631));
#28887=CARTESIAN_POINT('Ctrl Pts',(34.322363319031,-1.49958565217439,34.9678215425514));
#28888=CARTESIAN_POINT('Ctrl Pts',(34.649979729722,-1.49963122955625,34.9678238804795));
#28889=CARTESIAN_POINT('Ctrl Pts',(34.9787365315426,-1.49965028313962,34.9678248457331));
#28890=CARTESIAN_POINT('Ctrl Pts',(35.1431149324529,-1.49965980993131,34.9678253283599));
#28891=CARTESIAN_POINT('Ctrl Pts',(35.3077784311456,-1.49966270577337,34.9678254678181));
#28892=CARTESIAN_POINT('Ctrl Pts',(35.4723805288558,-1.4996670374846,34.9678256815692));
#28893=CARTESIAN_POINT('Ctrl Pts',(35.9661868219866,-1.49968003261829,34.9678263228224));
#28894=CARTESIAN_POINT('Ctrl Pts',(36.4594405062758,-1.49970595057452,34.9678276327118));
#28895=CARTESIAN_POINT('Ctrl Pts',(36.9526906817966,-1.49974153069046,34.9678294216938));
#28896=CARTESIAN_POINT('Ctrl Pts',(38.1015265336426,-1.4998244008339,34.9678335884367));
#28897=CARTESIAN_POINT('Ctrl Pts',(39.2503433512219,-1.49995968598758,34.9678403541474));
#28898=CARTESIAN_POINT('Ctrl Pts',(40.4000624645996,-1.4999926075592,34.9678420002216));
#28899=CARTESIAN_POINT('Ctrl Pts',(6.89999999997365,-5.65979197164529,9.46599415780712));
#28900=CARTESIAN_POINT('Ctrl Pts',(6.99168932310453,-5.60729410195165,9.49787619923353));
#28901=CARTESIAN_POINT('Ctrl Pts',(7.08405956072215,-5.55450818731572,9.52934434473076));
#28902=CARTESIAN_POINT('Ctrl Pts',(8.15473535981986,-4.94320927931174,9.88659437915724));
#28903=CARTESIAN_POINT('Ctrl Pts',(9.17052309187647,-4.34956920012189,10.1553288976265));
#28904=CARTESIAN_POINT('Ctrl Pts',(11.249912418623,-3.2475765754686,10.5681406908193));
#28905=CARTESIAN_POINT('Ctrl Pts',(12.2613271155137,-2.71507294053767,10.7096926815135));
#28906=CARTESIAN_POINT('Ctrl Pts',(14.3530613265277,-1.75089621035865,10.9182780492489));
#28907=CARTESIAN_POINT('Ctrl Pts',(15.3683896576347,-1.30024364084097,10.9736589531833));
#28908=CARTESIAN_POINT('Ctrl Pts',(17.4699484560063,-0.51160650808575,11.0479347559914));
#28909=CARTESIAN_POINT('Ctrl Pts',(18.4899441076999,-0.154966618543408,
11.0518486975415));
#28910=CARTESIAN_POINT('Ctrl Pts',(19.8459385111079,0.227738630131172,11.0525063200436));
#28911=CARTESIAN_POINT('Ctrl Pts',(20.3436052070642,0.364012293347549,11.0499443867429));
#28912=CARTESIAN_POINT('Ctrl Pts',(21.3765735172499,0.626365466004486,11.0391187302377));
#28913=CARTESIAN_POINT('Ctrl Pts',(22.1786513408684,0.80148237085404,11.0271780970656));
#28914=CARTESIAN_POINT('Ctrl Pts',(22.8524711894103,0.927590054426942,11.0190184236597));
#28915=CARTESIAN_POINT('Ctrl Pts',(23.1034772575406,0.973361071581968,11.015636270466));
#28916=CARTESIAN_POINT('Ctrl Pts',(23.6153488598143,1.06157978958535,11.0082046691873));
#28917=CARTESIAN_POINT('Ctrl Pts',(24.2640912191231,1.16309571993124,10.9980907558832));
#28918=CARTESIAN_POINT('Ctrl Pts',(24.9252112071703,1.25112898708133,10.9882975006411));
#28919=CARTESIAN_POINT('Ctrl Pts',(25.3924209938587,1.30426168416562,10.9823391891697));
#28920=CARTESIAN_POINT('Ctrl Pts',(25.6607104515486,1.332046615497,10.9792975977554));
#28921=CARTESIAN_POINT('Ctrl Pts',(25.7950739758558,1.34502686686554,10.9779150347045));
#28922=CARTESIAN_POINT('Ctrl Pts',(26.2512918422651,1.38748529291552,10.9735046934062));
#28923=CARTESIAN_POINT('Ctrl Pts',(27.3073301682004,1.45732017866833,10.9653764904263));
#28924=CARTESIAN_POINT('Ctrl Pts',(28.3319194320811,1.48237708919284,10.9609947024269));
#28925=CARTESIAN_POINT('Ctrl Pts',(29.1280123944214,1.50394716937725,10.9582092660149));
#28926=CARTESIAN_POINT('Ctrl Pts',(29.4779818455993,1.51103964894258,10.9573324846489));
#28927=CARTESIAN_POINT('Ctrl Pts',(29.9466600480359,1.51533483257754,10.9567800220405));
#28928=CARTESIAN_POINT('Ctrl Pts',(30.4585980273686,1.51632751174059,10.956656708735));
#28929=CARTESIAN_POINT('Ctrl Pts',(31.4732549878281,1.51158385370564,10.9572594965941));
#28930=CARTESIAN_POINT('Ctrl Pts',(32.3455845021632,1.4999511927851,10.95879335959));
#28931=CARTESIAN_POINT('Ctrl Pts',(33.1628510802405,1.49997453311311,10.9587933798862));
#28932=CARTESIAN_POINT('Ctrl Pts',(33.4532441810442,1.49997366471359,10.9587933789851));
#28933=CARTESIAN_POINT('Ctrl Pts',(33.7813843869345,1.49997637381128,10.9587933812939));
#28934=CARTESIAN_POINT('Ctrl Pts',(34.2755379701535,1.49997699476315,10.9587933817727));
#28935=CARTESIAN_POINT('Ctrl Pts',(34.8102302793009,1.49998326277599,10.9587933869434));
#28936=CARTESIAN_POINT('Ctrl Pts',(35.6332452367756,1.49998412101817,10.9587933876415));
#28937=CARTESIAN_POINT('Ctrl Pts',(36.2915450349079,1.49998577371297,10.9587933890033));
#28938=CARTESIAN_POINT('Ctrl Pts',(38.1020137670942,1.49998803993575,10.9587933908629));
#28939=CARTESIAN_POINT('Ctrl Pts',(39.5833333333333,1.5,10.9587934006931));
#28940=CARTESIAN_POINT('Ctrl Pts',(40.9,1.5,10.9587934006931));
#28941=CARTESIAN_POINT('Ctrl Pts',(6.65963435785827,-8.56288377493212,13.0027682689653));
#28942=CARTESIAN_POINT('Ctrl Pts',(6.7513219377677,-8.49067817166156,13.050957789036));
#28943=CARTESIAN_POINT('Ctrl Pts',(6.84370278928156,-8.41801298642698,13.0985893115687));
#28944=CARTESIAN_POINT('Ctrl Pts',(7.91483960325935,-7.57680655910808,13.6397807532085));
#28945=CARTESIAN_POINT('Ctrl Pts',(8.9325509112231,-6.75518385076231,14.0543934435321));
#28946=CARTESIAN_POINT('Ctrl Pts',(11.0192135814157,-5.22065437877307,14.7040310435559));
#28947=CARTESIAN_POINT('Ctrl Pts',(12.0340542508324,-4.4769598695545,14.9356992206141));
#28948=CARTESIAN_POINT('Ctrl Pts',(14.1407660172285,-3.1214593369057,15.2883456800052));
#28949=CARTESIAN_POINT('Ctrl Pts',(15.1616568764318,-2.48732138966201,15.3931503655329));
#28950=CARTESIAN_POINT('Ctrl Pts',(17.287218760307,-1.36959877283814,15.5446125872455));
#28951=CARTESIAN_POINT('Ctrl Pts',(18.3145546794907,-0.86490278664151,15.5707395254148));
#28952=CARTESIAN_POINT('Ctrl Pts',(19.6926214867647,-0.318801403605146,
15.5935126543779));
#28953=CARTESIAN_POINT('Ctrl Pts',(20.19452636269,-0.125373946234777,15.5977145841048));
#28954=CARTESIAN_POINT('Ctrl Pts',(21.2420076978203,0.248868189963681,15.5972978704292));
#28955=CARTESIAN_POINT('Ctrl Pts',(22.0575126096201,0.499284562147392,15.5901933457539));
#28956=CARTESIAN_POINT('Ctrl Pts',(22.7441078663834,0.679992377552245,15.5856475377419));
#28957=CARTESIAN_POINT('Ctrl Pts',(22.9980856324395,0.745267685418834,15.5834353094767));
#28958=CARTESIAN_POINT('Ctrl Pts',(23.5177883906687,0.871419538176182,15.5778337615218));
#28959=CARTESIAN_POINT('Ctrl Pts',(24.1766640555165,1.01665680544524,15.569151455817));
#28960=CARTESIAN_POINT('Ctrl Pts',(24.8496697365589,1.14287321247013,15.560128822227));
#28961=CARTESIAN_POINT('Ctrl Pts',(25.3259254544069,1.2191404135396,15.554601684436));
#28962=CARTESIAN_POINT('Ctrl Pts',(25.5996882691236,1.2590574298324,15.5518109321211));
#28963=CARTESIAN_POINT('Ctrl Pts',(25.7368188560809,1.27770917936971,15.550561003587));
#28964=CARTESIAN_POINT('Ctrl Pts',(26.2030586507879,1.33878235986071,15.5466206431081));
#28965=CARTESIAN_POINT('Ctrl Pts',(27.2845562696213,1.43928616936987,15.5388831179539));
#28966=CARTESIAN_POINT('Ctrl Pts',(28.3146233763975,1.47473229777557,15.534108117874));
#28967=CARTESIAN_POINT('Ctrl Pts',(29.1121433593266,1.5053783917148,15.5313810124223));
#28968=CARTESIAN_POINT('Ctrl Pts',(29.4693616319656,1.51558516408219,15.5305221749293));
#28969=CARTESIAN_POINT('Ctrl Pts',(29.9425518103672,1.5216968643791,15.5299808253862));
#28970=CARTESIAN_POINT('Ctrl Pts',(30.4595136734855,1.52312339822457,15.5298599056894));
#28971=CARTESIAN_POINT('Ctrl Pts',(31.4800666545032,1.51634797661239,15.5304501241615));
#28972=CARTESIAN_POINT('Ctrl Pts',(32.3507119180564,1.4999128955352,15.5319509809364));
#28973=CARTESIAN_POINT('Ctrl Pts',(33.1621363777215,1.49995461572564,15.5319505779396));
#28974=CARTESIAN_POINT('Ctrl Pts',(33.4535196029878,1.49995304854269,15.5319505880019));
#28975=CARTESIAN_POINT('Ctrl Pts',(33.7812306484551,1.49995788616631,15.5319505396377));
#28976=CARTESIAN_POINT('Ctrl Pts',(34.2755524327802,1.49995898984267,15.531950526851));
#28977=CARTESIAN_POINT('Ctrl Pts',(34.8101578274898,1.49997016508529,15.5319504091692));
#28978=CARTESIAN_POINT('Ctrl Pts',(35.6332135248365,1.49997169422773,15.5319503927198));
#28979=CARTESIAN_POINT('Ctrl Pts',(36.2914988048216,1.49997464065555,15.5319503616369));
#28980=CARTESIAN_POINT('Ctrl Pts',(38.1019885414694,1.49997868009126,15.5319503187541));
#28981=CARTESIAN_POINT('Ctrl Pts',(39.5833333333333,1.5,15.5319500929849));
#28982=CARTESIAN_POINT('Ctrl Pts',(40.9,1.5,15.5319500929849));
#28983=CARTESIAN_POINT('Ctrl Pts',(6.47503677058814,-13.6264850125633,19.2049631177014));
#28984=CARTESIAN_POINT('Ctrl Pts',(6.56582707216344,-13.5206117629928,19.2807931407427));
#28985=CARTESIAN_POINT('Ctrl Pts',(6.65722187862393,-13.4141026801341,19.3557456396964));
#28986=CARTESIAN_POINT('Ctrl Pts',(7.71979853459931,-12.1774082172639,20.2113974185276));
#28987=CARTESIAN_POINT('Ctrl Pts',(8.72714740265586,-10.9649265084515,20.876585861408));
#28988=CARTESIAN_POINT('Ctrl Pts',(10.792252425961,-8.69413764846818,21.9312131301472));
#28989=CARTESIAN_POINT('Ctrl Pts',(11.8008983729842,-7.58577239973431,22.3203974544121));
#28990=CARTESIAN_POINT('Ctrl Pts',(13.892634394048,-5.56042793834188,22.9231109701401));
#28991=CARTESIAN_POINT('Ctrl Pts',(14.910936596525,-4.60683703173286,23.1162450123325));
#28992=CARTESIAN_POINT('Ctrl Pts',(17.0374816014601,-2.91606182242837,23.4053158267904));
#28993=CARTESIAN_POINT('Ctrl Pts',(18.0678529336714,-2.15006970557795,23.4724397837998));
#28994=CARTESIAN_POINT('Ctrl Pts',(19.4632774216583,-1.31129970902877,23.5361137002685));
#28995=CARTESIAN_POINT('Ctrl Pts',(19.9690853949367,-1.01646669656859,23.5527456051548));
#28996=CARTESIAN_POINT('Ctrl Pts',(21.0306109698709,-0.441678056412671,
23.5717577824589));
#28997=CARTESIAN_POINT('Ctrl Pts',(21.8626014988188,-0.054300344268142,
23.5739085372705));
#28998=CARTESIAN_POINT('Ctrl Pts',(22.5665651705188,0.226484889079844,23.576178914363));
#28999=CARTESIAN_POINT('Ctrl Pts',(22.8246411038756,0.326902916553466,23.5761448043361));
#29000=CARTESIAN_POINT('Ctrl Pts',(23.3554232774669,0.522054743089693,23.5740054132278));
#29001=CARTESIAN_POINT('Ctrl Pts',(24.0293769285439,0.747005858788649,23.5680817805141));
#29002=CARTESIAN_POINT('Ctrl Pts',(24.7209631427047,0.943393581394331,23.560586503548));
#29003=CARTESIAN_POINT('Ctrl Pts',(25.2118242719342,1.06233480615607,23.5558940963915));
#29004=CARTESIAN_POINT('Ctrl Pts',(25.4945546545947,1.12470144437592,23.5535795021665));
#29005=CARTESIAN_POINT('Ctrl Pts',(25.6362544160062,1.15385183559377,23.5525764277763));
#29006=CARTESIAN_POINT('Ctrl Pts',(26.1191683853685,1.24953281052836,23.5495095529483));
#29007=CARTESIAN_POINT('Ctrl Pts',(27.244410780189,1.40715534997208,23.5425023713064));
#29008=CARTESIAN_POINT('Ctrl Pts',(28.2843056152442,1.46065929315376,23.5370396227258));
#29009=CARTESIAN_POINT('Ctrl Pts',(29.0843244121809,1.50737208683505,23.5344215873996));
#29010=CARTESIAN_POINT('Ctrl Pts',(29.4542021761287,1.52336782189617,23.5335942286398));
#29011=CARTESIAN_POINT('Ctrl Pts',(29.9352997409898,1.53271512054377,23.5330734925559));
#29012=CARTESIAN_POINT('Ctrl Pts',(30.4610555884278,1.5349453613852,23.532957187389));
#29013=CARTESIAN_POINT('Ctrl Pts',(31.4919316519535,1.52450364515754,23.5335262680548));
#29014=CARTESIAN_POINT('Ctrl Pts',(32.3596576160514,1.49979324124413,23.5349731541844));
#29015=CARTESIAN_POINT('Ctrl Pts',(33.1608710165812,1.49989213988255,23.5349736853906));
#29016=CARTESIAN_POINT('Ctrl Pts',(33.4539865796869,1.49988845489238,23.5349736699323));
#29017=CARTESIAN_POINT('Ctrl Pts',(33.780948091659,1.49989993226727,23.5349737329761));
#29018=CARTESIAN_POINT('Ctrl Pts',(34.275564602361,1.49990256114204,23.5349737489117));
#29019=CARTESIAN_POINT('Ctrl Pts',(34.8100214672069,1.49992910993535,23.5349738998239));
#29020=CARTESIAN_POINT('Ctrl Pts',(35.6331489543767,1.49993274473985,23.5349739207807));
#29021=CARTESIAN_POINT('Ctrl Pts',(36.2914097700016,1.4999397448351,23.5349739606187));
#29022=CARTESIAN_POINT('Ctrl Pts',(38.1019375614968,1.49994934328327,23.5349740154737));
#29023=CARTESIAN_POINT('Ctrl Pts',(39.5833333333333,1.5,23.5349743044955));
#29024=CARTESIAN_POINT('Ctrl Pts',(40.9,1.5,23.5349743044955));
#29025=CARTESIAN_POINT('Ctrl Pts',(6.39840282685635,-18.5950148818,25.4797798158266));
#29026=CARTESIAN_POINT('Ctrl Pts',(6.48879582230594,-18.455456538043,25.5825069307027));
#29027=CARTESIAN_POINT('Ctrl Pts',(6.57973810483189,-18.3151558806717,25.684006582131));
#29028=CARTESIAN_POINT('Ctrl Pts',(7.63881202209716,-16.6821095714367,26.8457843562122));
#29029=CARTESIAN_POINT('Ctrl Pts',(8.64206536867565,-15.0805562774161,27.7524045864227));
#29030=CARTESIAN_POINT('Ctrl Pts',(10.6943835463645,-12.08639394536,29.194220471563));
#29031=CARTESIAN_POINT('Ctrl Pts',(11.6986850371145,-10.6188960618635,29.7340826089764));
#29032=CARTESIAN_POINT('Ctrl Pts',(13.7736723466472,-7.9480571508383,30.5724457120527));
#29033=CARTESIAN_POINT('Ctrl Pts',(14.7865355152845,-6.68379951334874,30.8496813329458));
#29034=CARTESIAN_POINT('Ctrl Pts',(16.895644387614,-4.44867953439714,31.2681094727719));
#29035=CARTESIAN_POINT('Ctrl Pts',(17.921113585793,-3.42955614780409,31.3748718553479));
#29036=CARTESIAN_POINT('Ctrl Pts',(19.3111115725317,-2.31180057560694,31.4778602005301));
#29037=CARTESIAN_POINT('Ctrl Pts',(19.8164097330209,-1.91755167896535,31.5068304778962));
#29038=CARTESIAN_POINT('Ctrl Pts',(20.8772665291465,-1.14804732053491,31.5450009606978));
#29039=CARTESIAN_POINT('Ctrl Pts',(21.7126526899651,-0.625757760628936,
31.5565752055434));
#29040=CARTESIAN_POINT('Ctrl Pts',(22.4233939916368,-0.244774266221903,
31.5658469864011));
#29041=CARTESIAN_POINT('Ctrl Pts',(22.68321700305,-0.109074102068984,31.568070163829));
#29042=CARTESIAN_POINT('Ctrl Pts',(23.2191843843282,0.155714853804436,31.5695528321153));
#29043=CARTESIAN_POINT('Ctrl Pts',(23.9014490792895,0.461901703286709,31.5665856540486));
#29044=CARTESIAN_POINT('Ctrl Pts',(24.6052033552109,0.730987709817267,31.5607844376464));
#29045=CARTESIAN_POINT('Ctrl Pts',(25.1069219885717,0.894795181267931,31.5570192016244));
#29046=CARTESIAN_POINT('Ctrl Pts',(25.3966703145091,0.980957842597309,31.5552253028176));
#29047=CARTESIAN_POINT('Ctrl Pts',(25.5420691491796,1.02128571697646,31.5544886793522));
#29048=CARTESIAN_POINT('Ctrl Pts',(26.0386675456483,1.15405115562807,31.5523567719375));
#29049=CARTESIAN_POINT('Ctrl Pts',(27.2041996425261,1.37405103438869,31.5461367082151));
#29050=CARTESIAN_POINT('Ctrl Pts',(28.254481539011,1.44553527377015,31.5399727189289));
#29051=CARTESIAN_POINT('Ctrl Pts',(29.0567817440806,1.50856328668891,31.5374655658645));
#29052=CARTESIAN_POINT('Ctrl Pts',(29.4392037716731,1.53093305020556,31.5366692491296));
#29053=CARTESIAN_POINT('Ctrl Pts',(29.9281985709061,1.54360558359609,31.536168682902));
#29054=CARTESIAN_POINT('Ctrl Pts',(30.4627354290944,1.54671304059522,31.5360567738141));
#29055=CARTESIAN_POINT('Ctrl Pts',(31.5039222132188,1.53240580330097,31.5366047697957));
#29056=CARTESIAN_POINT('Ctrl Pts',(32.3686614831274,1.49961223537188,31.5379963364647));
#29057=CARTESIAN_POINT('Ctrl Pts',(33.1596379899179,1.49979803313559,31.5379973429874));
#29058=CARTESIAN_POINT('Ctrl Pts',(33.4544864001145,1.49979103760184,31.5379973136915));
#29059=CARTESIAN_POINT('Ctrl Pts',(33.7806952343975,1.49981257637976,31.5379974331442));
#29060=CARTESIAN_POINT('Ctrl Pts',(34.2756055948936,1.49981748473541,31.5379974633363));
#29061=CARTESIAN_POINT('Ctrl Pts',(34.8099061252942,1.49986722177693,31.5379977492716));
#29062=CARTESIAN_POINT('Ctrl Pts',(35.6331043028646,1.49987402634112,31.5379977889784));
#29063=CARTESIAN_POINT('Ctrl Pts',(36.2913385913736,1.49988713966987,31.5379978644599));
#29064=CARTESIAN_POINT('Ctrl Pts',(38.1019015852784,1.49990511666357,31.537997968394));
#29065=CARTESIAN_POINT('Ctrl Pts',(39.5833333333333,1.5,31.5379985160061));
#29066=CARTESIAN_POINT('Ctrl Pts',(40.9,1.5,31.5379985160061));
#29067=CARTESIAN_POINT('Ctrl Pts',(6.37427268165564,-20.7176664141567,28.1741189428499));
#29068=CARTESIAN_POINT('Ctrl Pts',(6.46448755772839,-20.5636424771022,28.2883460540946));
#29069=CARTESIAN_POINT('Ctrl Pts',(6.55522687426754,-20.4088293925213,28.4011972468989));
#29070=CARTESIAN_POINT('Ctrl Pts',(7.61282240204205,-18.6056139772311,29.693787896276));
#29071=CARTESIAN_POINT('Ctrl Pts',(8.61454082730176,-16.8370699794085,30.703424507615));
#29072=CARTESIAN_POINT('Ctrl Pts',(10.6618274824665,-13.5325068155167,32.3104201819496));
#29073=CARTESIAN_POINT('Ctrl Pts',(11.6645377987076,-11.9110180488694,32.9144254040795));
#29074=CARTESIAN_POINT('Ctrl Pts',(13.7331445959134,-8.96386257277558,33.8529424117878));
#29075=CARTESIAN_POINT('Ctrl Pts',(14.7439932704909,-7.56674532731094,34.1658004948675));
#29076=CARTESIAN_POINT('Ctrl Pts',(16.8461035490385,-5.10012840374637,34.6388264066738));
#29077=CARTESIAN_POINT('Ctrl Pts',(17.8695058124616,-3.97333364734334,34.7622645166785));
#29078=CARTESIAN_POINT('Ctrl Pts',(19.2561174443541,-2.73821070416468,34.8817349492475));
#29079=CARTESIAN_POINT('Ctrl Pts',(19.7609345646798,-2.30176586395498,34.9159214541564));
#29080=CARTESIAN_POINT('Ctrl Pts',(20.8205141053453,-1.45015687002429,34.9621410370326));
#29081=CARTESIAN_POINT('Ctrl Pts',(21.6560023791939,-0.871078443386998,
34.9776907709078));
#29082=CARTESIAN_POINT('Ctrl Pts',(22.3682688599883,-0.447778285927138,
34.989939594886));
#29083=CARTESIAN_POINT('Ctrl Pts',(22.6285200842947,-0.297086276283264,
34.9931281975259));
#29084=CARTESIAN_POINT('Ctrl Pts',(23.1658603614091,-0.00273379297028158,
34.9961605697035));
#29085=CARTESIAN_POINT('Ctrl Pts',(23.8505975407037,0.338068372298849,34.9944676948756));
#29086=CARTESIAN_POINT('Ctrl Pts',(24.5583968797874,0.638319272935674,34.9894056975888));
#29087=CARTESIAN_POINT('Ctrl Pts',(25.0640148551739,0.821498314632839,34.9860476379143));
#29088=CARTESIAN_POINT('Ctrl Pts',(25.3563632502514,0.917977493583091,34.9844821378475));
#29089=CARTESIAN_POINT('Ctrl Pts',(25.503160007456,0.963163948801064,34.9838621425449));
#29090=CARTESIAN_POINT('Ctrl Pts',(26.0049713545738,1.11209382847184,34.982139121313));
#29091=CARTESIAN_POINT('Ctrl Pts',(27.1869304722337,1.35965020681436,34.9762666166019));
#29092=CARTESIAN_POINT('Ctrl Pts',(28.2418054197051,1.43886806122646,34.9698003983093));
#29093=CARTESIAN_POINT('Ctrl Pts',(29.0450356043991,1.5089275405599,34.9673414359535));
#29094=CARTESIAN_POINT('Ctrl Pts',(29.4328041419752,1.53413528152413,34.9665583691038));
#29095=CARTESIAN_POINT('Ctrl Pts',(29.9251825362975,1.54824951859995,34.9660664512209));
#29096=CARTESIAN_POINT('Ctrl Pts',(30.4634799414205,1.55174636239756,34.9659564211645));
#29097=CARTESIAN_POINT('Ctrl Pts',(31.5090833787051,1.53574598606795,34.9664954410524));
#29098=CARTESIAN_POINT('Ctrl Pts',(32.3725304400172,1.49952340891733,34.9678633362529));
#29099=CARTESIAN_POINT('Ctrl Pts',(33.1591152593399,1.49975189997366,34.9678645826042));
#29100=CARTESIAN_POINT('Ctrl Pts',(33.4547063903441,1.49974326694616,34.9678645463389));
#29101=CARTESIAN_POINT('Ctrl Pts',(33.7805921021893,1.49976974530861,34.9678646942577));
#29102=CARTESIAN_POINT('Ctrl Pts',(34.2756282408745,1.49977576894615,34.9678647316484));
#29103=CARTESIAN_POINT('Ctrl Pts',(34.8098603973427,1.49983687714898,34.967865085736));
#29104=CARTESIAN_POINT('Ctrl Pts',(35.6330886763766,1.49984523535833,34.9678651349076));
#29105=CARTESIAN_POINT('Ctrl Pts',(36.2913112329655,1.49986134640235,34.9678652283802));
#29106=CARTESIAN_POINT('Ctrl Pts',(38.1018888107018,1.49988343135295,34.9678653570876));
#29107=CARTESIAN_POINT('Ctrl Pts',(39.5833333333333,1.5,34.9678660352249));
#29108=CARTESIAN_POINT('Ctrl Pts',(40.9,1.5,34.9678660352249));
#29109=CARTESIAN_POINT('',(40.9,1.50000000000002,32.9658914637539));
#29110=CARTESIAN_POINT('Ctrl Pts',(40.9,1.50000000000002,32.9658914637539));
#29111=CARTESIAN_POINT('Ctrl Pts',(40.9,1.50000000000002,33.466386268912));
#29112=CARTESIAN_POINT('Ctrl Pts',(40.9,1.50000000000002,33.9668810740701));
#29113=CARTESIAN_POINT('Ctrl Pts',(40.9,1.50000000000002,34.4673758792282));
#29114=CARTESIAN_POINT('',(38.,1.50000000000001,32.9658914637539));
#29115=CARTESIAN_POINT('Ctrl Pts',(38.,1.5,32.9658914637539));
#29116=CARTESIAN_POINT('Ctrl Pts',(38.9666666666667,1.5,32.9658914637539));
#29117=CARTESIAN_POINT('Ctrl Pts',(39.9333333333333,1.5,32.9658914637539));
#29118=CARTESIAN_POINT('Ctrl Pts',(40.9,1.5,32.9658914637539));
#29119=CARTESIAN_POINT('Ctrl Pts',(37.4997714574611,1.49990106437153,32.3652585803353));
#29120=CARTESIAN_POINT('Ctrl Pts',(37.6667294826965,1.4999047077905,32.5658056765355));
#29121=CARTESIAN_POINT('Ctrl Pts',(37.8334450600885,1.49990923999261,32.7660568372681));
#29122=CARTESIAN_POINT('Ctrl Pts',(37.9998166694663,1.49991439209149,32.9658909678229));
#29123=CARTESIAN_POINT('',(6.9,-16.9192021366758,24.7737885487526));
#29124=CARTESIAN_POINT('Ctrl Pts',(6.9,-16.9192021366758,24.7737885487526));
#29125=CARTESIAN_POINT('Ctrl Pts',(6.9,-15.3881766950258,22.6454446228759));
#29126=CARTESIAN_POINT('Ctrl Pts',(6.90000000000115,-13.8353835251886,20.4978726403359));
#29127=CARTESIAN_POINT('Ctrl Pts',(6.90000000000115,-10.3082122779765,15.662481608859));
#29128=CARTESIAN_POINT('Ctrl Pts',(6.9,-7.95935811114668,12.4764228571341));
#29129=CARTESIAN_POINT('Ctrl Pts',(6.9,-5.6597919716369,9.46599415782505));
#29130=CARTESIAN_POINT('',(22.9245129145126,1.94538850028551E-15,31.7706052331164));
#29131=CARTESIAN_POINT('Ctrl Pts',(22.9245129145126,6.11247215341707E-15,
31.7706052331164));
#29132=CARTESIAN_POINT('Ctrl Pts',(22.7202811020963,-0.0979233563002629,
31.7014549124251));
#29133=CARTESIAN_POINT('Ctrl Pts',(22.5089075447093,-0.203440182623871,
31.6320805544326));
#29134=CARTESIAN_POINT('Ctrl Pts',(22.2913349439917,-0.316637134194165,
31.5632247707622));
#29135=CARTESIAN_POINT('Ctrl Pts',(21.4451770585292,-0.756869465221198,
31.2954389184983));
#29136=CARTESIAN_POINT('Ctrl Pts',(20.5220951556666,-1.35418571023233,31.0475106147151));
#29137=CARTESIAN_POINT('Ctrl Pts',(19.7671428819537,-1.89915402350715,30.8612920963157));
#29138=CARTESIAN_POINT('Ctrl Pts',(19.519477305839,-2.07793339270839,30.8002022522972));
#29139=CARTESIAN_POINT('Ctrl Pts',(19.286571638609,-2.25204835959326,30.7444068279677));
#29140=CARTESIAN_POINT('Ctrl Pts',(19.0728538401323,-2.41532203906683,30.6939488833522));
#29141=CARTESIAN_POINT('Ctrl Pts',(18.7028555998035,-2.69798906318815,30.6065937315987));
#29142=CARTESIAN_POINT('Ctrl Pts',(18.4144703596235,-2.93373938287723,30.5399660639319));
#29143=CARTESIAN_POINT('Ctrl Pts',(18.0642874871537,-3.23398234070002,30.4582462938821));
#29144=CARTESIAN_POINT('Ctrl Pts',(17.442092711672,-3.76744532366929,30.3130489756353));
#29145=CARTESIAN_POINT('Ctrl Pts',(16.7224564418218,-4.43872907330236,30.1446863488622));
#29146=CARTESIAN_POINT('Ctrl Pts',(15.9202806616111,-5.24401550821529,29.9321297384067));
#29147=CARTESIAN_POINT('Ctrl Pts',(15.4090529834516,-5.75722561070139,29.7966671314304));
#29148=CARTESIAN_POINT('Ctrl Pts',(14.8739602945711,-6.33424649579702,29.6418940055914));
#29149=CARTESIAN_POINT('Ctrl Pts',(14.3169794331149,-6.96996102647284,29.455763484612));
#29150=CARTESIAN_POINT('Ctrl Pts',(13.8864206762832,-7.4613826837844,29.3118803976567));
#29151=CARTESIAN_POINT('Ctrl Pts',(13.3867890027802,-8.05270459512032,29.1311705407938));
#29152=CARTESIAN_POINT('Ctrl Pts',(12.8146824059514,-8.75043091662868,28.8915984033895));
#29153=CARTESIAN_POINT('Ctrl Pts',(12.2526665517595,-9.43585083093891,28.6562518085588));
#29154=CARTESIAN_POINT('Ctrl Pts',(11.6379478462804,-10.231366276768,28.3625845909803));
#29155=CARTESIAN_POINT('Ctrl Pts',(10.9739250490308,-11.1267230319105,27.981021293096));
#29156=CARTESIAN_POINT('Ctrl Pts',(10.5683455447963,-11.6735993596027,27.747965660321));
#29157=CARTESIAN_POINT('Ctrl Pts',(10.1437415406956,-12.2581093618546,27.4801235315866));
#29158=CARTESIAN_POINT('Ctrl Pts',(9.74137929176525,-12.8142541611144,27.2046666925187));
#29159=CARTESIAN_POINT('Ctrl Pts',(8.72285779294234,-14.2220538143138,26.5073877769786));
#29160=CARTESIAN_POINT('Ctrl Pts',(7.81323138778195,-15.580948814124,25.7100913255874));
#29161=CARTESIAN_POINT('Ctrl Pts',(6.9,-16.9192021366758,24.7737885487526));
#29162=CARTESIAN_POINT('Ctrl Pts',(30.5,1.55029606206997,34.9656486014478));
#29163=CARTESIAN_POINT('Ctrl Pts',(29.9560179420817,1.55343104498103,34.7222276068062));
#29164=CARTESIAN_POINT('Ctrl Pts',(29.4152668325132,1.54030953139106,34.4790656554127));
#29165=CARTESIAN_POINT('Ctrl Pts',(28.8740459957565,1.49470250846617,34.2361296888632));
#29166=CARTESIAN_POINT('Ctrl Pts',(28.3535277923439,1.4508400330705,34.0024864433252));
#29167=CARTESIAN_POINT('Ctrl Pts',(27.8179515912466,1.40923473841146,33.7608540997398));
#29168=CARTESIAN_POINT('Ctrl Pts',(27.2695051149491,1.33972398862116,33.5168388499063));
#29169=CARTESIAN_POINT('Ctrl Pts',(26.9554553615883,1.29992095446743,33.3771115796287));
#29170=CARTESIAN_POINT('Ctrl Pts',(26.6378099296971,1.25106463707208,33.2369493090937));
#29171=CARTESIAN_POINT('Ctrl Pts',(26.3179304017917,1.18777049128279,33.0983258448229));
#29172=CARTESIAN_POINT('Ctrl Pts',(26.1078196745982,1.14619615520081,33.0072719500184));
#29173=CARTESIAN_POINT('Ctrl Pts',(25.8967402232745,1.09839525532296,32.9168907470981));
#29174=CARTESIAN_POINT('Ctrl Pts',(25.6850706236774,1.04282885388104,32.8277596053404));
#29175=CARTESIAN_POINT('Ctrl Pts',(25.6562210027417,1.03525540156946,32.8156114288513));
#29176=CARTESIAN_POINT('Ctrl Pts',(25.6277737638215,1.0276506122434,32.8036595933923));
#29177=CARTESIAN_POINT('Ctrl Pts',(25.5983858063598,1.01964325944536,32.7913423709803));
#29178=CARTESIAN_POINT('Ctrl Pts',(25.1249357452756,0.890642063078173,32.5929076988546));
#29179=CARTESIAN_POINT('Ctrl Pts',(24.1510084067019,0.588069770626604,32.1858811669087));
#29180=CARTESIAN_POINT('Ctrl Pts',(22.9245129145126,6.11247215341707E-15,
31.7706052331164));
#29181=CARTESIAN_POINT('Origin',(40.65,0.,0.));
#29182=CARTESIAN_POINT('',(40.4,-18.7829592905825,29.5330398077868));
#29183=CARTESIAN_POINT('',(40.9,-18.5327260452907,29.0996231131986));
#29184=CARTESIAN_POINT('Ctrl Pts',(40.4,-18.7829592905825,29.5330398077868));
#29185=CARTESIAN_POINT('Ctrl Pts',(40.5666590136477,-18.6995531510789,29.3885761365034));
#29186=CARTESIAN_POINT('Ctrl Pts',(40.733343045036,-18.6161333949886,29.2440888806));
#29187=CARTESIAN_POINT('Ctrl Pts',(40.9,-18.5327260452907,29.0996231131986));
#29188=CARTESIAN_POINT('',(40.9,-15.9346498339374,30.5996231131986));
#29189=CARTESIAN_POINT('Origin',(40.9,0.,0.));
#29190=CARTESIAN_POINT('',(40.4,-16.1848830792292,31.0330398077868));
#29191=CARTESIAN_POINT('Ctrl Pts',(40.9,-15.9346498339374,30.5996231131986));
#29192=CARTESIAN_POINT('Ctrl Pts',(40.7333430442473,-16.0180571840301,30.7440888812837));
#29193=CARTESIAN_POINT('Ctrl Pts',(40.5666590122953,-16.1014769404025,30.8885761376758));
#29194=CARTESIAN_POINT('Ctrl Pts',(40.4,-16.1848830792292,31.0330398077868));
#29195=CARTESIAN_POINT('Origin',(40.4,0.,0.));
#29196=CARTESIAN_POINT('Origin',(35.7,0.,0.));
#29197=CARTESIAN_POINT('',(30.5,-16.1402285275843,31.0562879796886));
#29198=CARTESIAN_POINT('Ctrl Pts',(40.3999012894849,-16.1848928782182,31.0330346270951));
#29199=CARTESIAN_POINT('Ctrl Pts',(39.2494626810401,-16.1849362443212,31.0330116996609));
#29200=CARTESIAN_POINT('Ctrl Pts',(38.0976708836828,-16.1851115327779,31.0329190263647));
#29201=CARTESIAN_POINT('Ctrl Pts',(36.9467340384723,-16.1851746119074,31.0328856894588));
#29202=CARTESIAN_POINT('Ctrl Pts',(36.745427730736,-16.1851856448557,31.032879858618));
#29203=CARTESIAN_POINT('Ctrl Pts',(36.5441475779313,-16.1851932450653,31.0328758430125));
#29204=CARTESIAN_POINT('Ctrl Pts',(36.3429119519248,-16.1852000001162,31.0328722727086));
#29205=CARTESIAN_POINT('Ctrl Pts',(36.2102758775794,-16.1852044524265,31.0328699194916));
#29206=CARTESIAN_POINT('Ctrl Pts',(36.0822774296293,-16.1852084224022,31.0328678560427));
#29207=CARTESIAN_POINT('Ctrl Pts',(35.9587202262686,-16.1852125810274,31.0328657167445));
#29208=CARTESIAN_POINT('Ctrl Pts',(35.7925662245336,-16.1852181733537,31.0328628399153));
#29209=CARTESIAN_POINT('Ctrl Pts',(35.6344388155489,-16.1852241162452,31.0328598211429));
#29210=CARTESIAN_POINT('Ctrl Pts',(35.4837714463452,-16.1852312078526,31.032856216152));
#29211=CARTESIAN_POINT('Ctrl Pts',(35.3175474553577,-16.1852390316786,31.0328522389407));
#29212=CARTESIAN_POINT('Ctrl Pts',(35.1604041224813,-16.1852482463284,31.0328475520712));
#29213=CARTESIAN_POINT('Ctrl Pts',(35.0116427948686,-16.1852592402397,31.0328419178902));
#29214=CARTESIAN_POINT('Ctrl Pts',(34.997927209115,-16.1852602538629,31.0328413984267));
#29215=CARTESIAN_POINT('Ctrl Pts',(34.9842829110374,-16.1852612822246,31.0328408711132));
#29216=CARTESIAN_POINT('Ctrl Pts',(34.9707093736272,-16.1852623254084,31.0328403358797));
#29217=CARTESIAN_POINT('Ctrl Pts',(34.8522491799023,-16.1852714295754,31.0328356647415));
#29218=CARTESIAN_POINT('Ctrl Pts',(34.7391835006529,-16.1852816068676,31.0328304196803));
#29219=CARTESIAN_POINT('Ctrl Pts',(34.6312849042887,-16.1852915612823,31.0328252639047));
#29220=CARTESIAN_POINT('Ctrl Pts',(34.5096795260853,-16.1853027802453,31.0328194531708));
#29221=CARTESIAN_POINT('Ctrl Pts',(34.394637058133,-16.1853137193614,31.0328137541413));
#29222=CARTESIAN_POINT('Ctrl Pts',(34.2857585821194,-16.1853233495613,31.0328086821746));
#29223=CARTESIAN_POINT('Ctrl Pts',(34.1786801908155,-16.1853328205454,31.0328036940625));
#29224=CARTESIAN_POINT('Ctrl Pts',(34.0775620514829,-16.185341043166,31.0327993031901));
#29225=CARTESIAN_POINT('Ctrl Pts',(33.9819758246427,-16.1853475980775,31.0327957057953));
#29226=CARTESIAN_POINT('Ctrl Pts',(33.9184449689727,-16.1853519547631,31.0327933148067));
#29227=CARTESIAN_POINT('Ctrl Pts',(33.8573517602305,-16.1853555977387,31.0327912624254));
#29228=CARTESIAN_POINT('Ctrl Pts',(33.7984399511826,-16.1853587887284,31.0327894081824));
#29229=CARTESIAN_POINT('Ctrl Pts',(33.7337970612213,-16.1853622901453,31.0327873735543));
#29230=CARTESIAN_POINT('Ctrl Pts',(33.6717809742681,-16.1853652470742,31.0327855776265));
#29231=CARTESIAN_POINT('Ctrl Pts',(33.6121191806454,-16.1853678991828,31.0327838881567));
#29232=CARTESIAN_POINT('Ctrl Pts',(33.5695978710648,-16.1853697893561,31.0327826840617));
#29233=CARTESIAN_POINT('Ctrl Pts',(33.5282738752657,-16.185371522363,31.0327815352149));
#29234=CARTESIAN_POINT('Ctrl Pts',(33.4880643388298,-16.1853731585247,31.032780407062));
#29235=CARTESIAN_POINT('Ctrl Pts',(33.4508270573206,-16.1853746737428,31.0327793623013));
#29236=CARTESIAN_POINT('Ctrl Pts',(33.4145509216558,-16.1853761126592,31.0327783314862));
#29237=CARTESIAN_POINT('Ctrl Pts',(33.3793439789548,-16.1853777420673,31.0327771639657));
#29238=CARTESIAN_POINT('Ctrl Pts',(33.3411337035362,-16.1853795104722,31.0327758968498));
#29239=CARTESIAN_POINT('Ctrl Pts',(33.3041826660689,-16.1853815029502,31.0327744688781));
#29240=CARTESIAN_POINT('Ctrl Pts',(33.2685652776782,-16.1853839484229,31.0327727495066));
#29241=CARTESIAN_POINT('Ctrl Pts',(33.231009447455,-16.1853865269881,31.0327709365599));
#29242=CARTESIAN_POINT('Ctrl Pts',(33.1949357943681,-16.185389608116,31.0327688002293));
#29243=CARTESIAN_POINT('Ctrl Pts',(33.1603699172393,-16.1853933524012,31.0327662471215));
#29244=CARTESIAN_POINT('Ctrl Pts',(33.122371567942,-16.1853974685027,31.0327634404841));
#29245=CARTESIAN_POINT('Ctrl Pts',(33.0861949166479,-16.1854023852333,31.0327601306123));
#29246=CARTESIAN_POINT('Ctrl Pts',(33.0518089354078,-16.1854082033113,31.0327562557942));
#29247=CARTESIAN_POINT('Ctrl Pts',(33.0341030813062,-16.1854111991264,31.0327542605926));
#29248=CARTESIAN_POINT('Ctrl Pts',(33.0168710360023,-16.1854144322605,31.032752116523));
#29249=CARTESIAN_POINT('Ctrl Pts',(33.0001033802535,-16.1854179076007,31.0327498200704));
#29250=CARTESIAN_POINT('Ctrl Pts',(32.9420348133412,-16.1854299431544,31.0327418671573));
#29251=CARTESIAN_POINT('Ctrl Pts',(32.8874145324497,-16.1852296143114,31.0328461364757));
#29252=CARTESIAN_POINT('Ctrl Pts',(32.8357863520582,-16.1849068811705,31.0330149777623));
#29253=CARTESIAN_POINT('Ctrl Pts',(32.7779739682632,-16.1845454899291,31.0332040434467));
#29254=CARTESIAN_POINT('Ctrl Pts',(32.7239136589685,-16.1840302574575,31.0334742654593));
#29255=CARTESIAN_POINT('Ctrl Pts',(32.6729278684755,-16.1834371021678,31.033785409572));
#29256=CARTESIAN_POINT('Ctrl Pts',(32.6180801336262,-16.1827990180322,31.0341201214522));
#29257=CARTESIAN_POINT('Ctrl Pts',(32.5667902508432,-16.1820699950122,31.0345025939175));
#29258=CARTESIAN_POINT('Ctrl Pts',(32.5181731636797,-16.1812992842338,31.034906696383));
#29259=CARTESIAN_POINT('Ctrl Pts',(32.4659536029866,-16.1804714646211,31.0353407424038));
#29260=CARTESIAN_POINT('Ctrl Pts',(32.4168175136245,-16.1795947944396,31.0358001425894));
#29261=CARTESIAN_POINT('Ctrl Pts',(32.3696233879008,-16.1786925325962,31.0362725138779));
#29262=CARTESIAN_POINT('Ctrl Pts',(32.3182581618427,-16.1777105272546,31.0367866341767));
#29263=CARTESIAN_POINT('Ctrl Pts',(32.2691934412642,-16.1766975364928,31.0373164741889));
#29264=CARTESIAN_POINT('Ctrl Pts',(32.220906472482,-16.1756521425246,31.0378627004434));
#29265=CARTESIAN_POINT('Ctrl Pts',(32.1715370438644,-16.1745833137248,31.0384211715746));
#29266=CARTESIAN_POINT('Ctrl Pts',(32.1229805798603,-16.173479840102,31.0389971805319));
#29267=CARTESIAN_POINT('Ctrl Pts',(32.0735591134784,-16.1723205501867,31.039601856364));
#29268=CARTESIAN_POINT('Ctrl Pts',(32.0254239419646,-16.1711914331653,31.0401907942692));
#29269=CARTESIAN_POINT('Ctrl Pts',(31.9764682879417,-16.1700086968177,31.0408072809901));
#29270=CARTESIAN_POINT('Ctrl Pts',(31.925094792153,-16.1687449477339,31.041465759884));
#29271=CARTESIAN_POINT('Ctrl Pts',(31.8952919104888,-16.168011819419,31.0418477578044));
#29272=CARTESIAN_POINT('Ctrl Pts',(31.8646744620483,-16.1672513233696,31.0422439429542));
#29273=CARTESIAN_POINT('Ctrl Pts',(31.8329224323944,-16.1664582369103,31.0426570718779));
#29274=CARTESIAN_POINT('Ctrl Pts',(31.7319354368356,-16.1639358337881,31.0439710240642));
#29275=CARTESIAN_POINT('Ctrl Pts',(31.6284526822057,-16.1613063818566,31.0453389332579));
#29276=CARTESIAN_POINT('Ctrl Pts',(31.5232336354319,-16.1587277943726,31.0466795487252));
#29277=CARTESIAN_POINT('Ctrl Pts',(31.4188807866256,-16.156170434673,31.0480091278028));
#29278=CARTESIAN_POINT('Ctrl Pts',(31.3128198672035,-16.1536645426213,31.0493111005243));
#29279=CARTESIAN_POINT('Ctrl Pts',(31.2058402970424,-16.1513736799427,31.0505011542277));
#29280=CARTESIAN_POINT('Ctrl Pts',(31.1464339374063,-16.1501015509562,31.0511619977718));
#29281=CARTESIAN_POINT('Ctrl Pts',(31.086745188952,-16.1488957763821,31.051788304276));
#29282=CARTESIAN_POINT('Ctrl Pts',(31.0269161235859,-16.1477831210734,31.052366291213));
#29283=CARTESIAN_POINT('Ctrl Pts',(30.9223727403119,-16.1458389029967,31.0533762469848));
#29284=CARTESIAN_POINT('Ctrl Pts',(30.8173993541569,-16.1441811147896,31.0542375463396));
#29285=CARTESIAN_POINT('Ctrl Pts',(30.7129204018003,-16.1429541726495,31.0548748925162));
#29286=CARTESIAN_POINT('Ctrl Pts',(30.6397146645874,-16.1420944855847,31.0553214647269));
#29287=CARTESIAN_POINT('Ctrl Pts',(30.5667525557982,-16.1414458510595,31.0556583368409));
#29288=CARTESIAN_POINT('Ctrl Pts',(30.4943593393942,-16.1410459118957,31.0558660149161));
#29289=CARTESIAN_POINT('',(30.5,-18.7405179110273,29.559989655385));
#29290=CARTESIAN_POINT('Origin',(30.5,0.,0.));
#29291=CARTESIAN_POINT('Ctrl Pts',(30.5049791805003,-18.7395177484758,29.5605178050973));
#29292=CARTESIAN_POINT('Ctrl Pts',(30.5973676827744,-18.7400797009803,29.560162264643));
#29293=CARTESIAN_POINT('Ctrl Pts',(30.6891105694846,-18.7410567560113,29.559542510155));
#29294=CARTESIAN_POINT('Ctrl Pts',(30.7806774793081,-18.7423441244048,29.5587264396735));
#29295=CARTESIAN_POINT('Ctrl Pts',(30.8441888930629,-18.7432370516298,29.5581604077948));
#29296=CARTESIAN_POINT('Ctrl Pts',(30.9076166453417,-18.7442800408076,29.5574994222392));
#29297=CARTESIAN_POINT('Ctrl Pts',(30.971128809674,-18.7454455999911,29.5567612578201));
#29298=CARTESIAN_POINT('Ctrl Pts',(31.0735567068111,-18.7473253308648,29.5555707987956));
#29299=CARTESIAN_POINT('Ctrl Pts',(31.1762019082914,-18.7495231556641,29.5541800414699));
#29300=CARTESIAN_POINT('Ctrl Pts',(31.2798872709469,-18.7519033574722,29.5526737444515));
#29301=CARTESIAN_POINT('Ctrl Pts',(31.3828989348267,-18.7542680938472,29.5511772346436));
#29302=CARTESIAN_POINT('Ctrl Pts',(31.4869372222122,-18.756814411791,29.5495656759358));
#29303=CARTESIAN_POINT('Ctrl Pts',(31.5928574097442,-18.7594156373084,29.5479181178244));
#29304=CARTESIAN_POINT('Ctrl Pts',(31.6516459294303,-18.7608593866172,29.5470036792766));
#29305=CARTESIAN_POINT('Ctrl Pts',(31.7110150391215,-18.7623200347851,29.5460781618908));
#29306=CARTESIAN_POINT('Ctrl Pts',(31.7711176725243,-18.763774049131,29.5451562912556));
#29307=CARTESIAN_POINT('Ctrl Pts',(31.8409082760365,-18.7654624366936,29.5440858238842));
#29308=CARTESIAN_POINT('Ctrl Pts',(31.9056373311747,-18.7669933631241,29.5431152615715));
#29309=CARTESIAN_POINT('Ctrl Pts',(31.9658882086283,-18.7683675834941,29.5422441375119));
#29310=CARTESIAN_POINT('Ctrl Pts',(32.0341093482756,-18.7699235920325,29.5412577771694));
#29311=CARTESIAN_POINT('Ctrl Pts',(32.0965888127922,-18.7712796560443,29.5403982847666));
#29312=CARTESIAN_POINT('Ctrl Pts',(32.1542362617661,-18.7724634074923,29.5396480149485));
#29313=CARTESIAN_POINT('Ctrl Pts',(32.2151538519828,-18.773714309083,29.5388551849075));
#29314=CARTESIAN_POINT('Ctrl Pts',(32.2706761902186,-18.7747738843965,29.5381836213574));
#29315=CARTESIAN_POINT('Ctrl Pts',(32.3219402247755,-18.7756849339009,29.5376060245819));
#29316=CARTESIAN_POINT('Ctrl Pts',(32.3761674213235,-18.776648643858,29.536995041577));
#29317=CARTESIAN_POINT('Ctrl Pts',(32.4256304058823,-18.7774469218491,29.5364887148649));
#29318=CARTESIAN_POINT('Ctrl Pts',(32.4717350314044,-18.7781265619113,29.5360572749798));
#29319=CARTESIAN_POINT('Ctrl Pts',(32.5214923281234,-18.7788600469327,29.5355916539681));
#29320=CARTESIAN_POINT('Ctrl Pts',(32.5673384642507,-18.7794559410666,29.5352128774493));
#29321=CARTESIAN_POINT('Ctrl Pts',(32.6111004962912,-18.7799576530151,29.5348934788928));
#29322=CARTESIAN_POINT('Ctrl Pts',(32.6551147163156,-18.780462256185,29.5345722397345));
#29323=CARTESIAN_POINT('Ctrl Pts',(32.6970214084842,-18.7808718608789,29.5343108907558));
#29324=CARTESIAN_POINT('Ctrl Pts',(32.7387279964545,-18.7812095285095,29.5340950825232));
#29325=CARTESIAN_POINT('Ctrl Pts',(32.7800761354851,-18.7815442940421,29.5338811290631));
#29326=CARTESIAN_POINT('Ctrl Pts',(32.8212277342329,-18.7818087481603,29.5337116838824));
#29327=CARTESIAN_POINT('Ctrl Pts',(32.864082933751,-18.7820000955041,29.5335890251804));
#29328=CARTESIAN_POINT('Ctrl Pts',(32.903732033251,-18.7821771276952,29.5334755428695));
#29329=CARTESIAN_POINT('Ctrl Pts',(32.9448394203892,-18.7822919200911,29.5334018918637));
#29330=CARTESIAN_POINT('Ctrl Pts',(32.988943859822,-18.7823158450368,29.5333868654406));
#29331=CARTESIAN_POINT('Ctrl Pts',(32.9925102269236,-18.7823177796524,29.5333856503761));
#29332=CARTESIAN_POINT('Ctrl Pts',(32.996096210623,-18.7823191027633,29.5333848297968));
#29333=CARTESIAN_POINT('Ctrl Pts',(32.9997026353889,-18.7823197895506,29.5333844198654));
#29334=CARTESIAN_POINT('Ctrl Pts',(33.0361388185046,-18.782326728253,29.5333802782743));
#29335=CARTESIAN_POINT('Ctrl Pts',(33.0740002606605,-18.7823330770045,29.5333765562529));
#29336=CARTESIAN_POINT('Ctrl Pts',(33.1140504028668,-18.7823389179975,29.5333733966326));
#29337=CARTESIAN_POINT('Ctrl Pts',(33.2460690464808,-18.7823581718611,29.533362981469));
#29338=CARTESIAN_POINT('Ctrl Pts',(33.3720922029407,-18.782366189783,29.5333587011924));
#29339=CARTESIAN_POINT('Ctrl Pts',(33.4992849360726,-18.782373736073,29.5333546566756));
#29340=CARTESIAN_POINT('Ctrl Pts',(33.6626792864138,-18.7823834301894,29.5333494610079));
#29341=CARTESIAN_POINT('Ctrl Pts',(33.8280037294637,-18.7823923459959,29.5333446544026));
#29342=CARTESIAN_POINT('Ctrl Pts',(33.9928746198635,-18.7824059536077,29.5333373313073));
#29343=CARTESIAN_POINT('Ctrl Pts',(34.3226164006631,-18.7824331688313,29.5333226851165));
#29344=CARTESIAN_POINT('Ctrl Pts',(34.6505439708621,-18.7824791512759,29.5332979729652));
#29345=CARTESIAN_POINT('Ctrl Pts',(34.9791449252861,-18.7825099763789,29.5332814027049));
#29346=CARTESIAN_POINT('Ctrl Pts',(35.30774587971,-18.782540801482,29.5332648324445));
#29347=CARTESIAN_POINT('Ctrl Pts',(35.6370202183589,-18.7825564692435,29.5332564040752));
#29348=CARTESIAN_POINT('Ctrl Pts',(35.9661418060974,-18.7825697306317,29.5332492722835));
#29349=CARTESIAN_POINT('Ctrl Pts',(36.2952633938358,-18.7825829920199,29.5332421404918));
#29350=CARTESIAN_POINT('Ctrl Pts',(36.6242322306637,-18.7825938470347,29.5332363052777));
#29351=CARTESIAN_POINT('Ctrl Pts',(36.9531363303404,-18.7826154119861,29.5332247108411));
#29352=CARTESIAN_POINT('Ctrl Pts',(38.1022190076918,-18.7826907528289,29.5331842036954));
#29353=CARTESIAN_POINT('Ctrl Pts',(39.2505115204485,-18.782896816333,29.5330734009978));
#29354=CARTESIAN_POINT('Ctrl Pts',(40.400093943525,-18.7829477771169,29.533045998731));
#29355=CARTESIAN_POINT('Ctrl Pts',(6.89999999997365,-9.63452070648359,5.3678954269134));
#29356=CARTESIAN_POINT('Ctrl Pts',(6.99168932310453,-9.60499723839754,5.42175501956));
#29357=CARTESIAN_POINT('Ctrl Pts',(7.08383915760479,-9.57508016834563,5.47527828673705));
#29358=CARTESIAN_POINT('Ctrl Pts',(8.15762752947027,-9.22342495405908,6.09209251732962));
#29359=CARTESIAN_POINT('Ctrl Pts',(9.16608342448599,-8.84591675027098,6.61836595106259));
#29360=CARTESIAN_POINT('Ctrl Pts',(11.2535425311854,-8.09542754093136,7.53037930120419));
#29361=CARTESIAN_POINT('Ctrl Pts',(12.2577133097064,-7.70725001371761,7.91666449612081));
#29362=CARTESIAN_POINT('Ctrl Pts',(14.356433377742,-6.97440810645327,8.58141250110813));
#29363=CARTESIAN_POINT('Ctrl Pts',(15.3659105035251,-6.61345583116597,8.85322312286061));
#29364=CARTESIAN_POINT('Ctrl Pts',(17.4728641219044,-5.96623757129008,9.31281879192962));
#29365=CARTESIAN_POINT('Ctrl Pts',(18.4890996814195,-5.66020885204394,9.49384943617778));
#29366=CARTESIAN_POINT('Ctrl Pts',(19.8476172011441,-5.32865724601649,9.68599953593307));
#29367=CARTESIAN_POINT('Ctrl Pts',(20.3454889307686,-5.2093054291626,9.75195458239818));
#29368=CARTESIAN_POINT('Ctrl Pts',(21.3782040612024,-4.97678151322347,9.87366876552719));
#29369=CARTESIAN_POINT('Ctrl Pts',(22.1792648896895,-4.81935607344487,9.95072592994714));
#29370=CARTESIAN_POINT('Ctrl Pts',(22.8542621828909,-4.70591921690555,10.0067883222623));
#29371=CARTESIAN_POINT('Ctrl Pts',(23.1054579010968,-4.66456206383028,10.0267605301623));
#29372=CARTESIAN_POINT('Ctrl Pts',(23.6171513959785,-4.58448144656259,10.0644076466806));
#29373=CARTESIAN_POINT('Ctrl Pts',(24.1360713221937,-4.51012725444835,10.0979855598765));
#29374=CARTESIAN_POINT('Ctrl Pts',(24.6624927871864,-4.44285620865166,10.1277002159266));
#29375=CARTESIAN_POINT('Ctrl Pts',(25.1928168818088,-4.3809527171812,10.154786256444));
#29376=CARTESIAN_POINT('Ctrl Pts',(25.5948982287615,-4.34117176259643,10.1721457030179));
#29377=CARTESIAN_POINT('Ctrl Pts',(26.1232031889651,-4.29604941535507,10.1922876384417));
#29378=CARTESIAN_POINT('Ctrl Pts',(27.1768897027567,-4.2232612911204,10.2241871753182));
#29379=CARTESIAN_POINT('Ctrl Pts',(28.2111297865347,-4.19969555688313,10.2325109692973));
#29380=CARTESIAN_POINT('Ctrl Pts',(29.1277555719713,-4.17661492679514,10.2421056253618));
#29381=CARTESIAN_POINT('Ctrl Pts',(29.4767605677587,-4.1700561490002,10.2448788784735));
#29382=CARTESIAN_POINT('Ctrl Pts',(30.1601418995912,-4.16421367130872,10.2473221772452));
#29383=CARTESIAN_POINT('Ctrl Pts',(31.3500242312262,-4.16794387579264,10.2457563290907));
#29384=CARTESIAN_POINT('Ctrl Pts',(32.3461596131128,-4.18040640609126,10.2405791191157));
#29385=CARTESIAN_POINT('Ctrl Pts',(33.1614718826738,-4.18039330945984,10.2405840900447));
#29386=CARTESIAN_POINT('Ctrl Pts',(33.4925794155279,-4.18039253080268,10.2405841444578));
#29387=CARTESIAN_POINT('Ctrl Pts',(34.1499904318886,-4.18039030822715,10.2405848392549));
#29388=CARTESIAN_POINT('Ctrl Pts',(34.9738731541179,-4.18038393925505,10.2405865289644));
#29389=CARTESIAN_POINT('Ctrl Pts',(35.9612754428242,-4.18038119412748,10.2405873001735));
#29390=CARTESIAN_POINT('Ctrl Pts',(37.936646788162,-4.18037753677864,10.2405882857915));
#29391=CARTESIAN_POINT('Ctrl Pts',(39.5833333333333,-4.18035859466987,10.2405934798255));
#29392=CARTESIAN_POINT('Ctrl Pts',(40.9,-4.18035859466987,10.2405934798255));
#29393=CARTESIAN_POINT('Ctrl Pts',(6.71972576838711,-12.8464244365415,6.5764381714634));
#29394=CARTESIAN_POINT('Ctrl Pts',(6.81144220747046,-12.8102053989753,6.6482837686261));
#29395=CARTESIAN_POINT('Ctrl Pts',(6.90362823998598,-12.7734498343709,6.71971524922859));
#29396=CARTESIAN_POINT('Ctrl Pts',(7.97787811486329,-12.3410744046091,7.54294881554194));
#29397=CARTESIAN_POINT('Ctrl Pts',(8.98681832185142,-11.871220138602,8.24809748747637));
#29398=CARTESIAN_POINT('Ctrl Pts',(11.0806583453373,-10.9274240314556,9.47774891389534));
#29399=CARTESIAN_POINT('Ctrl Pts',(12.0862475175457,-10.4368998098018,10.0005505115845));
#29400=CARTESIAN_POINT('Ctrl Pts',(14.197639322261,-9.50280276487817,10.906656993414));
#29401=CARTESIAN_POINT('Ctrl Pts',(15.2100862637122,-9.0420363325472,11.2785931828498));
#29402=CARTESIAN_POINT('Ctrl Pts',(17.3364698493954,-8.20932952666153,11.9121957711898));
#29403=CARTESIAN_POINT('Ctrl Pts',(18.357279581038,-7.81594677169139,12.1627870018009));
#29404=CARTESIAN_POINT('Ctrl Pts',(19.7331217809845,-7.38628119283516,12.4307568384137));
#29405=CARTESIAN_POINT('Ctrl Pts',(20.2341927100358,-7.23233618870704,12.5225360922774));
#29406=CARTESIAN_POINT('Ctrl Pts',(21.2777139275316,-6.93114017240205,12.6928916013278));
#29407=CARTESIAN_POINT('Ctrl Pts',(22.0885637816418,-6.72673758680647,12.8012350092453));
#29408=CARTESIAN_POINT('Ctrl Pts',(22.7734874647764,-6.57909772915772,12.8801738355232));
#29409=CARTESIAN_POINT('Ctrl Pts',(23.0269571312139,-6.52549682636868,12.9082278965574));
#29410=CARTESIAN_POINT('Ctrl Pts',(23.5444618566097,-6.42148511325403,12.9612738268023));
#29411=CARTESIAN_POINT('Ctrl Pts',(24.0694383156461,-6.32485290039694,13.0087020921734));
#29412=CARTESIAN_POINT('Ctrl Pts',(24.6027295908464,-6.2373000813771,13.0507741241225));
#29413=CARTESIAN_POINT('Ctrl Pts',(25.1403192523141,-6.15667530541499,13.0891677302172));
#29414=CARTESIAN_POINT('Ctrl Pts',(25.5484689870706,-6.10479659087691,13.1137995888261));
#29415=CARTESIAN_POINT('Ctrl Pts',(26.0852808149067,-6.04589855121055,13.1423647911197));
#29416=CARTESIAN_POINT('Ctrl Pts',(27.1586857291269,-5.95074158602808,13.1877077660314));
#29417=CARTESIAN_POINT('Ctrl Pts',(28.1995312980844,-5.92039197700574,13.1995114624862));
#29418=CARTESIAN_POINT('Ctrl Pts',(29.1157533315888,-5.89061060808306,13.2130297822556));
#29419=CARTESIAN_POINT('Ctrl Pts',(29.4698938670486,-5.88204921070823,13.2169740538762));
#29420=CARTESIAN_POINT('Ctrl Pts',(30.1587234046998,-5.8744768355958,13.220429005539));
#29421=CARTESIAN_POINT('Ctrl Pts',(31.355731195606,-5.87931523414859,13.2182120926509));
#29422=CARTESIAN_POINT('Ctrl Pts',(32.350180243561,-5.89537176970751,13.2109234983782));
#29423=CARTESIAN_POINT('Ctrl Pts',(33.1605031382466,-5.89535013085609,13.2109314016452));
#29424=CARTESIAN_POINT('Ctrl Pts',(33.4922179295252,-5.89534881762644,13.2109314596682));
#29425=CARTESIAN_POINT('Ctrl Pts',(34.1493400019899,-5.89534512891168,13.2109325467447));
#29426=CARTESIAN_POINT('Ctrl Pts',(34.9735241318652,-5.89533452524069,13.2109351472382));
#29427=CARTESIAN_POINT('Ctrl Pts',(35.9608954520827,-5.89532995964262,13.2109363413972));
#29428=CARTESIAN_POINT('Ctrl Pts',(37.9363824842976,-5.8953238722353,13.2109378608691));
#29429=CARTESIAN_POINT('Ctrl Pts',(39.5833333333333,-5.89529235427929,13.2109458830841));
#29430=CARTESIAN_POINT('Ctrl Pts',(40.9,-5.89529235427929,13.2109458830841));
#29431=CARTESIAN_POINT('Ctrl Pts',(6.48177011792014,-20.336764848396,9.40621265917915));
#29432=CARTESIAN_POINT('Ctrl Pts',(6.57271435585528,-20.2851799357091,9.51911083717172));
#29433=CARTESIAN_POINT('Ctrl Pts',(6.66411141569866,-20.2327517601296,9.63139437446865));
#29434=CARTESIAN_POINT('Ctrl Pts',(7.73048017258431,-19.614616528956,10.9276768808967));
#29435=CARTESIAN_POINT('Ctrl Pts',(8.73292722985417,-18.9319609573801,12.0456324995184));
#29436=CARTESIAN_POINT('Ctrl Pts',(10.8102906905198,-17.5485371602851,14.0013807284478));
#29437=CARTESIAN_POINT('Ctrl Pts',(11.8125687231201,-16.8218444562665,14.8418955382559));
#29438=CARTESIAN_POINT('Ctrl Pts',(13.9177445864075,-15.4271303717407,16.3050153868123));
#29439=CARTESIAN_POINT('Ctrl Pts',(14.9296562678442,-14.7350649820735,16.9116612373854));
#29440=CARTESIAN_POINT('Ctrl Pts',(17.0680844879216,-13.4708635112562,17.9535844659564));
#29441=CARTESIAN_POINT('Ctrl Pts',(18.0932339179161,-12.8729609429,18.3688941094638));
#29442=CARTESIAN_POINT('Ctrl Pts',(19.4933464326809,-12.2099892645604,18.8183285494774));
#29443=CARTESIAN_POINT('Ctrl Pts',(19.9993272808496,-11.9744841299437,18.971430097181));
#29444=CARTESIAN_POINT('Ctrl Pts',(21.0600020168761,-11.5100300116438,19.2581324129064));
#29445=CARTESIAN_POINT('Ctrl Pts',(21.8888875769482,-11.1928649299996,19.4420158954032));
#29446=CARTESIAN_POINT('Ctrl Pts',(22.5933490549503,-10.962505511385,19.5764520117208));
#29447=CARTESIAN_POINT('Ctrl Pts',(22.8513437851799,-10.8796937171906,19.6238525927722));
#29448=CARTESIAN_POINT('Ctrl Pts',(23.3805933886566,-10.7182299385361,19.7139851739534));
#29449=CARTESIAN_POINT('Ctrl Pts',(23.9182257576784,-10.5680285062335,19.7948254980796));
#29450=CARTESIAN_POINT('Ctrl Pts',(24.4662138806867,-10.4315004891655,19.8668205194741));
#29451=CARTESIAN_POINT('Ctrl Pts',(25.0195744741822,-10.3055778221167,19.9326328666884));
#29452=CARTESIAN_POINT('Ctrl Pts',(25.4412458088222,-10.2242864909386,19.9749776253082));
#29453=CARTESIAN_POINT('Ctrl Pts',(25.9971983460992,-10.131797107587,20.0240850656221));
#29454=CARTESIAN_POINT('Ctrl Pts',(27.1157050405652,-9.98182332250462,20.102368552767));
#29455=CARTESIAN_POINT('Ctrl Pts',(28.1723100127449,-9.93573708068025,20.1222437541335));
#29456=CARTESIAN_POINT('Ctrl Pts',(29.0876106506766,-9.89029022572785,20.1449463132817));
#29457=CARTESIAN_POINT('Ctrl Pts',(29.4537207931442,-9.87684873205164,20.1517438988729));
#29458=CARTESIAN_POINT('Ctrl Pts',(30.1552759232946,-9.86516345924738,20.1576060163182));
#29459=CARTESIAN_POINT('Ctrl Pts',(31.368924127636,-9.87263514017793,20.1538463873917));
#29460=CARTESIAN_POINT('Ctrl Pts',(32.3594787154311,-9.89702302165624,20.1416711708076));
#29461=CARTESIAN_POINT('Ctrl Pts',(33.1581760188914,-9.89696607979067,20.1416983285705));
#29462=CARTESIAN_POINT('Ctrl Pts',(33.4913102145729,-9.89696201382195,20.1416998058431));
#29463=CARTESIAN_POINT('Ctrl Pts',(34.1477617736107,-9.89695193052414,20.1417043298969));
#29464=CARTESIAN_POINT('Ctrl Pts',(34.9726616332633,-9.89692218573783,20.1417171222835));
#29465=CARTESIAN_POINT('Ctrl Pts',(35.9599657908142,-9.89690948638392,20.1417226604566));
#29466=CARTESIAN_POINT('Ctrl Pts',(37.9357298104643,-9.89689244880616,20.1417300151411));
#29467=CARTESIAN_POINT('Ctrl Pts',(39.5833333333333,-9.8968044600346,20.1417681573542));
#29468=CARTESIAN_POINT('Ctrl Pts',(40.9,-9.8968044600346,20.1417681573542));
#29469=CARTESIAN_POINT('Ctrl Pts',(6.40644620858992,-27.7818319413302,12.3446157076951));
#29470=CARTESIAN_POINT('Ctrl Pts',(6.49686818484384,-27.7146057723315,12.4976194141968));
#29471=CARTESIAN_POINT('Ctrl Pts',(6.58771883172007,-27.6462615383487,12.6497754970257));
#29472=CARTESIAN_POINT('Ctrl Pts',(7.64885870107047,-26.8389674658771,14.4089312086777));
#29473=CARTESIAN_POINT('Ctrl Pts',(8.64786699401839,-25.9406999974138,15.9309901815184));
#29474=CARTESIAN_POINT('Ctrl Pts',(10.7071344443812,-24.1258468463739,18.5841088194585));
#29475=CARTESIAN_POINT('Ctrl Pts',(11.7059636153277,-23.1640388241121,19.7351568023896));
#29476=CARTESIAN_POINT('Ctrl Pts',(13.7894167134297,-21.32755345859,21.7274097031724));
#29477=CARTESIAN_POINT('Ctrl Pts',(14.7964804448639,-20.40896606215,22.5625068415354));
#29478=CARTESIAN_POINT('Ctrl Pts',(16.9150096963281,-18.734786787185,23.9923642448819));
#29479=CARTESIAN_POINT('Ctrl Pts',(17.9356563974909,-17.9376031564435,24.568778311437));
#29480=CARTESIAN_POINT('Ctrl Pts',(19.3316378726113,-17.0495061236355,25.1942531765859));
#29481=CARTESIAN_POINT('Ctrl Pts',(19.8373783148988,-16.733671277521,25.4080883980548));
#29482=CARTESIAN_POINT('Ctrl Pts',(20.8986146451321,-16.1088561234904,25.8097110946141));
#29483=CARTESIAN_POINT('Ctrl Pts',(21.7322089233615,-15.6790344990822,26.0695581056351));
#29484=CARTESIAN_POINT('Ctrl Pts',(22.4452152218927,-15.3644450466695,26.2607608176433));
#29485=CARTESIAN_POINT('Ctrl Pts',(22.7053175952387,-15.2520352575855,26.3278633535721));
#29486=CARTESIAN_POINT('Ctrl Pts',(23.2405350109147,-15.0319031635372,26.4560495577169));
#29487=CARTESIAN_POINT('Ctrl Pts',(23.7856351879594,-14.8265027181049,26.5714803865859));
#29488=CARTESIAN_POINT('Ctrl Pts',(24.3434088150882,-14.6389049166987,26.6748081507042));
#29489=CARTESIAN_POINT('Ctrl Pts',(24.9080926446007,-14.4653482504621,26.7695587595053));
#29490=CARTESIAN_POINT('Ctrl Pts',(25.3404979553364,-14.3526452692475,26.8308622015487));
#29491=CARTESIAN_POINT('Ctrl Pts',(25.9125607075504,-14.2239063651395,26.9021372597287));
#29492=CARTESIAN_POINT('Ctrl Pts',(27.0720378258712,-14.0136986134135,27.0165941086124));
#29493=CARTESIAN_POINT('Ctrl Pts',(28.1454151442859,-13.9518646781025,27.0445191043407));
#29494=CARTESIAN_POINT('Ctrl Pts',(29.0596751952944,-13.890725520751,27.0764264216485));
#29495=CARTESIAN_POINT('Ctrl Pts',(29.4376599373188,-13.8719255145712,27.0863532011149));
#29496=CARTESIAN_POINT('Ctrl Pts',(30.1519376760718,-13.855954576287,27.0947220176404));
#29497=CARTESIAN_POINT('Ctrl Pts',(31.3821999577689,-13.8661782937677,27.0893514143297));
#29498=CARTESIAN_POINT('Ctrl Pts',(32.3688386893657,-13.8987881217581,27.0723527225427));
#29499=CARTESIAN_POINT('Ctrl Pts',(33.1558986739574,-13.8986675947835,27.0724155351932));
#29500=CARTESIAN_POINT('Ctrl Pts',(33.49045038666,-13.8986584195583,27.072419804706));
#29501=CARTESIAN_POINT('Ctrl Pts',(34.1462287076184,-13.8986367255002,27.0724307945236));
#29502=CARTESIAN_POINT('Ctrl Pts',(34.9718350023128,-13.8985720488061,27.0724629552156));
#29503=CARTESIAN_POINT('Ctrl Pts',(35.9590682028415,-13.8985445297568,27.0724767217601));
#29504=CARTESIAN_POINT('Ctrl Pts',(37.9351039480424,-13.8985075170899,27.072495155898));
#29505=CARTESIAN_POINT('Ctrl Pts',(39.5833333333333,-13.8983165657899,27.0725904316243));
#29506=CARTESIAN_POINT('Ctrl Pts',(40.9,-13.8983165657899,27.0725904316243));
#29507=CARTESIAN_POINT('Ctrl Pts',(6.37427268165564,-32.0290848932163,14.0406695266741));
#29508=CARTESIAN_POINT('Ctrl Pts',(6.46448755772839,-31.9528098065586,14.2166050753401));
#29509=CARTESIAN_POINT('Ctrl Pts',(6.55512327887566,-31.8752581000468,14.3915605358513));
#29510=CARTESIAN_POINT('Ctrl Pts',(7.61410360785656,-30.958672886913,16.4151695040826));
#29511=CARTESIAN_POINT('Ctrl Pts',(8.61142775869687,-29.9361952854453,18.1677152487792));
#29512=CARTESIAN_POINT('Ctrl Pts',(10.6634825022472,-27.8730682250753,21.2183968262284));
#29513=CARTESIAN_POINT('Ctrl Pts',(11.6607542873627,-26.7761583709752,22.5462154536683));
#29514=CARTESIAN_POINT('Ctrl Pts',(13.7353039743977,-24.6873364683673,24.8383185913233));
#29515=CARTESIAN_POINT('Ctrl Pts',(14.7402095633116,-23.6392130729629,25.8029859119439));
#29516=CARTESIAN_POINT('Ctrl Pts',(16.8490881066137,-21.733995182915,27.450307490631));
#29517=CARTESIAN_POINT('Ctrl Pts',(17.8672038783315,-20.8239061433235,28.117536242687));
#29518=CARTESIAN_POINT('Ctrl Pts',(19.2585933984997,-19.811022849419,28.8404836901117));
#29519=CARTESIAN_POINT('Ctrl Pts',(19.7636418533908,-19.4499572035579,29.0884650342026));
#29520=CARTESIAN_POINT('Ctrl Pts',(20.8231816497994,-18.7357747989968,29.5540603372584));
#29521=CARTESIAN_POINT('Ctrl Pts',(21.6568670511735,-18.2431916560479,29.8562628482713));
#29522=CARTESIAN_POINT('Ctrl Pts',(22.3720072062877,-17.8815051531588,30.0792593376712));
#29523=CARTESIAN_POINT('Ctrl Pts',(22.6326824787813,-17.7523977438432,30.1574913312728));
#29524=CARTESIAN_POINT('Ctrl Pts',(23.1697036949937,-17.4991937768336,30.3071564102286));
#29525=CARTESIAN_POINT('Ctrl Pts',(23.7174377716562,-17.2625030946595,30.4422233412819));
#29526=CARTESIAN_POINT('Ctrl Pts',(24.2790946262572,-17.0457855087881,30.5634410393029));
#29527=CARTESIAN_POINT('Ctrl Pts',(24.8485847331463,-16.8449230908939,30.6748008187179));
#29528=CARTESIAN_POINT('Ctrl Pts',(25.2859632686137,-16.714000734413,30.7471152582869));
#29529=CARTESIAN_POINT('Ctrl Pts',(25.8659001690755,-16.5640760155963,30.8313513860032));
#29530=CARTESIAN_POINT('Ctrl Pts',(27.0467877055032,-16.3181083484215,30.9672841404844));
#29531=CARTESIAN_POINT('Ctrl Pts',(28.1301993946288,-16.2470842981322,30.9999203594232));
#29532=CARTESIAN_POINT('Ctrl Pts',(29.0438132065911,-16.1769735529556,31.0370949113971));
#29533=CARTESIAN_POINT('Ctrl Pts',(29.4285323170642,-16.1549555741443,31.0489002942269));
#29534=CARTESIAN_POINT('Ctrl Pts',(30.1500796604944,-16.1364761766636,31.0587367393328));
#29535=CARTESIAN_POINT('Ctrl Pts',(31.3898224001987,-16.1483068856791,31.0524272220083));
#29536=CARTESIAN_POINT('Ctrl Pts',(32.3742147772173,-16.1855693458549,31.0327017051641));
#29537=CARTESIAN_POINT('Ctrl Pts',(33.1546196294426,-16.1853991323255,31.0327939306214));
#29538=CARTESIAN_POINT('Ctrl Pts',(33.4899805045662,-16.185385634532,31.0328008093452));
#29539=CARTESIAN_POINT('Ctrl Pts',(34.1453728987309,-16.1853546639146,31.0328173216774));
#29540=CARTESIAN_POINT('Ctrl Pts',(34.9713787068036,-16.1852616946182,31.0328663827335));
#29541=CARTESIAN_POINT('Ctrl Pts',(35.9585696612047,-16.1852222245757,31.0328872804502));
#29542=CARTESIAN_POINT('Ctrl Pts',(37.9347583211501,-16.1851690519237,31.0329153648958));
#29543=CARTESIAN_POINT('Ctrl Pts',(39.5833333333333,-16.1848949119358,31.0330603026358));
#29544=CARTESIAN_POINT('Ctrl Pts',(40.9,-16.1848949119358,31.0330603026358));
#29545=CARTESIAN_POINT('',(40.9,-15.1839076262003,29.2992994660114));
#29546=CARTESIAN_POINT('Ctrl Pts',(40.9,-15.1839076262003,29.2992994660114));
#29547=CARTESIAN_POINT('Ctrl Pts',(40.9,-15.4341550287793,29.7327406817405));
#29548=CARTESIAN_POINT('Ctrl Pts',(40.9,-15.6844024313584,30.1661818974696));
#29549=CARTESIAN_POINT('Ctrl Pts',(40.9,-15.9346498339374,30.5996231131986));
#29550=CARTESIAN_POINT('',(38.,-15.1839076262003,29.2992994660114));
#29551=CARTESIAN_POINT('Ctrl Pts',(38.,-15.1839076262003,29.2992994660114));
#29552=CARTESIAN_POINT('Ctrl Pts',(38.9666666666667,-15.1839076262003,29.2992994660114));
#29553=CARTESIAN_POINT('Ctrl Pts',(39.9333333333333,-15.1839076262003,29.2992994660114));
#29554=CARTESIAN_POINT('Ctrl Pts',(40.9,-15.1839076262003,29.2992994660114));
#29555=CARTESIAN_POINT('Ctrl Pts',(37.4974382384971,-14.8838038109906,28.7790269720418));
#29556=CARTESIAN_POINT('Ctrl Pts',(37.6645213547142,-14.9840691120817,28.9527098777876));
#29557=CARTESIAN_POINT('Ctrl Pts',(37.8313739960413,-15.0841847150558,29.1261374112001));
#29558=CARTESIAN_POINT('Ctrl Pts',(37.9978889629903,-15.1840905833949,29.2992044501375));
#29559=CARTESIAN_POINT('',(6.9,-27.0393531365015,12.9951291628659));
#29560=CARTESIAN_POINT('Ctrl Pts',(6.9,-27.0393531365015,12.9951291628659));
#29561=CARTESIAN_POINT('Ctrl Pts',(6.9,-24.649274247254,11.9174419758914));
#29562=CARTESIAN_POINT('Ctrl Pts',(6.90000000000115,-22.230729924082,10.8339866674746));
#29563=CARTESIAN_POINT('Ctrl Pts',(6.90000000000115,-16.7584145047598,8.41000082059024));
#29564=CARTESIAN_POINT('Ctrl Pts',(6.9,-13.1312177506378,6.82522008706163));
#29565=CARTESIAN_POINT('Ctrl Pts',(6.9,-9.63452070648529,5.36789542693312));
#29566=CARTESIAN_POINT('',(22.9245129145126,-15.8853026165582,27.5141512254857));
#29567=CARTESIAN_POINT('Ctrl Pts',(22.9245129145126,-15.8853026165582,27.5141512254857));
#29568=CARTESIAN_POINT('Ctrl Pts',(22.7202811020963,-15.9355315703924,27.405303612937));
#29569=CARTESIAN_POINT('Ctrl Pts',(22.5089075447093,-15.9922246435191,27.2924652433825));
#29570=CARTESIAN_POINT('Ctrl Pts',(22.2913349439917,-16.0558281873747,27.1762359097413));
#29571=CARTESIAN_POINT('Ctrl Pts',(21.4451770585293,-16.3031876434794,26.7242103933932));
#29572=CARTESIAN_POINT('Ctrl Pts',(20.5220951556669,-16.6965145338605,26.2108400614943));
#29573=CARTESIAN_POINT('Ctrl Pts',(19.767142881954,-17.0753616782143,25.777085937268));
#29574=CARTESIAN_POINT('Ctrl Pts',(19.5194773058392,-17.1996442316059,25.634790895834));
#29575=CARTESIAN_POINT('Ctrl Pts',(19.2865716386091,-17.3225345039426,25.4994131575072));
#29576=CARTESIAN_POINT('Ctrl Pts',(19.0728538401323,-17.4387046858284,25.3740784559106));
#29577=CARTESIAN_POINT('Ctrl Pts',(18.7028555998035,-17.6398239336529,25.15709316328));
#29578=CARTESIAN_POINT('Ctrl Pts',(18.4144703596235,-17.8106758656205,24.9815167506411));
#29579=CARTESIAN_POINT('Ctrl Pts',(18.0642874871537,-18.0298340093775,24.7606238748751));
#29580=CARTESIAN_POINT('Ctrl Pts',(17.4420927116721,-18.4192278454841,24.3681478172274));
#29581=CARTESIAN_POINT('Ctrl Pts',(16.7224564418218,-18.9163953124275,23.8866996305775));
#29582=CARTESIAN_POINT('Ctrl Pts',(15.9202806616111,-19.5075155171573,23.2999769887242));
#29583=CARTESIAN_POINT('Ctrl Pts',(15.409052983452,-19.8842371999007,22.926057878577));
#29584=CARTESIAN_POINT('Ctrl Pts',(14.8739602945718,-20.3065653819879,22.5035099772299));
#29585=CARTESIAN_POINT('Ctrl Pts',(14.316979433116,-20.764045054618,22.0244589523046));
#29586=CARTESIAN_POINT('Ctrl Pts',(13.886420676284,-21.1176871503423,21.6541417151704));
#29587=CARTESIAN_POINT('Ctrl Pts',(13.3867890027807,-21.5394320189423,21.2019814327446));
#29588=CARTESIAN_POINT('Ctrl Pts',(12.8146824059514,-22.0238946695559,20.6456427149589));
#29589=CARTESIAN_POINT('Ctrl Pts',(12.2526665517595,-22.499812430193,20.0991166279862));
#29590=CARTESIAN_POINT('Ctrl Pts',(11.6379478462803,-23.0419154065947,19.44703563439));
#29591=CARTESIAN_POINT('Ctrl Pts',(10.9739250490308,-23.626535453056,18.6689137476991));
#29592=CARTESIAN_POINT('Ctrl Pts',(10.5683455447963,-23.9836164291782,18.1936434853748));
#29593=CARTESIAN_POINT('Ctrl Pts',(10.1437415406956,-24.3558958755273,17.6694303965612));
#29594=CARTESIAN_POINT('Ctrl Pts',(9.74137929176525,-24.6998029803349,17.1528053766524));
#29595=CARTESIAN_POINT('Ctrl Pts',(8.72285779294234,-25.5703537856744,15.8450442956717));
#29596=CARTESIAN_POINT('Ctrl Pts',(7.81323138778195,-26.3485431508901,14.4751178145147));
#29597=CARTESIAN_POINT('Ctrl Pts',(6.9,-27.0393531365015,12.9951291628659));
#29598=CARTESIAN_POINT('Ctrl Pts',(30.5,-16.1402285275843,31.0562879796886));
#29599=CARTESIAN_POINT('Ctrl Pts',(29.9560179420817,-16.0158030554221,30.8470467059701));
#29600=CARTESIAN_POINT('Ctrl Pts',(29.4152668325132,-15.9055856438304,30.6299015220344));
#29601=CARTESIAN_POINT('Ctrl Pts',(28.8740459957565,-15.8236145009996,30.3967092920472));
#29602=CARTESIAN_POINT('Ctrl Pts',(28.353527792344,-15.7447788961961,30.1724370682909));
#29603=CARTESIAN_POINT('Ctrl Pts',(27.8179515912467,-15.65999396651,29.9423746730404));
#29604=CARTESIAN_POINT('Ctrl Pts',(27.2695051149491,-15.5981844167478,29.6962958928787));
#29605=CARTESIAN_POINT('Ctrl Pts',(26.9554553615883,-15.5627912203338,29.5553870101399));
#29606=CARTESIAN_POINT('Ctrl Pts',(26.6378099296971,-15.5350208970661,29.4095747645068));
#29607=CARTESIAN_POINT('Ctrl Pts',(26.3179304017917,-15.5205235030951,29.2578762499931));
#29608=CARTESIAN_POINT('Ctrl Pts',(26.1078196745982,-15.5110009868853,29.1582340959379));
#29609=CARTESIAN_POINT('Ctrl Pts',(25.8967402232745,-15.507207179043,29.0560612282453));
#29610=CARTESIAN_POINT('Ctrl Pts',(25.6850706236774,-15.5107635234098,28.9510881944939));
#29611=CARTESIAN_POINT('Ctrl Pts',(25.6562210027417,-15.5112482372614,28.9367808388889));
#29612=CARTESIAN_POINT('Ctrl Pts',(25.6277737638215,-15.5118582602788,28.9226278510966));
#29613=CARTESIAN_POINT('Ctrl Pts',(25.5983858063598,-15.5126342200129,28.9079571471847));
#29614=CARTESIAN_POINT('Ctrl Pts',(25.1249357452756,-15.5251351971226,28.6716070819486));
#29615=CARTESIAN_POINT('Ctrl Pts',(24.1510084067019,-15.5836572228941,28.1678256190434));
#29616=CARTESIAN_POINT('Ctrl Pts',(22.9245129145126,-15.8853026165582,27.5141512254857));
#29617=CARTESIAN_POINT('Origin',(40.65,0.,0.));
#29618=CARTESIAN_POINT('',(40.4,-31.0330398077868,16.1848830792292));
#29619=CARTESIAN_POINT('',(40.9,-30.5996231131986,15.9346498339374));
#29620=CARTESIAN_POINT('Ctrl Pts',(40.4,-31.0330398077868,16.1848830792292));
#29621=CARTESIAN_POINT('Ctrl Pts',(40.5666590129021,-30.8885761371497,16.1014769400988));
#29622=CARTESIAN_POINT('Ctrl Pts',(40.7333430446799,-30.7440888809087,16.0180571838136));
#29623=CARTESIAN_POINT('Ctrl Pts',(40.9,-30.5996231131986,15.9346498339374));
#29624=CARTESIAN_POINT('',(40.9,-29.0996231131986,18.5327260452908));
#29625=CARTESIAN_POINT('Origin',(40.9,0.,0.));
#29626=CARTESIAN_POINT('',(40.4,-29.5330398077868,18.7829592905825));
#29627=CARTESIAN_POINT('Ctrl Pts',(40.9,-29.0996231131986,18.5327260452908));
#29628=CARTESIAN_POINT('Ctrl Pts',(40.7333430444293,-29.244088881126,18.6161333952923));
#29629=CARTESIAN_POINT('Ctrl Pts',(40.5666590126687,-29.3885761373521,18.6995531515689));
#29630=CARTESIAN_POINT('Ctrl Pts',(40.4,-29.5330398077868,18.7829592905825));
#29631=CARTESIAN_POINT('Origin',(40.4,0.,0.));
#29632=CARTESIAN_POINT('Origin',(35.7,0.,0.));
#29633=CARTESIAN_POINT('',(30.5,-29.5059919176187,18.8254200738635));
#29634=CARTESIAN_POINT('Ctrl Pts',(40.3998805977094,-29.5330468723883,18.7829479019245));
#29635=CARTESIAN_POINT('Ctrl Pts',(39.2493532038211,-29.5330781202017,18.7828975281218));
#29636=CARTESIAN_POINT('Ctrl Pts',(38.0972325173324,-29.5332042421652,18.7826942098493));
#29637=CARTESIAN_POINT('Ctrl Pts',(36.9466403233753,-29.5332467931519,18.7826256101695));
#29638=CARTESIAN_POINT('Ctrl Pts',(36.7453942973752,-29.533254235595,18.7826136116412));
#29639=CARTESIAN_POINT('Ctrl Pts',(36.5441950314395,-29.5332591214118,18.7826057344612));
#29640=CARTESIAN_POINT('Ctrl Pts',(36.3429831482115,-29.5332638326535,18.7825981392431));
#29641=CARTESIAN_POINT('Ctrl Pts',(36.2103627229288,-29.533266937872,18.7825931331717));
#29642=CARTESIAN_POINT('Ctrl Pts',(36.0823539050873,-29.5332699079824,18.7825884046388));
#29643=CARTESIAN_POINT('Ctrl Pts',(35.9587472612551,-29.533273304022,18.7825830315924));
#29644=CARTESIAN_POINT('Ctrl Pts',(35.7554552092488,-29.5332788893841,18.7825741947079));
#29645=CARTESIAN_POINT('Ctrl Pts',(35.5640774641664,-29.5332855100166,18.78256380265));
#29646=CARTESIAN_POINT('Ctrl Pts',(35.3838244599901,-29.5332919882698,18.7825536727525));
#29647=CARTESIAN_POINT('Ctrl Pts',(35.2391029659002,-29.5332971895284,18.7825455396624));
#29648=CARTESIAN_POINT('Ctrl Pts',(35.1015509582746,-29.5333023181163,18.7825375448068));
#29649=CARTESIAN_POINT('Ctrl Pts',(34.970735999324,-29.5333070397951,18.7825301856736));
#29650=CARTESIAN_POINT('Ctrl Pts',(34.857898178191,-29.533311112601,18.7825238378632));
#29651=CARTESIAN_POINT('Ctrl Pts',(34.7500670454289,-29.5333148977242,18.7825179389498));
#29652=CARTESIAN_POINT('Ctrl Pts',(34.6468496335934,-29.5333184739771,18.7825123391461));
#29653=CARTESIAN_POINT('Ctrl Pts',(34.5887227637577,-29.5333204879433,18.7825091856175));
#29654=CARTESIAN_POINT('Ctrl Pts',(34.5320601650214,-29.5333224349754,18.7825061280289));
#29655=CARTESIAN_POINT('Ctrl Pts',(34.4767987085013,-29.53332432459,18.7825031467392));
#29656=CARTESIAN_POINT('Ctrl Pts',(34.3959515550965,-29.5333270890838,18.7824987851317));
#29657=CARTESIAN_POINT('Ctrl Pts',(34.3181086378963,-29.533329735084,18.7824945795527));
#29658=CARTESIAN_POINT('Ctrl Pts',(34.2432236356273,-29.5333323757695,18.7824903288468));
#29659=CARTESIAN_POINT('Ctrl Pts',(34.162267530415,-29.5333352305416,18.7824857335262));
#29660=CARTESIAN_POINT('Ctrl Pts',(34.0847679659787,-29.5333380786013,18.7824810862876));
#29661=CARTESIAN_POINT('Ctrl Pts',(34.0106064145146,-29.5333409984257,18.7824762390846));
#29662=CARTESIAN_POINT('Ctrl Pts',(34.0011740963656,-29.5333413697867,18.7824756225878));
#29663=CARTESIAN_POINT('Ctrl Pts',(33.9917957065319,-29.5333417422357,18.7824750029764));
#29664=CARTESIAN_POINT('Ctrl Pts',(33.982470944213,-29.5333421158732,18.7824743800457));
#29665=CARTESIAN_POINT('Ctrl Pts',(33.9223617768103,-29.533344524411,18.7824703645173));
#29666=CARTESIAN_POINT('Ctrl Pts',(33.8644761963964,-29.5333469783619,18.7824662176402));
#29667=CARTESIAN_POINT('Ctrl Pts',(33.8085662291514,-29.5333493560496,18.7824621300573));
#29668=CARTESIAN_POINT('Ctrl Pts',(33.7474237015737,-29.5333519562627,18.7824576599214));
#29669=CARTESIAN_POINT('Ctrl Pts',(33.6886441629424,-29.5333544654644,18.7824532603738));
#29670=CARTESIAN_POINT('Ctrl Pts',(33.6319696815246,-29.5333567795574,18.7824490897141));
#29671=CARTESIAN_POINT('Ctrl Pts',(33.5826925637263,-29.5333587916063,18.7824454634244));
#29672=CARTESIAN_POINT('Ctrl Pts',(33.5350083428651,-29.5333606573844,18.7824420081377));
#29673=CARTESIAN_POINT('Ctrl Pts',(33.4887791610293,-29.5333623350578,18.7824387839385));
#29674=CARTESIAN_POINT('Ctrl Pts',(33.4518540159975,-29.5333636750843,18.7824362086383));
#29675=CARTESIAN_POINT('Ctrl Pts',(33.4158630418951,-29.5333649012576,18.7824337706412));
#29676=CARTESIAN_POINT('Ctrl Pts',(33.3809178973936,-29.5333661853239,18.7824311829815));
#29677=CARTESIAN_POINT('Ctrl Pts',(33.3430135141807,-29.533367578128,18.7824283761925));
#29678=CARTESIAN_POINT('Ctrl Pts',(33.3063394413795,-29.533369038868,18.7824253936111));
#29679=CARTESIAN_POINT('Ctrl Pts',(33.2709744549997,-29.5333707165148,18.782421984424));
#29680=CARTESIAN_POINT('Ctrl Pts',(33.2337091833705,-29.5333724843074,18.7824183920493));
#29681=CARTESIAN_POINT('Ctrl Pts',(33.1978968817061,-29.5333744922841,18.7824143270743));
#29682=CARTESIAN_POINT('Ctrl Pts',(33.163568044013,-29.5333768470907,18.7824096072586));
#29683=CARTESIAN_POINT('Ctrl Pts',(33.1258517952642,-29.5333794342588,18.7824044217133));
#29684=CARTESIAN_POINT('Ctrl Pts',(33.0899258346466,-29.5333824396273,18.7823984464624));
#29685=CARTESIAN_POINT('Ctrl Pts',(33.0557653924644,-29.5333859335647,18.782391556659));
#29686=CARTESIAN_POINT('Ctrl Pts',(33.0368719876726,-29.5333878659862,18.7823877460571));
#29687=CARTESIAN_POINT('Ctrl Pts',(33.0185175726609,-29.5333899466912,18.7823836576175));
#29688=CARTESIAN_POINT('Ctrl Pts',(33.0006913488414,-29.533392180445,18.7823792819583));
#29689=CARTESIAN_POINT('Ctrl Pts',(32.9433364917302,-29.5333993674205,18.782365203525));
#29690=CARTESIAN_POINT('Ctrl Pts',(32.8893232017973,-29.5332829792511,18.7825476275079));
#29691=CARTESIAN_POINT('Ctrl Pts',(32.8382230275391,-29.5330947066424,18.7828441878577));
#29692=CARTESIAN_POINT('Ctrl Pts',(32.7810653123535,-29.5328841157333,18.7831759032042));
#29693=CARTESIAN_POINT('Ctrl Pts',(32.7275524566169,-29.532583390884,18.783650731462));
#29694=CARTESIAN_POINT('Ctrl Pts',(32.6770430178928,-29.5322363386496,18.7841988325575));
#29695=CARTESIAN_POINT('Ctrl Pts',(32.6227203151,-29.5318630853359,18.7847883131312));
#29696=CARTESIAN_POINT('Ctrl Pts',(32.5718714570977,-29.5314358212365,18.7854632228815));
#29697=CARTESIAN_POINT('Ctrl Pts',(32.5236533104256,-29.5309832901803,18.7861776881423));
#29698=CARTESIAN_POINT('Ctrl Pts',(32.4718100170294,-29.5304967368402,18.7869458684789));
#29699=CARTESIAN_POINT('Ctrl Pts',(32.4230076636111,-29.5299805545515,18.787760443828));
#29700=CARTESIAN_POINT('Ctrl Pts',(32.3761512171934,-29.5294487411367,18.7885990065863));
#29701=CARTESIAN_POINT('Ctrl Pts',(32.3248096591137,-29.5288660223986,18.7895178367975));
#29702=CARTESIAN_POINT('Ctrl Pts',(32.275804395008,-29.5282641700436,18.7904660498706));
#29703=CARTESIAN_POINT('Ctrl Pts',(32.2276418899935,-29.5276429422446,18.7914438965952));
#29704=CARTESIAN_POINT('Ctrl Pts',(32.1780484879536,-29.5270032579094,18.7924507949227));
#29705=CARTESIAN_POINT('Ctrl Pts',(32.1293485207497,-29.5263425803878,18.7934898288216));
#29706=CARTESIAN_POINT('Ctrl Pts',(32.0798596721975,-29.5256485080419,18.7945806299648));
#29707=CARTESIAN_POINT('Ctrl Pts',(32.0310319727755,-29.5249637081956,18.7956568584871));
#29708=CARTESIAN_POINT('Ctrl Pts',(31.9814363679959,-29.5242459918056,18.7967841293549));
#29709=CARTESIAN_POINT('Ctrl Pts',(31.9294088356327,-29.5234781937104,18.7979897024648));
#29710=CARTESIAN_POINT('Ctrl Pts',(31.8980169361537,-29.523014926676,18.7987171102077));
#29711=CARTESIAN_POINT('Ctrl Pts',(31.8657387723057,-29.5225333465275,18.7994731533958));
#29712=CARTESIAN_POINT('Ctrl Pts',(31.8321995506891,-29.5220297162343,18.8002637757389));
#29713=CARTESIAN_POINT('Ctrl Pts',(31.7313430769548,-29.5205152393626,18.8026412722264));
#29714=CARTESIAN_POINT('Ctrl Pts',(31.6280303063015,-29.5189339811,18.8051208616255));
#29715=CARTESIAN_POINT('Ctrl Pts',(31.5230436306592,-29.5173797888792,18.8075570016556));
#29716=CARTESIAN_POINT('Ctrl Pts',(31.4165412834618,-29.5158031590973,18.8100283117502));
#29717=CARTESIAN_POINT('Ctrl Pts',(31.3083161799734,-29.5142552687721,18.8124534992282));
#29718=CARTESIAN_POINT('Ctrl Pts',(31.1992361907463,-29.5128402023347,18.8146708525443));
#29719=CARTESIAN_POINT('Ctrl Pts',(31.1417800802781,-29.5120948391006,18.815838807345));
#29720=CARTESIAN_POINT('Ctrl Pts',(31.0840876501124,-29.5113863470818,18.816949067126));
#29721=CARTESIAN_POINT('Ctrl Pts',(31.02629146246,-29.5107292754508,18.817979046424));
#29722=CARTESIAN_POINT('Ctrl Pts',(30.9238422517517,-29.5095645538193,18.8198047821761));
#29723=CARTESIAN_POINT('Ctrl Pts',(30.8210652493993,-29.5085625954711,18.8213763518943));
#29724=CARTESIAN_POINT('Ctrl Pts',(30.7187655025438,-29.5078108353849,18.8225556928751));
#29725=CARTESIAN_POINT('Ctrl Pts',(30.6466529304574,-29.5072809088203,18.8233870274004));
#29726=CARTESIAN_POINT('Ctrl Pts',(30.5747782878161,-29.5068750511296,18.8240238694395));
#29727=CARTESIAN_POINT('Ctrl Pts',(30.5034323931868,-29.5066169475224,18.824428995823));
#29728=CARTESIAN_POINT('Ctrl Pts',(30.5006731165971,-29.506606965459,18.8244446639389));
#29729=CARTESIAN_POINT('Ctrl Pts',(30.4979146316512,-29.5065972035125,18.82445998689));
#29730=CARTESIAN_POINT('Ctrl Pts',(30.4951569508122,-29.5065876629556,18.8244749626663));
#29731=CARTESIAN_POINT('',(30.5,-31.0097594187194,16.229443021655));
#29732=CARTESIAN_POINT('Origin',(30.5,0.,0.));
#29733=CARTESIAN_POINT('Ctrl Pts',(30.5049076308142,-31.009123868732,16.2304573503027));
#29734=CARTESIAN_POINT('Ctrl Pts',(30.5973062294346,-31.0094328533549,16.2298682766553));
#29735=CARTESIAN_POINT('Ctrl Pts',(30.6890591585861,-31.009969267703,16.2288427503287));
#29736=CARTESIAN_POINT('Ctrl Pts',(30.780636436492,-31.0106763092386,16.2274919709622));
#29737=CARTESIAN_POINT('Ctrl Pts',(30.8441456090293,-31.0111666450937,16.2265552005995));
#29738=CARTESIAN_POINT('Ctrl Pts',(30.9075713010185,-31.0117394593185,16.2254611740685));
#29739=CARTESIAN_POINT('Ctrl Pts',(30.9710816356705,-31.012379837551,16.2242390174925));
#29740=CARTESIAN_POINT('Ctrl Pts',(31.0734991469997,-31.0134125190072,16.2222681534488));
#29741=CARTESIAN_POINT('Ctrl Pts',(31.1761345288069,-31.0146205155169,16.2199648111637));
#29742=CARTESIAN_POINT('Ctrl Pts',(31.2798100568472,-31.0159286966546,16.2174702047239));
#29743=CARTESIAN_POINT('Ctrl Pts',(31.382832629713,-31.017228638783,16.2149913094767));
#29744=CARTESIAN_POINT('Ctrl Pts',(31.4868822244331,-31.0186283615543,16.2123218973815));
#29745=CARTESIAN_POINT('Ctrl Pts',(31.5928140565593,-31.0200576696061,16.2095937955791));
#29746=CARTESIAN_POINT('Ctrl Pts',(31.6516194621104,-31.0208511142012,16.2080793581371));
#29747=CARTESIAN_POINT('Ctrl Pts',(31.7110057676088,-31.0216536678952,16.2065468518028));
#29748=CARTESIAN_POINT('Ctrl Pts',(31.771125977653,-31.0224523036439,16.205020814195));
#29749=CARTESIAN_POINT('Ctrl Pts',(31.8409078613428,-31.023379284885,16.2032495333099));
#29750=CARTESIAN_POINT('Ctrl Pts',(31.9056298453965,-31.0242198767435,16.2016434584278));
#29751=CARTESIAN_POINT('Ctrl Pts',(31.9658749467866,-31.0249744961547,16.2002018139143));
#29752=CARTESIAN_POINT('Ctrl Pts',(32.0341046687229,-31.025829129501,16.198569100183));
#29753=CARTESIAN_POINT('Ctrl Pts',(32.0965918298942,-31.0265740158191,16.1971462744692));
#29754=CARTESIAN_POINT('Ctrl Pts',(32.1542461945015,-31.0272242625031,16.195904238954));
#29755=CARTESIAN_POINT('Ctrl Pts',(32.2151665953522,-31.0279113447197,16.1945918439259));
#29756=CARTESIAN_POINT('Ctrl Pts',(32.2706916712566,-31.0284933558528,16.1934801514052));
#29757=CARTESIAN_POINT('Ctrl Pts',(32.3219582775166,-31.0289937114783,16.1925241206213));
#29758=CARTESIAN_POINT('Ctrl Pts',(32.3761916324787,-31.0295230221977,16.1915127652646));
#29759=CARTESIAN_POINT('Ctrl Pts',(32.4256599862244,-31.0299613681538,16.1906748064836));
#29760=CARTESIAN_POINT('Ctrl Pts',(32.4717693483807,-31.0303343957025,16.1899610544419));
#29761=CARTESIAN_POINT('Ctrl Pts',(32.5215332003086,-31.030736988296,16.1891907325537));
#29762=CARTESIAN_POINT('Ctrl Pts',(32.5673849287966,-31.0310638203076,16.1885644631732));
#29763=CARTESIAN_POINT('Ctrl Pts',(32.6111519417731,-31.0313387615314,16.1880367365759));
#29764=CARTESIAN_POINT('Ctrl Pts',(32.6551741210764,-31.0316153056917,16.1875059332765));
#29765=CARTESIAN_POINT('Ctrl Pts',(32.6970878717851,-31.0318395012597,16.1870745377529));
#29766=CARTESIAN_POINT('Ctrl Pts',(32.7388013470541,-31.0320241553174,16.18671857384));
#29767=CARTESIAN_POINT('Ctrl Pts',(32.7801521457895,-31.032207203906,16.1863657048444));
#29768=CARTESIAN_POINT('Ctrl Pts',(32.8213062770031,-31.0323516104908,16.1860865454659));
#29769=CARTESIAN_POINT('Ctrl Pts',(32.8641640035306,-31.0324560971771,16.1858844594635));
#29770=CARTESIAN_POINT('Ctrl Pts',(32.9038200784547,-31.0325527782704,16.1856974701314));
#29771=CARTESIAN_POINT('Ctrl Pts',(32.9449347772922,-31.0326154655021,16.1855761117062));
#29772=CARTESIAN_POINT('Ctrl Pts',(32.9890474705844,-31.0326287580453,16.1855509840874));
#29773=CARTESIAN_POINT('Ctrl Pts',(32.992608929339,-31.032629831225,16.1855489553974));
#29774=CARTESIAN_POINT('Ctrl Pts',(32.9961899495417,-31.0326305730128,16.1855475722578));
#29775=CARTESIAN_POINT('Ctrl Pts',(32.9997913521115,-31.0326309700539,16.185546860962));
#29776=CARTESIAN_POINT('Ctrl Pts',(33.0362292496772,-31.0326349871947,16.1855396642873));
#29777=CARTESIAN_POINT('Ctrl Pts',(33.0740922921121,-31.0326386992186,16.1855331333215));
#29778=CARTESIAN_POINT('Ctrl Pts',(33.1141439185632,-31.0326422490869,16.1855273500632));
#29779=CARTESIAN_POINT('Ctrl Pts',(33.2461674547435,-31.0326539506384,16.1855082865123));
#29780=CARTESIAN_POINT('Ctrl Pts',(33.3721931286569,-31.0326588963954,16.1855003220479));
#29781=CARTESIAN_POINT('Ctrl Pts',(33.4993879207449,-31.0326635427517,16.185492813855));
#29782=CARTESIAN_POINT('Ctrl Pts',(33.6627849160626,-31.0326695115548,16.185483168679));
#29783=CARTESIAN_POINT('Ctrl Pts',(33.828111247454,-31.0326749862723,16.1854742764645));
#29784=CARTESIAN_POINT('Ctrl Pts',(33.9929845306744,-31.0326833946006,16.1854606405094));
#29785=CARTESIAN_POINT('Ctrl Pts',(34.3227310971152,-31.032700211257,16.1854333685993));
#29786=CARTESIAN_POINT('Ctrl Pts',(34.6506654708719,-31.0327287623561,16.185387121727));
#29787=CARTESIAN_POINT('Ctrl Pts',(34.9792693636211,-31.0327480042371,16.1853559472169));
#29788=CARTESIAN_POINT('Ctrl Pts',(35.3078732563702,-31.0327672461181,16.1853247727069));
#29789=CARTESIAN_POINT('Ctrl Pts',(35.6371466681117,-31.0327771787811,16.185308670559));
#29790=CARTESIAN_POINT('Ctrl Pts',(35.9662682695209,-31.0327855310262,16.1852951338217));
#29791=CARTESIAN_POINT('Ctrl Pts',(36.2953898709301,-31.0327938832714,16.1852815970843));
#29792=CARTESIAN_POINT('Ctrl Pts',(36.624359662007,-31.0328006550989,16.1852706257574));
#29793=CARTESIAN_POINT('Ctrl Pts',(36.9532592751492,-31.0328145551759,16.185248102247));
#29794=CARTESIAN_POINT('Ctrl Pts',(38.1023262780261,-31.0328631174705,16.1851694125147));
#29795=CARTESIAN_POINT('Ctrl Pts',(39.2505367075415,-31.0329986853002,16.184949719878));
#29796=CARTESIAN_POINT('Ctrl Pts',(40.4000986012038,-31.0330322281526,16.1848953623403));
#29797=CARTESIAN_POINT('Ctrl Pts',(6.89999999997365,-11.0276873985587,-0.168526548676476));
#29798=CARTESIAN_POINT('Ctrl Pts',(6.99168932310453,-11.0290491215116,-0.107121039164008));
#29799=CARTESIAN_POINT('Ctrl Pts',(7.08383940291242,-11.0299018391088,-0.0458098125994616));
#29800=CARTESIAN_POINT('Ctrl Pts',(8.15761824498006,-11.0337651740187,0.664186592400576));
#29801=CARTESIAN_POINT('Ctrl Pts',(9.166078574375,-10.9699676285446,1.30870352701556));
#29802=CARTESIAN_POINT('Ctrl Pts',(11.2535171643192,-10.77603305676,2.47376106241927));
#29803=CARTESIAN_POINT('Ctrl Pts',(12.2576790632369,-10.6330057282434,3.00237606292525));
#29804=CARTESIAN_POINT('Ctrl Pts',(14.3563663857894,-10.3307260661656,3.94447005883399));
#29805=CARTESIAN_POINT('Ctrl Pts',(15.3658129161116,-10.1540434041659,4.36032593857961));
#29806=CARTESIAN_POINT('Ctrl Pts',(17.4727193021212,-9.82334300624283,5.08193366885832));
#29807=CARTESIAN_POINT('Ctrl Pts',(18.4888802671462,-9.6488422591121,5.39169279079136));
#29808=CARTESIAN_POINT('Ctrl Pts',(19.8473882183426,-9.45778984314827,5.72385817850078));
#29809=CARTESIAN_POINT('Ctrl Pts',(20.3451395577184,-9.38741838105894,5.84063156394592));
#29810=CARTESIAN_POINT('Ctrl Pts',(21.119864121141,-9.28201599203951,6.00690103675049));
#29811=CARTESIAN_POINT('Ctrl Pts',(21.9116430735679,-9.18172875488037,6.15921075032182));
#29812=CARTESIAN_POINT('Ctrl Pts',(22.4533884343747,-9.12054551137776,6.25063668203688));
#29813=CARTESIAN_POINT('Ctrl Pts',(22.8546099577479,-9.07881438233612,6.31320896750581));
#29814=CARTESIAN_POINT('Ctrl Pts',(23.1058218650382,-9.05298395410356,6.35118260107245));
#29815=CARTESIAN_POINT('Ctrl Pts',(23.6175153199789,-9.00245668094438,6.42382403760964));
#29816=CARTESIAN_POINT('Ctrl Pts',(24.1364702886545,-8.95485371029556,6.49007583237978));
#29817=CARTESIAN_POINT('Ctrl Pts',(24.6629181373247,-8.91145225308146,6.54944423929281));
#29818=CARTESIAN_POINT('Ctrl Pts',(25.0606678571037,-8.88140293076166,6.59024788291776));
#29819=CARTESIAN_POINT('Ctrl Pts',(25.3945416155883,-8.85873533710267,6.62099228309712));
#29820=CARTESIAN_POINT('Ctrl Pts',(25.6627586119465,-8.84221409068036,6.64352323130155));
#29821=CARTESIAN_POINT('Ctrl Pts',(25.7972076165426,-8.83452216013017,6.65408072739389));
#29822=CARTESIAN_POINT('Ctrl Pts',(26.3824137782947,-8.80240169886326,6.69837697633856));
#29823=CARTESIAN_POINT('Ctrl Pts',(27.4369717967156,-8.76563881905857,6.74704662082205));
#29824=CARTESIAN_POINT('Ctrl Pts',(28.4593635146678,-8.74917816753953,6.76713562537257));
#29825=CARTESIAN_POINT('Ctrl Pts',(29.0427481469893,-8.73952198264548,6.77974505298725));
#29826=CARTESIAN_POINT('Ctrl Pts',(29.2174939164953,-8.73701514175021,6.78306424239326));
#29827=CARTESIAN_POINT('Ctrl Pts',(29.560704833228,-8.73336568489196,6.78786835107264));
#29828=CARTESIAN_POINT('Ctrl Pts',(29.9899637006215,-8.73093988338432,6.7910625393568));
#29829=CARTESIAN_POINT('Ctrl Pts',(30.5003627545719,-8.73068255391876,6.79139754852951));
#29830=CARTESIAN_POINT('Ctrl Pts',(31.5152290141056,-8.73381293113862,6.78728755019412));
#29831=CARTESIAN_POINT('Ctrl Pts',(32.346385618228,-8.74063107149336,6.77838967797267));
#29832=CARTESIAN_POINT('Ctrl Pts',(33.1616392309915,-8.74062146997074,6.77840182636606));
#29833=CARTESIAN_POINT('Ctrl Pts',(33.4928689770884,-8.74062052628884,6.77840284181041));
#29834=CARTESIAN_POINT('Ctrl Pts',(33.9856875201801,-8.74061852020513,6.77840526161275));
#29835=CARTESIAN_POINT('Ctrl Pts',(34.479956929609,-8.74061713883255,6.7784068708528));
#29836=CARTESIAN_POINT('Ctrl Pts',(35.1382080085716,-8.74061527897129,6.778409075901));
#29837=CARTESIAN_POINT('Ctrl Pts',(35.9613703496106,-8.74061266742265,6.7784121544085));
#29838=CARTESIAN_POINT('Ctrl Pts',(37.9364530322258,-8.74060999527037,6.77841531264166));
#29839=CARTESIAN_POINT('Ctrl Pts',(39.5833333333333,-8.74059347982545,6.77843480602319));
#29840=CARTESIAN_POINT('Ctrl Pts',(40.9,-8.74059347982545,6.77843480602319));
#29841=CARTESIAN_POINT('Ctrl Pts',(6.65963435785827,-15.5421695279122,-0.914290744262173));
#29842=CARTESIAN_POINT('Ctrl Pts',(6.7513219377677,-15.5478000748543,-0.827664097498932));
#29843=CARTESIAN_POINT('Ctrl Pts',(6.84347928233528,-15.552705535984,-0.741125593738216));
#29844=CARTESIAN_POINT('Ctrl Pts',(7.91768245328712,-15.6010379387116,0.260912141468049));
#29845=CARTESIAN_POINT('Ctrl Pts',(8.92716941433653,-15.5498192559038,1.17337698529147));
#29846=CARTESIAN_POINT('Ctrl Pts',(11.0226592374973,-15.3445243615387,2.83406080960164));
#29847=CARTESIAN_POINT('Ctrl Pts',(12.0289222513091,-15.174357849642,3.58841078209879));
#29848=CARTESIAN_POINT('Ctrl Pts',(14.1441326723881,-14.8006104561251,4.94359337154892));
#29849=CARTESIAN_POINT('Ctrl Pts',(15.1576282381579,-14.5754503759515,5.54148857510365));
#29850=CARTESIAN_POINT('Ctrl Pts',(17.2903455772588,-14.1464770374584,6.58799131832697));
#29851=CARTESIAN_POINT('Ctrl Pts',(18.3126565164254,-13.9174993841978,7.03615941125111));
#29852=CARTESIAN_POINT('Ctrl Pts',(19.6943886098338,-13.6636269320846,7.52140607073201));
#29853=CARTESIAN_POINT('Ctrl Pts',(20.1963997689949,-13.5705283753709,7.69105316997363));
#29854=CARTESIAN_POINT('Ctrl Pts',(20.9820476354982,-13.4299327266448,7.9338457745664));
#29855=CARTESIAN_POINT('Ctrl Pts',(21.7860719497258,-13.2956844767357,8.15658902665418));
#29856=CARTESIAN_POINT('Ctrl Pts',(22.337913112583,-13.2134517389134,8.29065006793576));
#29857=CARTESIAN_POINT('Ctrl Pts',(22.7470242103181,-13.1573095336481,8.38247788994951));
#29858=CARTESIAN_POINT('Ctrl Pts',(23.0012838485785,-13.1227286630507,8.43794163853499));
#29859=CARTESIAN_POINT('Ctrl Pts',(23.5207560883433,-13.0548326909721,8.54431696039333));
#29860=CARTESIAN_POINT('Ctrl Pts',(24.0478165510038,-12.9907421048667,8.6413962979357));
#29861=CARTESIAN_POINT('Ctrl Pts',(24.5834508086859,-12.9321620155412,8.72854413973127));
#29862=CARTESIAN_POINT('Ctrl Pts',(24.9884814516725,-12.8915554305395,8.78849484453726));
#29863=CARTESIAN_POINT('Ctrl Pts',(25.3288761766951,-12.8608881947636,8.83370307828864));
#29864=CARTESIAN_POINT('Ctrl Pts',(25.6025411192578,-12.8385223247212,8.86685769924433));
#29865=CARTESIAN_POINT('Ctrl Pts',(25.73979094788,-12.8281059147068,8.88239886754129));
#29866=CARTESIAN_POINT('Ctrl Pts',(26.3376341743262,-12.7845927902169,8.94762125697));
#29867=CARTESIAN_POINT('Ctrl Pts',(27.4152541470277,-12.7347557261565,9.01924678134855));
#29868=CARTESIAN_POINT('Ctrl Pts',(28.4429499146133,-12.7126826807293,9.04845162691347));
#29869=CARTESIAN_POINT('Ctrl Pts',(29.0259735124592,-12.6997781188676,9.06676270853369));
#29870=CARTESIAN_POINT('Ctrl Pts',(29.2042686472714,-12.6963761571783,9.07165323227908));
#29871=CARTESIAN_POINT('Ctrl Pts',(29.5518704410187,-12.6914548812216,9.07868995890017));
#29872=CARTESIAN_POINT('Ctrl Pts',(29.9865605489545,-12.6881801081657,9.08337117217634));
#29873=CARTESIAN_POINT('Ctrl Pts',(30.5013181269547,-12.6878363073061,9.08385656546482));
#29874=CARTESIAN_POINT('Ctrl Pts',(31.5221463919968,-12.692041007367,9.07785413361798));
#29875=CARTESIAN_POINT('Ctrl Pts',(32.3518561954418,-12.7011306199596,9.06494609970922));
#29876=CARTESIAN_POINT('Ctrl Pts',(33.1604291208178,-12.7011133788388,9.06496486760967));
#29877=CARTESIAN_POINT('Ctrl Pts',(33.4925190590671,-12.7011117013819,9.06496624091916));
#29878=CARTESIAN_POINT('Ctrl Pts',(33.9849476449336,-12.7011081104537,9.06496984963707));
#29879=CARTESIAN_POINT('Ctrl Pts',(34.4794328720439,-12.7011056432242,9.06497218408094));
#29880=CARTESIAN_POINT('Ctrl Pts',(35.1376484147356,-12.7011023177079,9.06497542847038));
#29881=CARTESIAN_POINT('Ctrl Pts',(35.9609115545804,-12.7010976498373,9.06497993729913));
#29882=CARTESIAN_POINT('Ctrl Pts',(37.9360269889122,-12.7010928728514,9.06498457262957));
#29883=CARTESIAN_POINT('Ctrl Pts',(39.5833333333333,-12.701063350837,9.06501315216909));
#29884=CARTESIAN_POINT('Ctrl Pts',(40.9,-12.701063350837,9.06501315216909));
#29885=CARTESIAN_POINT('Ctrl Pts',(6.47499700785697,-23.4452408248497,-2.19830497971403));
#29886=CARTESIAN_POINT('Ctrl Pts',(6.56578730943226,-23.4579749263878,-2.06870104448402));
#29887=CARTESIAN_POINT('Ctrl Pts',(6.65702462351448,-23.4696212195475,-1.93921681262018));
#29888=CARTESIAN_POINT('Ctrl Pts',(7.72175305647137,-23.5924911125725,-0.437116228582369));
#29889=CARTESIAN_POINT('Ctrl Pts',(8.72281885180382,-23.562968194923,0.93768014090861));
#29890=CARTESIAN_POINT('Ctrl Pts',(10.7949492361907,-23.3400040819286,3.44026704375966));
#29891=CARTESIAN_POINT('Ctrl Pts',(11.7960921547002,-23.1244337632637,4.58695803318564));
#29892=CARTESIAN_POINT('Ctrl Pts',(13.8958332645754,-22.6316660291752,6.64967501166335));
#29893=CARTESIAN_POINT('Ctrl Pts',(14.90655296446,-22.3241101177864,7.56603922905964));
#29894=CARTESIAN_POINT('Ctrl Pts',(17.0410718223018,-21.7268962408645,9.17994203101701));
#29895=CARTESIAN_POINT('Ctrl Pts',(18.0654584152639,-21.4035033181339,9.87337110606603));
#29896=CARTESIAN_POINT('Ctrl Pts',(19.4655915747002,-21.0382396447148,10.6334003056859));
#29897=CARTESIAN_POINT('Ctrl Pts',(19.9714665789849,-20.9051898734593,10.8971713557552));
#29898=CARTESIAN_POINT('Ctrl Pts',(20.7678306953019,-20.7020007981629,11.2774874271219));
#29899=CARTESIAN_POINT('Ctrl Pts',(21.5858101282049,-20.5068169170513,11.6277425327431));
#29900=CARTESIAN_POINT('Ctrl Pts',(22.1506096305012,-20.3863209191721,11.8398576536859));
#29901=CARTESIAN_POINT('Ctrl Pts',(22.5704199924792,-20.3038374401208,11.9854171937934));
#29902=CARTESIAN_POINT('Ctrl Pts',(22.8289065956908,-20.2535349220293,12.0724797867542));
#29903=CARTESIAN_POINT('Ctrl Pts',(23.3593853239227,-20.1541718428526,12.2402701514192));
#29904=CARTESIAN_POINT('Ctrl Pts',(23.8985486588058,-20.0601195256969,12.3936552183108));
#29905=CARTESIAN_POINT('Ctrl Pts',(24.4483714419234,-19.9737860075935,12.5318087211868));
#29906=CARTESIAN_POINT('Ctrl Pts',(24.8648919059684,-19.9138158121696,12.6269879069122));
#29907=CARTESIAN_POINT('Ctrl Pts',(25.2158455690757,-19.8684065291875,12.6989260386039));
#29908=CARTESIAN_POINT('Ctrl Pts',(25.4984343217207,-19.8352396029271,12.7517388774024));
#29909=CARTESIAN_POINT('Ctrl Pts',(25.6403132052064,-19.8197769054431,12.7765150372189));
#29910=CARTESIAN_POINT('Ctrl Pts',(26.2592160414081,-19.7551088720197,12.8806146990981));
#29911=CARTESIAN_POINT('Ctrl Pts',(27.3768446537005,-19.6810635867321,12.994818613011));
#29912=CARTESIAN_POINT('Ctrl Pts',(28.4139434096805,-19.6491350216629,13.0400692167481));
#29913=CARTESIAN_POINT('Ctrl Pts',(28.9963902080608,-19.6305403234117,13.0683908406421));
#29914=CARTESIAN_POINT('Ctrl Pts',(29.180878403009,-19.6254773891901,13.0761959447011));
#29915=CARTESIAN_POINT('Ctrl Pts',(29.5361613355606,-19.6182496508377,13.0872826938044));
#29916=CARTESIAN_POINT('Ctrl Pts',(29.9803701492975,-19.613426667661,13.0946820190499));
#29917=CARTESIAN_POINT('Ctrl Pts',(30.5027645652051,-19.6129305494837,13.0954354949456));
#29918=CARTESIAN_POINT('Ctrl Pts',(31.5340441540658,-19.619049331486,13.0860712826798));
#29919=CARTESIAN_POINT('Ctrl Pts',(32.361293357075,-19.6320590316267,13.0662692307128));
#29920=CARTESIAN_POINT('Ctrl Pts',(33.1582057305723,-19.6320151866218,13.0663352315321));
#29921=CARTESIAN_POINT('Ctrl Pts',(33.4918052160808,-19.6320107493385,13.0663415440457));
#29922=CARTESIAN_POINT('Ctrl Pts',(33.9835585756086,-19.6320015037508,13.0663552182345));
#29923=CARTESIAN_POINT('Ctrl Pts',(34.4784268233885,-19.6319950964453,13.0663645784942));
#29924=CARTESIAN_POINT('Ctrl Pts',(35.1365871092733,-19.6319864972548,13.0663772185058));
#29925=CARTESIAN_POINT('Ctrl Pts',(35.9600364992905,-19.631974409872,13.0663949498221));
#29926=CARTESIAN_POINT('Ctrl Pts',(37.935219274406,-19.6319620479287,13.0664131007023));
#29927=CARTESIAN_POINT('Ctrl Pts',(39.5833333333333,-19.6318856251071,13.0665252579244));
#29928=CARTESIAN_POINT('Ctrl Pts',(40.9,-19.6318856251071,13.0665252579244));
#29929=CARTESIAN_POINT('Ctrl Pts',(6.39840282685635,-31.3636440442398,-3.36386536347516));
#29930=CARTESIAN_POINT('Ctrl Pts',(6.48879582230594,-31.3828291635015,-3.19164073503352));
#29931=CARTESIAN_POINT('Ctrl Pts',(6.57961766269115,-31.4005708453189,-3.01959979440376));
#29932=CARTESIAN_POINT('Ctrl Pts',(7.64032554406628,-31.5903744166847,-1.0214771742003));
#29933=CARTESIAN_POINT('Ctrl Pts',(8.63867106160224,-31.5754173772483,0.811297807542586));
#29934=CARTESIAN_POINT('Ctrl Pts',(10.6964316380006,-31.3261515036618,4.13353910931635));
#29935=CARTESIAN_POINT('Ctrl Pts',(11.6947290441859,-31.0615534966588,5.66648609020814));
#29936=CARTESIAN_POINT('Ctrl Pts',(13.7762263687762,-30.4500782098735,8.40637303045944));
#29937=CARTESIAN_POINT('Ctrl Pts',(14.7826773906134,-30.0602543273649,9.63313444048393));
#29938=CARTESIAN_POINT('Ctrl Pts',(16.8988982405362,-29.3025485110513,11.7841821047735));
#29939=CARTESIAN_POINT('Ctrl Pts',(17.9188263508252,-28.8873179990429,12.7156877051221));
#29940=CARTESIAN_POINT('Ctrl Pts',(19.3136620513073,-28.4161739072999,13.7379571249216));
#29941=CARTESIAN_POINT('Ctrl Pts',(19.8189838754924,-28.2441169214324,14.0939758439964));
#29942=CARTESIAN_POINT('Ctrl Pts',(20.6150001505384,-27.9803060047161,14.6080226620617));
#29943=CARTESIAN_POINT('Ctrl Pts',(21.4350390683302,-27.7255808745093,15.0835002485375));
#29944=CARTESIAN_POINT('Ctrl Pts',(22.0037815933943,-27.5672808319298,15.3731124530265));
#29945=CARTESIAN_POINT('Ctrl Pts',(22.4278524797961,-27.4584837184542,15.5725968076267));
#29946=CARTESIAN_POINT('Ctrl Pts',(22.6881478873211,-27.3924576319504,15.6914147925573));
#29947=CARTESIAN_POINT('Ctrl Pts',(23.2238106344271,-27.2614400973337,15.921268075794));
#29948=CARTESIAN_POINT('Ctrl Pts',(23.7696978745005,-27.1369441741205,16.1321064141348));
#29949=CARTESIAN_POINT('Ctrl Pts',(24.3285206801333,-27.022064166134,16.3229204338608));
#29950=CARTESIAN_POINT('Ctrl Pts',(24.7529653140504,-26.9419913350362,16.4547973514759));
#29951=CARTESIAN_POINT('Ctrl Pts',(25.1117719491785,-26.8811074137509,16.554863796012));
#29952=CARTESIAN_POINT('Ctrl Pts',(25.4013553254924,-26.836506870562,16.6285198436922));
#29953=CARTESIAN_POINT('Ctrl Pts',(25.5469791293171,-26.8156703264605,16.6631374284086));
#29954=CARTESIAN_POINT('Ctrl Pts',(26.1832292898987,-26.7283606594225,16.8088431266916));
#29955=CARTESIAN_POINT('Ctrl Pts',(27.3386864567867,-26.6279357083785,16.9694451045118));
#29956=CARTESIAN_POINT('Ctrl Pts',(28.3853135289695,-26.5860990135272,17.0308214554548));
#29957=CARTESIAN_POINT('Ctrl Pts',(28.9671494424549,-26.5618106446087,17.0691585340134));
#29958=CARTESIAN_POINT('Ctrl Pts',(29.1577497745605,-26.5549253720648,17.0801578267592));
#29959=CARTESIAN_POINT('Ctrl Pts',(29.5206667657,-26.5452518307316,17.0955352214361));
#29960=CARTESIAN_POINT('Ctrl Pts',(29.9743609805096,-26.5387742795118,17.1058350294713));
#29961=CARTESIAN_POINT('Ctrl Pts',(30.5043929318942,-26.5381249904399,17.1068574997828));
#29962=CARTESIAN_POINT('Ctrl Pts',(31.5460952643805,-26.54622028874,17.0940221862975));
#29963=CARTESIAN_POINT('Ctrl Pts',(32.3708379684223,-26.5630634070367,17.0674707682792));
#29964=CARTESIAN_POINT('Ctrl Pts',(33.1560659395073,-26.5629740474711,17.0676145179389));
#29965=CARTESIAN_POINT('Ctrl Pts',(33.4911715963805,-26.5629648505727,17.0676289242213));
#29966=CARTESIAN_POINT('Ctrl Pts',(33.9822440621776,-26.5629459056337,17.0676591426917));
#29967=CARTESIAN_POINT('Ctrl Pts',(34.4774910986523,-26.5629327280363,17.0676800396183));
#29968=CARTESIAN_POINT('Ctrl Pts',(35.1355906516825,-26.5629150749568,17.0677081152075));
#29969=CARTESIAN_POINT('Ctrl Pts',(35.9592185001008,-26.5628902459987,17.0677475655254));
#29970=CARTESIAN_POINT('Ctrl Pts',(37.9344606912907,-26.5628648600815,17.067787918432));
#29971=CARTESIAN_POINT('Ctrl Pts',(39.5833333333333,-26.5627078993772,17.0680373636797));
#29972=CARTESIAN_POINT('Ctrl Pts',(40.9,-26.5627078993772,17.0680373636797));
#29973=CARTESIAN_POINT('Ctrl Pts',(6.37427268165564,-34.7583359408307,-3.85496595036637));
#29974=CARTESIAN_POINT('Ctrl Pts',(6.46448755772838,-34.7802475524424,-3.66446375246399));
#29975=CARTESIAN_POINT('Ctrl Pts',(6.55512331969025,-34.8005635888992,-3.47417181608893));
#29976=CARTESIAN_POINT('Ctrl Pts',(7.61410548625795,-35.0185788676572,-1.26339052014805));
#29977=CARTESIAN_POINT('Ctrl Pts',(8.61145388480624,-35.0093532870147,0.765602457207686));
#29978=CARTESIAN_POINT('Ctrl Pts',(10.6635149436019,-34.747974440135,4.43910992978124));
#29979=CARTESIAN_POINT('Ctrl Pts',(11.6608017032625,-34.4619345886989,6.13747453196185));
#29980=CARTESIAN_POINT('Ctrl Pts',(13.7353542747945,-33.7990269238398,9.16685810272323));
#29981=CARTESIAN_POINT('Ctrl Pts',(14.7402715202386,-33.3736740493576,10.5262979552789));
#29982=CARTESIAN_POINT('Ctrl Pts',(16.8491677832147,-32.5473921410153,12.9054531131771));
#29983=CARTESIAN_POINT('Ctrl Pts',(17.8672809631136,-32.092886041556,13.9382203331611));
#29984=CARTESIAN_POINT('Ctrl Pts',(19.2587625104673,-31.577179869867,15.0707179501981));
#29985=CARTESIAN_POINT('Ctrl Pts',(19.7635899403542,-31.3885503410944,15.4658689812884));
#29986=CARTESIAN_POINT('Ctrl Pts',(20.5586991602297,-31.0991569516509,16.0362969262867));
#29987=CARTESIAN_POINT('Ctrl Pts',(21.3785272493019,-30.819343278526,16.564533786793));
#29988=CARTESIAN_POINT('Ctrl Pts',(21.9479176287994,-30.6451300260617,16.8867906552356));
#29989=CARTESIAN_POINT('Ctrl Pts',(22.3729695502115,-30.525234440013,17.1090467735268));
#29990=CARTESIAN_POINT('Ctrl Pts',(22.6337096028249,-30.45253373981,17.2413581349254));
#29991=CARTESIAN_POINT('Ctrl Pts',(23.170751986421,-30.3080867629257,17.4975676797997));
#29992=CARTESIAN_POINT('Ctrl Pts',(23.7186485394885,-30.1706268071311,17.7328951431606));
#29993=CARTESIAN_POINT('Ctrl Pts',(24.2804077704386,-30.0435395405948,17.9462491604951));
#29994=CARTESIAN_POINT('Ctrl Pts',(24.7075732751059,-29.9548357769836,18.093896808302));
#29995=CARTESIAN_POINT('Ctrl Pts',(25.0692008252976,-29.8872739715488,18.2061112471098));
#29996=CARTESIAN_POINT('Ctrl Pts',(25.3613771492326,-29.8377189043885,18.2888047627701));
#29997=CARTESIAN_POINT('Ctrl Pts',(25.5084154817282,-29.8145466170754,18.3277015544067));
#29998=CARTESIAN_POINT('Ctrl Pts',(26.1512870025445,-29.7173716879778,18.4915385207408));
#29999=CARTESIAN_POINT('Ctrl Pts',(27.3223884400174,-29.6052740416532,18.6726738474943));
#30000=CARTESIAN_POINT('Ctrl Pts',(28.3731396048322,-29.5591775248211,18.7409825767552));
#30001=CARTESIAN_POINT('Ctrl Pts',(28.9547046473316,-29.532448097728,18.7836137746099));
#30002=CARTESIAN_POINT('Ctrl Pts',(29.1479037067739,-29.5247529606445,18.7960320303042));
#30003=CARTESIAN_POINT('Ctrl Pts',(29.5140802367922,-29.5140058211202,18.8132921881814));
#30004=CARTESIAN_POINT('Ctrl Pts',(29.9718311305159,-29.5067996680498,18.8248686377543));
#30005=CARTESIAN_POINT('Ctrl Pts',(30.505136527612,-29.5060845192012,18.8260067178223));
#30006=CARTESIAN_POINT('Ctrl Pts',(31.5512984754482,-29.515038303799,18.8116639693829));
#30007=CARTESIAN_POINT('Ctrl Pts',(32.3749555043413,-29.5335081969199,18.7822473977007));
#30008=CARTESIAN_POINT('Ctrl Pts',(33.1551698865007,-29.5333957726549,18.7824304492384));
#30009=CARTESIAN_POINT('Ctrl Pts',(33.4909201969602,-29.533384156022,18.782448957068));
#30010=CARTESIAN_POINT('Ctrl Pts',(33.981699427726,-29.5333602907363,18.7824875453788));
#30011=CARTESIAN_POINT('Ctrl Pts',(34.4771077390558,-29.533343676228,18.7825142819534));
#30012=CARTESIAN_POINT('Ctrl Pts',(35.1351798881798,-29.5333214285967,18.7825501686284));
#30013=CARTESIAN_POINT('Ctrl Pts',(35.958882261465,-29.5332901329543,18.7826006107083));
#30014=CARTESIAN_POINT('Ctrl Pts',(37.9341479260215,-29.5332581373787,18.7826521993715));
#30015=CARTESIAN_POINT('Ctrl Pts',(39.5833333333333,-29.5330603026358,18.7829711232891));
#30016=CARTESIAN_POINT('Ctrl Pts',(40.9,-29.5330603026358,18.7829711232891));
#30017=CARTESIAN_POINT('',(40.9,-27.7992994660114,17.7819838375536));
#30018=CARTESIAN_POINT('Ctrl Pts',(40.9,-27.7992994660114,17.7819838375536));
#30019=CARTESIAN_POINT('Ctrl Pts',(40.9,-28.2327406817405,18.0322312401327));
#30020=CARTESIAN_POINT('Ctrl Pts',(40.9,-28.6661818974695,18.2824786427117));
#30021=CARTESIAN_POINT('Ctrl Pts',(40.9,-29.0996231131986,18.5327260452908));
#30022=CARTESIAN_POINT('',(38.,-27.7992994660114,17.7819838375536));
#30023=CARTESIAN_POINT('Ctrl Pts',(38.,-27.7992994660114,17.7819838375536));
#30024=CARTESIAN_POINT('Ctrl Pts',(38.9666666666667,-27.7992994660114,17.7819838375536));
#30025=CARTESIAN_POINT('Ctrl Pts',(39.9333333333333,-27.7992994660114,17.7819838375536));
#30026=CARTESIAN_POINT('Ctrl Pts',(40.9,-27.7992994660114,17.7819838375536));
#30027=CARTESIAN_POINT('Ctrl Pts',(37.4972396727241,-27.2792903521173,17.4814222894395));
#30028=CARTESIAN_POINT('Ctrl Pts',(37.6643013627082,-27.4529632561665,17.581705123587));
#30029=CARTESIAN_POINT('Ctrl Pts',(37.8311425499703,-27.6263785906013,17.681842059693));
#30030=CARTESIAN_POINT('Ctrl Pts',(37.9976538234737,-27.7994318724651,17.7817719425585));
#30031=CARTESIAN_POINT('',(6.9,-29.9143312995417,-2.26556458774884));
#30032=CARTESIAN_POINT('Ctrl Pts',(6.9,-29.9143312995417,-2.26556458774883));
#30033=CARTESIAN_POINT('Ctrl Pts',(6.9,-27.3056186709172,-2.00382962437802));
#30034=CARTESIAN_POINT('Ctrl Pts',(6.90000000000115,-24.6693701926632,-1.73285728374608));
#30035=CARTESIAN_POINT('Ctrl Pts',(6.90000000000115,-18.7182130985667,-1.09593289590079));
#30036=CARTESIAN_POINT('Ctrl Pts',(6.9,-14.7845781982083,-0.65479489350369));
#30037=CARTESIAN_POINT('Ctrl Pts',(6.9,-11.02768739857,-0.168526548660246));
#30038=CARTESIAN_POINT('',(22.9245129145126,-27.5141512254856,15.8853026165582));
#30039=CARTESIAN_POINT('Ctrl Pts',(22.9245129145126,-27.5141512254856,15.8853026165582));
#30040=CARTESIAN_POINT('Ctrl Pts',(22.7202811020963,-27.5032269692373,15.7659233420327));
#30041=CARTESIAN_POINT('Ctrl Pts',(22.5089075447093,-27.4959054260063,15.6398559109135));
#30042=CARTESIAN_POINT('Ctrl Pts',(22.2913349439917,-27.4928730439354,15.5073965833875));
#30043=CARTESIAN_POINT('Ctrl Pts',(21.4451770585294,-27.4810798586144,14.992251275019));
#30044=CARTESIAN_POINT('Ctrl Pts',(20.522095155667,-27.5650257717264,14.3509960808547));
#30045=CARTESIAN_POINT('Ctrl Pts',(19.7671428819542,-27.6762399607748,13.7859304181016));
#30046=CARTESIAN_POINT('Ctrl Pts',(19.5194773058393,-27.7127242885422,13.6005580206914));
#30047=CARTESIAN_POINT('Ctrl Pts',(19.2865716386092,-27.7514615171004,13.4218723240252));
#30048=CARTESIAN_POINT('Ctrl Pts',(19.0728538401323,-27.7894004949774,13.2552441975238));
#30049=CARTESIAN_POINT('Ctrl Pts',(18.7028555998035,-27.8550822264681,12.9667697979459));
#30050=CARTESIAN_POINT('Ctrl Pts',(18.4144703596235,-27.9152561335183,12.7292901983115));
#30051=CARTESIAN_POINT('Ctrl Pts',(18.0642874871537,-27.9946062155751,12.4284122845046));
#30052=CARTESIAN_POINT('Ctrl Pts',(17.4420927116721,-28.1355931408966,11.8938211301512));
#30053=CARTESIAN_POINT('Ctrl Pts',(16.7224564418218,-28.3254287038798,11.2282910364347));
#30054=CARTESIAN_POINT('Ctrl Pts',(15.9202806616111,-28.5439924969395,10.4246142212493));
#30055=CARTESIAN_POINT('Ctrl Pts',(15.4090529834519,-28.6832834892781,9.91242993152971));
#30056=CARTESIAN_POINT('Ctrl Pts',(14.8739602945717,-28.8377564730262,9.33532862360362));
#30057=CARTESIAN_POINT('Ctrl Pts',(14.3169794331159,-28.9944199787762,8.69171842999422));
#30058=CARTESIAN_POINT('Ctrl Pts',(13.8864206762839,-29.1155243989539,8.19419324731461));
#30059=CARTESIAN_POINT('Ctrl Pts',(13.3867890027806,-29.2546860278643,7.59173852185157));
#30060=CARTESIAN_POINT('Ctrl Pts',(12.8146824059514,-29.3960736315876,6.86770373383358));
#30061=CARTESIAN_POINT('Ctrl Pts',(12.2526665517594,-29.5349674589251,6.15643937836574));
#30062=CARTESIAN_POINT('Ctrl Pts',(11.6379478462802,-29.678401911158,5.3206691843855));
#30063=CARTESIAN_POINT('Ctrl Pts',(10.9739250490306,-29.7956367796097,4.35448584003977));
#30064=CARTESIAN_POINT('Ctrl Pts',(10.5683455447962,-29.8672428449776,3.76434923114257));
#30065=CARTESIAN_POINT('Ctrl Pts',(10.1437415406955,-29.9275397584159,3.12422765605926));
#30066=CARTESIAN_POINT('Ctrl Pts',(9.74137929176525,-29.9670595377668,2.50486371218385));
#30067=CARTESIAN_POINT('Ctrl Pts',(8.72285779294234,-30.0670981099855,0.937033991304209));
#30068=CARTESIAN_POINT('Ctrl Pts',(7.81323138778195,-30.0560666286387,-0.638451825302673));
#30069=CARTESIAN_POINT('Ctrl Pts',(6.9,-29.9143312995417,-2.26556458774883));
#30070=CARTESIAN_POINT('Ctrl Pts',(30.5,-29.5059919176187,18.8254200738635));
#30071=CARTESIAN_POINT('Ctrl Pts',(29.9560179420816,-29.293615660989,18.7064245513841));
#30072=CARTESIAN_POINT('Ctrl Pts',(29.4152668325132,-29.0895919906434,18.5734800115823));
#30073=CARTESIAN_POINT('Ctrl Pts',(28.8740459957565,-28.9020067835811,18.4125151878636));
#30074=CARTESIAN_POINT('Ctrl Pts',(28.353527792344,-28.7215970352203,18.2577075471291));
#30075=CARTESIAN_POINT('Ctrl Pts',(27.8179515912467,-28.533139934629,18.1008601332298));
#30076=CARTESIAN_POINT('Ctrl Pts',(27.2695051149491,-28.3565719042575,17.9186544331585));
#30077=CARTESIAN_POINT('Ctrl Pts',(26.9554553615883,-28.2554660556725,17.8143203592948));
#30078=CARTESIAN_POINT('Ctrl Pts',(26.6378099296971,-28.1585101274347,17.7019284120276));
#30079=CARTESIAN_POINT('Ctrl Pts',(26.3179304017917,-28.0701057587103,17.5778023417279));
#30080=CARTESIAN_POINT('Ctrl Pts',(26.1078196745982,-28.012037940737,17.4962709631332));
#30081=CARTESIAN_POINT('Ctrl Pts',(25.8967402232745,-27.9576659729224,17.409683568055));
#30082=CARTESIAN_POINT('Ctrl Pts',(25.6850706236774,-27.9082593406129,17.3169960819306));
#30083=CARTESIAN_POINT('Ctrl Pts',(25.6562210027417,-27.9015254373195,17.3043631915899));
#30084=CARTESIAN_POINT('Ctrl Pts',(25.6277737638215,-27.8949772388532,17.2918013331136));
#30085=CARTESIAN_POINT('Ctrl Pts',(25.5983858063598,-27.8883138877393,17.2787081509674));
#30086=CARTESIAN_POINT('Ctrl Pts',(25.1249357452756,-27.7809650188704,17.067772501732));
#30087=CARTESIAN_POINT('Ctrl Pts',(24.1510084067019,-27.5797558484168,16.6022239440147));
#30088=CARTESIAN_POINT('Ctrl Pts',(22.9245129145126,-27.5141512254856,15.8853026165582));
#30089=CARTESIAN_POINT('Origin',(40.65,0.,0.));
#30090=CARTESIAN_POINT('',(40.4,-34.9678423698117,-1.5));
#30091=CARTESIAN_POINT('',(40.9,-34.4673758792282,-1.5));
#30092=CARTESIAN_POINT('Ctrl Pts',(40.4,-34.9678423698117,-1.5));
#30093=CARTESIAN_POINT('Ctrl Pts',(40.5666590142081,-34.8010300902437,-1.5));
#30094=CARTESIAN_POINT('Ctrl Pts',(40.7333430453063,-34.6341905783534,-1.5));
#30095=CARTESIAN_POINT('Ctrl Pts',(40.9,-34.4673758792282,-1.5));
#30096=CARTESIAN_POINT('',(40.9,-34.4673758792282,1.50000000000002));
#30097=CARTESIAN_POINT('Origin',(40.9,0.,0.));
#30098=CARTESIAN_POINT('',(40.4,-34.9678423698117,1.5));
#30099=CARTESIAN_POINT('Ctrl Pts',(40.9,-34.4673758792282,1.5));
#30100=CARTESIAN_POINT('Ctrl Pts',(40.7333430446438,-34.6341905790166,1.5));
#30101=CARTESIAN_POINT('Ctrl Pts',(40.5666590131148,-34.801030091338,1.5));
#30102=CARTESIAN_POINT('Ctrl Pts',(40.4,-34.9678423698117,1.5));
#30103=CARTESIAN_POINT('Origin',(40.4,0.,0.));
#30104=CARTESIAN_POINT('Origin',(35.7,0.,0.));
#30105=CARTESIAN_POINT('',(30.5,-34.9656486014478,1.55029606206997));
#30106=CARTESIAN_POINT('Ctrl Pts',(40.3999921398529,-34.9678423429768,1.49999538724756));
#30107=CARTESIAN_POINT('Ctrl Pts',(39.2499570215113,-34.9678422244593,1.49997501500716));
#30108=CARTESIAN_POINT('Ctrl Pts',(38.0998114916604,-34.9678417480135,1.49989311899335));
#30109=CARTESIAN_POINT('Ctrl Pts',(36.9497038557168,-34.9678416168427,1.49987059349837));
#30110=CARTESIAN_POINT('Ctrl Pts',(36.785105117964,-34.96784159807,1.49986736974094));
#30111=CARTESIAN_POINT('Ctrl Pts',(36.6205071563607,-34.9678415863694,1.49986536202073));
#30112=CARTESIAN_POINT('Ctrl Pts',(36.4559233022361,-34.9678415707796,1.49986268095532));
#30113=CARTESIAN_POINT('Ctrl Pts',(36.4193640724435,-34.9678415673166,1.4998620854067));
#30114=CARTESIAN_POINT('Ctrl Pts',(36.3828055387466,-34.9678415636617,1.49986145663366));
#30115=CARTESIAN_POINT('Ctrl Pts',(36.3462474593958,-34.967841559861,1.49986080263033));
#30116=CARTESIAN_POINT('Ctrl Pts',(36.0895450699579,-34.967841533173,1.49985621036996));
#30117=CARTESIAN_POINT('Ctrl Pts',(35.8501671305851,-34.9678416196704,1.49985084735669));
#30118=CARTESIAN_POINT('Ctrl Pts',(35.6266230092018,-34.9678417642539,1.49984692867087));
#30119=CARTESIAN_POINT('Ctrl Pts',(35.5729810992077,-34.9678417989483,1.49984598833841));
#30120=CARTESIAN_POINT('Ctrl Pts',(35.5202511626857,-34.9678418369404,1.49984512300934));
#30121=CARTESIAN_POINT('Ctrl Pts',(35.4684130151836,-34.9678418773881,1.49984434928581));
#30122=CARTESIAN_POINT('Ctrl Pts',(35.3128073279263,-34.9678419988026,1.49984202675329));
#30123=CARTESIAN_POINT('Ctrl Pts',(35.1652418679138,-34.9678421408902,1.49984027810625));
#30124=CARTESIAN_POINT('Ctrl Pts',(35.0252627275547,-34.967842254217,1.49983493809963));
#30125=CARTESIAN_POINT('Ctrl Pts',(35.0082618963838,-34.9678422679808,1.49983428954192));
#30126=CARTESIAN_POINT('Ctrl Pts',(34.9913729068342,-34.9678422813397,1.49983359135557));
#30127=CARTESIAN_POINT('Ctrl Pts',(34.9745948969331,-34.9678422942204,1.49983283870325));
#30128=CARTESIAN_POINT('Ctrl Pts',(34.8399133402553,-34.9678423976168,1.49982679696251));
#30129=CARTESIAN_POINT('Ctrl Pts',(34.7123780512931,-34.9678424712592,1.49981743040038));
#30130=CARTESIAN_POINT('Ctrl Pts',(34.591404591981,-34.9678425127826,1.49980840280397));
#30131=CARTESIAN_POINT('Ctrl Pts',(34.4539348326465,-34.9678425599684,1.49979814417772));
#30132=CARTESIAN_POINT('Ctrl Pts',(34.3249390274092,-34.9678425655798,1.49978830616205));
#30133=CARTESIAN_POINT('Ctrl Pts',(34.2036312646158,-34.9678425105859,1.49978156609768));
#30134=CARTESIAN_POINT('Ctrl Pts',(34.1284740534062,-34.967842476514,1.49977739023598));
#30135=CARTESIAN_POINT('Ctrl Pts',(34.0562692606603,-34.9678424188851,1.49977435262848));
#30136=CARTESIAN_POINT('Ctrl Pts',(33.9868395791739,-34.9678423310509,1.49977272195139));
#30137=CARTESIAN_POINT('Ctrl Pts',(33.944569913827,-34.9678422775764,1.49977172917462));
#30138=CARTESIAN_POINT('Ctrl Pts',(33.903332682828,-34.9678422127028,1.49977122168105));
#30139=CARTESIAN_POINT('Ctrl Pts',(33.8632274501546,-34.9678421281365,1.49977004757329));
#30140=CARTESIAN_POINT('Ctrl Pts',(33.8167531035319,-34.9678420301403,1.49976868700542));
#30141=CARTESIAN_POINT('Ctrl Pts',(33.771789463122,-34.9678419060139,1.49976648823776));
#30142=CARTESIAN_POINT('Ctrl Pts',(33.7281109635882,-34.9678417565821,1.49976414064438));
#30143=CARTESIAN_POINT('Ctrl Pts',(33.6812712011832,-34.9678415963351,1.49976162314223));
#30144=CARTESIAN_POINT('Ctrl Pts',(33.6359095723891,-34.9678414069824,1.49975893360226));
#30145=CARTESIAN_POINT('Ctrl Pts',(33.591810246565,-34.9678411881909,1.49975667024847));
#30146=CARTESIAN_POINT('Ctrl Pts',(33.5583448079856,-34.9678410221577,1.4997549526683));
#30147=CARTESIAN_POINT('Ctrl Pts',(33.5256076932742,-34.9678408391413,1.49975347489115));
#30148=CARTESIAN_POINT('Ctrl Pts',(33.4935243452377,-34.9678406385663,1.49975241817239));
#30149=CARTESIAN_POINT('Ctrl Pts',(33.4574180647961,-34.9678404128412,1.49975122895162));
#30150=CARTESIAN_POINT('Ctrl Pts',(33.4221459355308,-34.9678401647559,1.49975055002974));
#30151=CARTESIAN_POINT('Ctrl Pts',(33.3878318916215,-34.9678398888653,1.49974977143672));
#30152=CARTESIAN_POINT('Ctrl Pts',(33.3506903036195,-34.9678395902407,1.49974892868613));
#30153=CARTESIAN_POINT('Ctrl Pts',(33.3146710708563,-34.9678392590421,1.49974796966079));
#30154=CARTESIAN_POINT('Ctrl Pts',(33.2798677329257,-34.967838889585,1.49974635090117));
#30155=CARTESIAN_POINT('Ctrl Pts',(33.2432742079925,-34.9678385011241,1.49974464887706));
#30156=CARTESIAN_POINT('Ctrl Pts',(33.2080243245405,-34.9678380703783,1.49974221953695));
#30157=CARTESIAN_POINT('Ctrl Pts',(33.1741651388243,-34.9678375919209,1.49973865377071));
#30158=CARTESIAN_POINT('Ctrl Pts',(33.1370631468227,-34.96783706764,1.49973474649923));
#30159=CARTESIAN_POINT('Ctrl Pts',(33.101630651562,-34.9678364860775,1.49972947597289));
#30160=CARTESIAN_POINT('Ctrl Pts',(33.0678641021075,-34.9678358413429,1.49972253958675));
#30161=CARTESIAN_POINT('Ctrl Pts',(33.0456526984029,-34.967835417241,1.49971797687971));
#30162=CARTESIAN_POINT('Ctrl Pts',(33.0241607955795,-34.9678349658306,1.49971269819094));
#30163=CARTESIAN_POINT('Ctrl Pts',(33.0033754048768,-34.9678344856631,1.49970666036489));
#30164=CARTESIAN_POINT('Ctrl Pts',(32.9442530209621,-34.9678331198648,1.49968948625087));
#30165=CARTESIAN_POINT('Ctrl Pts',(32.8887085075052,-34.9678225692835,1.49991335207053));
#30166=CARTESIAN_POINT('Ctrl Pts',(32.8362583193005,-34.9678066670084,1.50027559162313));
#30167=CARTESIAN_POINT('Ctrl Pts',(32.7773090712612,-34.9677887942955,1.50068271598182));
#30168=CARTESIAN_POINT('Ctrl Pts',(32.7222687069611,-34.9677641462319,1.50126502290935));
#30169=CARTESIAN_POINT('Ctrl Pts',(32.6704155259707,-34.9677359487883,1.50193537623736));
#30170=CARTESIAN_POINT('Ctrl Pts',(32.6144302418903,-34.9677055043322,1.50265914902789));
#30171=CARTESIAN_POINT('Ctrl Pts',(32.5621602746537,-34.967670888482,1.50348644308882));
#30172=CARTESIAN_POINT('Ctrl Pts',(32.5126575741462,-34.9676341575402,1.50436077830379));
#30173=CARTESIAN_POINT('Ctrl Pts',(32.4592478825334,-34.967594527616,1.50530412025724));
#30174=CARTESIAN_POINT('Ctrl Pts',(32.4090594121703,-34.9675524017484,1.50630310623456));
#30175=CARTESIAN_POINT('Ctrl Pts',(32.3608584151776,-34.9675086790575,1.50733170420881));
#30176=CARTESIAN_POINT('Ctrl Pts',(32.3080624384018,-34.9674607883018,1.50845835797426));
#30177=CARTESIAN_POINT('Ctrl Pts',(32.2576510584102,-34.9674109512874,1.50962133088217));
#30178=CARTESIAN_POINT('Ctrl Pts',(32.2079531230122,-34.9673589385144,1.51082436306573));
#30179=CARTESIAN_POINT('Ctrl Pts',(32.1569814991443,-34.9673055927269,1.51205822727901));
#30180=CARTESIAN_POINT('Ctrl Pts',(32.1067603493753,-34.9672499217566,1.51333518230823));
#30181=CARTESIAN_POINT('Ctrl Pts',(32.0554367657627,-34.9671908102209,1.51468303813506));
#30182=CARTESIAN_POINT('Ctrl Pts',(32.0053752916503,-34.9671331523098,1.51599774854366));
#30183=CARTESIAN_POINT('Ctrl Pts',(31.9542650752303,-34.9670721879269,1.51738077462805));
#30184=CARTESIAN_POINT('Ctrl Pts',(31.9003392718779,-34.9670065776396,1.51886693662989));
#30185=CARTESIAN_POINT('Ctrl Pts',(31.8778362033484,-34.9669791986726,1.51948710736995));
#30186=CARTESIAN_POINT('Ctrl Pts',(31.8548422465646,-34.9669510097079,1.52012527669196));
#30187=CARTESIAN_POINT('Ctrl Pts',(31.8312262657831,-34.9669219190816,1.52078388908931));
#30188=CARTESIAN_POINT('Ctrl Pts',(31.7273802318769,-34.9667939995094,1.52367999092728));
#30189=CARTESIAN_POINT('Ctrl Pts',(31.6210019634565,-34.9666588880294,1.52670831990391));
#30190=CARTESIAN_POINT('Ctrl Pts',(31.5129311113833,-34.9665259706005,1.52968152042074));
#30191=CARTESIAN_POINT('Ctrl Pts',(31.4048670765169,-34.9663930615562,1.5326545333854));
#30192=CARTESIAN_POINT('Ctrl Pts',(31.295110396831,-34.9662624173991,1.53557057541601));
#30193=CARTESIAN_POINT('Ctrl Pts',(31.1845493642895,-34.9661438310284,1.53823056067685));
#30194=CARTESIAN_POINT('Ctrl Pts',(31.1321570104796,-34.9660876356498,1.5394910670751));
#30195=CARTESIAN_POINT('Ctrl Pts',(31.0795847658982,-34.9660341471942,1.54069407696174));
#30196=CARTESIAN_POINT('Ctrl Pts',(31.0269312050905,-34.9659843676727,1.54181935957433));
#30197=CARTESIAN_POINT('Ctrl Pts',(30.9325025960689,-34.9658950933502,1.5438374352796));
#30198=CARTESIAN_POINT('Ctrl Pts',(30.8378102330027,-34.9658178028119,1.54560383003055));
#30199=CARTESIAN_POINT('Ctrl Pts',(30.7433599242841,-34.9657577677723,1.54697518213503));
#30200=CARTESIAN_POINT('Ctrl Pts',(30.6608249248197,-34.965705306409,1.54817353232302));
#30201=CARTESIAN_POINT('Ctrl Pts',(30.5784749808876,-34.9656660234083,1.54907006656161));
#30202=CARTESIAN_POINT('Ctrl Pts',(30.4966730088978,-34.9656427667437,1.54959005157024));
#30203=CARTESIAN_POINT('',(30.5,-34.9699609326822,-1.44976976333441));
#30204=CARTESIAN_POINT('Origin',(30.5,0.,0.));
#30205=CARTESIAN_POINT('Ctrl Pts',(30.5051992612603,-34.9699071381489,-1.44903843638966));
#30206=CARTESIAN_POINT('Ctrl Pts',(30.6030952980657,-34.9698787568566,-1.44976082626917));
#30207=CARTESIAN_POINT('Ctrl Pts',(30.7001121880333,-34.9698264221104,-1.45104998650339));
#30208=CARTESIAN_POINT('Ctrl Pts',(30.7969947619801,-34.9697577270266,-1.45274237549662));
#30209=CARTESIAN_POINT('Ctrl Pts',(30.8545454823775,-34.9697169203944,-1.45374769773142));
#30210=CARTESIAN_POINT('Ctrl Pts',(30.9120492097055,-34.9696702850816,-1.45489634227782));
#30211=CARTESIAN_POINT('Ctrl Pts',(30.9696671110348,-34.9696190483589,-1.45616096255286));
#30212=CARTESIAN_POINT('Ctrl Pts',(31.0687356284601,-34.969530951673,-1.45833535719175));
#30213=CARTESIAN_POINT('Ctrl Pts',(31.1681385828748,-34.9694292858245,-1.46085179879274));
#30214=CARTESIAN_POINT('Ctrl Pts',(31.2685908593294,-34.9693191238307,-1.46356721252908));
#30215=CARTESIAN_POINT('Ctrl Pts',(31.3711796386319,-34.9692066188196,-1.46634037995092));
#30216=CARTESIAN_POINT('Ctrl Pts',(31.4748629185107,-34.9690851710714,-1.46932276608705));
#30217=CARTESIAN_POINT('Ctrl Pts',(31.5804543970555,-34.9689598486836,-1.4723695155306));
#30218=CARTESIAN_POINT('Ctrl Pts',(31.6427002532175,-34.9688859715162,-1.47416556508156));
#30219=CARTESIAN_POINT('Ctrl Pts',(31.7056101943812,-34.9688107472906,-1.47598400420448));
#30220=CARTESIAN_POINT('Ctrl Pts',(31.7693590594471,-34.9687353433411,-1.4777925610394));
#30221=CARTESIAN_POINT('Ctrl Pts',(31.8369567664635,-34.968655386873,-1.47971030961302));
#30222=CARTESIAN_POINT('Ctrl Pts',(31.8998289473023,-34.9685826953725,-1.48145356148269));
#30223=CARTESIAN_POINT('Ctrl Pts',(31.9584912820088,-34.9685172658125,-1.48302365833457));
#30224=CARTESIAN_POINT('Ctrl Pts',(32.0219681801233,-34.9684464662861,-1.48472261693203));
#30225=CARTESIAN_POINT('Ctrl Pts',(32.0805160965752,-34.9683841232145,-1.48621979971344));
#30226=CARTESIAN_POINT('Ctrl Pts',(32.1348442130228,-34.9683291276834,-1.48754049944253));
#30227=CARTESIAN_POINT('Ctrl Pts',(32.1955320114825,-34.9682676943422,-1.48901580107684));
#30228=CARTESIAN_POINT('Ctrl Pts',(32.2509543450045,-34.9682153821449,-1.49027186778449));
#30229=CARTESIAN_POINT('Ctrl Pts',(32.3021641802449,-34.968170114115,-1.49135570584805));
#30230=CARTESIAN_POINT('Ctrl Pts',(32.3568725417881,-34.9681217534879,-1.49251358898431));
#30231=CARTESIAN_POINT('Ctrl Pts',(32.4067738547341,-34.9680813901956,-1.49347579219532));
#30232=CARTESIAN_POINT('Ctrl Pts',(32.4532143425777,-34.9680466762592,-1.49429647043747));
#30233=CARTESIAN_POINT('Ctrl Pts',(32.5024778890134,-34.9680098521064,-1.49516703667327));
#30234=CARTESIAN_POINT('Ctrl Pts',(32.5478477692462,-34.9679793561973,-1.49587895592541));
#30235=CARTESIAN_POINT('Ctrl Pts',(32.5909873019042,-34.9679531603256,-1.49648137333639));
#30236=CARTESIAN_POINT('Ctrl Pts',(32.6362425762347,-34.9679256796997,-1.49711333579671));
#30237=CARTESIAN_POINT('Ctrl Pts',(32.6790438910183,-34.9679029082457,-1.49762527612471));
#30238=CARTESIAN_POINT('Ctrl Pts',(32.7213614276303,-34.9678837287556,-1.49804900699204));
#30239=CARTESIAN_POINT('Ctrl Pts',(32.7633326545687,-34.9678647062226,-1.49846927021664));
#30240=CARTESIAN_POINT('Ctrl Pts',(32.8048283340763,-34.9678491963778,-1.49880319667881));
#30241=CARTESIAN_POINT('Ctrl Pts',(32.8478112859697,-34.9678375791942,-1.49905168880698));
#30242=CARTESIAN_POINT('Ctrl Pts',(32.8880595868515,-34.9678267011162,-1.49928437142882));
#30243=CARTESIAN_POINT('Ctrl Pts',(32.9296120625675,-34.9678192143482,-1.49944259954574));
#30244=CARTESIAN_POINT('Ctrl Pts',(32.9741124736885,-34.9678170031322,-1.49949475964765));
#30245=CARTESIAN_POINT('Ctrl Pts',(32.9824658917633,-34.9678165880527,-1.49950455090861));
#30246=CARTESIAN_POINT('Ctrl Pts',(32.9909232824636,-34.9678163642396,-1.49951049395371));
#30247=CARTESIAN_POINT('Ctrl Pts',(32.9994956564547,-34.9678163521983,-1.4995122138931));
#30248=CARTESIAN_POINT('Ctrl Pts',(33.035916707601,-34.9678163010392,-1.49951952132052));
#30249=CARTESIAN_POINT('Ctrl Pts',(33.0737648470631,-34.9678163144541,-1.49952600456097));
#30250=CARTESIAN_POINT('Ctrl Pts',(33.1138039348094,-34.9678165569182,-1.49953164904712));
#30251=CARTESIAN_POINT('Ctrl Pts',(33.2457861392315,-34.9678173561608,-1.49955025515845));
#30252=CARTESIAN_POINT('Ctrl Pts',(33.3718058092168,-34.9678177616075,-1.49955552940343));
#30253=CARTESIAN_POINT('Ctrl Pts',(33.4990121011459,-34.9678181023247,-1.49956083536768));
#30254=CARTESIAN_POINT('Ctrl Pts',(33.6624238693915,-34.9678185400169,-1.49956765151637));
#30255=CARTESIAN_POINT('Ctrl Pts',(33.8277938592881,-34.9678188708891,-1.49957452000976));
#30256=CARTESIAN_POINT('Ctrl Pts',(33.9926457806311,-34.9678194856962,-1.49958605843696));
#30257=CARTESIAN_POINT('Ctrl Pts',(34.322349623317,-34.9678207153104,-1.49960913529135));
#30258=CARTESIAN_POINT('Ctrl Pts',(34.649981191788,-34.9678230806641,-1.49965089188094));
#30259=CARTESIAN_POINT('Ctrl Pts',(34.978743760729,-34.9678240597269,-1.499668413021));
#30260=CARTESIAN_POINT('Ctrl Pts',(35.1431250451995,-34.9678245492582,-1.49967717359104));
#30261=CARTESIAN_POINT('Ctrl Pts',(35.3077890797876,-34.9678246922169,-1.49967987529869));
#30262=CARTESIAN_POINT('Ctrl Pts',(35.4723919953983,-34.9678249110675,-1.49968390458378));
#30263=CARTESIAN_POINT('Ctrl Pts',(35.9662007422305,-34.9678255676192,-1.49969599243905));
#30264=CARTESIAN_POINT('Ctrl Pts',(36.4594594182669,-34.9678269071982,-1.49972002849122));
#30265=CARTESIAN_POINT('Ctrl Pts',(36.9527108273738,-34.9678287658476,-1.49975356610212));
#30266=CARTESIAN_POINT('Ctrl Pts',(38.1015495523822,-34.9678330948538,-1.49983167901864));
#30267=CARTESIAN_POINT('Ctrl Pts',(39.2503488559568,-34.9678402396984,-1.49996133572171));
#30268=CARTESIAN_POINT('Ctrl Pts',(40.4000634893725,-34.9678419791559,-1.49999290859452));
#30269=CARTESIAN_POINT('Ctrl Pts',(6.89999999997365,-9.46599415780712,-5.65979197164529));
#30270=CARTESIAN_POINT('Ctrl Pts',(6.99168932310453,-9.49787619923353,-5.60729410195164));
#30271=CARTESIAN_POINT('Ctrl Pts',(7.08405956072215,-9.52934434473076,-5.55450818731572));
#30272=CARTESIAN_POINT('Ctrl Pts',(8.15473535981986,-9.88659437915722,-4.94320927931172));
#30273=CARTESIAN_POINT('Ctrl Pts',(9.17052309187647,-10.1553288976265,-4.34956920012189));
#30274=CARTESIAN_POINT('Ctrl Pts',(11.249912418623,-10.5681406908193,-3.24757657546859));
#30275=CARTESIAN_POINT('Ctrl Pts',(12.2613271155137,-10.7096926815135,-2.71507294053766));
#30276=CARTESIAN_POINT('Ctrl Pts',(14.3530613265277,-10.9182780492489,-1.75089621035865));
#30277=CARTESIAN_POINT('Ctrl Pts',(15.3683896576347,-10.9736589531833,-1.30024364084097));
#30278=CARTESIAN_POINT('Ctrl Pts',(17.4699484560063,-11.0479347559914,-0.511606508085749));
#30279=CARTESIAN_POINT('Ctrl Pts',(18.4899441076999,-11.0518486975415,-0.154966618543406));
#30280=CARTESIAN_POINT('Ctrl Pts',(19.8459385111079,-11.0525063200436,0.227738630131173));
#30281=CARTESIAN_POINT('Ctrl Pts',(20.3436052070642,-11.0499443867429,0.36401229334755));
#30282=CARTESIAN_POINT('Ctrl Pts',(21.3765735172499,-11.0391187302377,0.626365466004487));
#30283=CARTESIAN_POINT('Ctrl Pts',(22.1786513408684,-11.0271780970655,0.801482370854041));
#30284=CARTESIAN_POINT('Ctrl Pts',(22.8524711894103,-11.0190184236597,0.927590054426943));
#30285=CARTESIAN_POINT('Ctrl Pts',(23.1034772575406,-11.015636270466,0.973361071581969));
#30286=CARTESIAN_POINT('Ctrl Pts',(23.6153488598143,-11.0082046691873,1.06157978958535));
#30287=CARTESIAN_POINT('Ctrl Pts',(24.2640912191231,-10.9980907558832,1.16309571993124));
#30288=CARTESIAN_POINT('Ctrl Pts',(24.9252112071703,-10.9882975006411,1.25112898708133));
#30289=CARTESIAN_POINT('Ctrl Pts',(25.3924209938587,-10.9823391891697,1.30426168416562));
#30290=CARTESIAN_POINT('Ctrl Pts',(25.6607104515486,-10.9792975977554,1.332046615497));
#30291=CARTESIAN_POINT('Ctrl Pts',(25.7950739758558,-10.9779150347045,1.34502686686554));
#30292=CARTESIAN_POINT('Ctrl Pts',(26.2512918422651,-10.9735046934062,1.38748529291552));
#30293=CARTESIAN_POINT('Ctrl Pts',(27.3073301682004,-10.9653764904263,1.45732017866833));
#30294=CARTESIAN_POINT('Ctrl Pts',(28.3319194320811,-10.9609947024269,1.48237708919284));
#30295=CARTESIAN_POINT('Ctrl Pts',(29.1280123944214,-10.9582092660149,1.50394716937725));
#30296=CARTESIAN_POINT('Ctrl Pts',(29.4779818455993,-10.9573324846489,1.51103964894258));
#30297=CARTESIAN_POINT('Ctrl Pts',(29.9466600480359,-10.9567800220405,1.51533483257754));
#30298=CARTESIAN_POINT('Ctrl Pts',(30.4585980273686,-10.956656708735,1.51632751174059));
#30299=CARTESIAN_POINT('Ctrl Pts',(31.4732549878281,-10.9572594965941,1.51158385370564));
#30300=CARTESIAN_POINT('Ctrl Pts',(32.3455845021632,-10.95879335959,1.4999511927851));
#30301=CARTESIAN_POINT('Ctrl Pts',(33.1628510802405,-10.9587933798862,1.49997453311311));
#30302=CARTESIAN_POINT('Ctrl Pts',(33.4532441810442,-10.9587933789851,1.49997366471359));
#30303=CARTESIAN_POINT('Ctrl Pts',(33.7813843869345,-10.9587933812939,1.49997637381128));
#30304=CARTESIAN_POINT('Ctrl Pts',(34.2755379701535,-10.9587933817727,1.49997699476315));
#30305=CARTESIAN_POINT('Ctrl Pts',(34.8102302793009,-10.9587933869434,1.49998326277599));
#30306=CARTESIAN_POINT('Ctrl Pts',(35.6332452367756,-10.9587933876415,1.49998412101817));
#30307=CARTESIAN_POINT('Ctrl Pts',(36.2915450349079,-10.9587933890033,1.49998577371297));
#30308=CARTESIAN_POINT('Ctrl Pts',(38.1020137670942,-10.9587933908629,1.49998803993575));
#30309=CARTESIAN_POINT('Ctrl Pts',(39.5833333333333,-10.9587934006931,1.5));
#30310=CARTESIAN_POINT('Ctrl Pts',(40.9,-10.9587934006931,1.5));
#30311=CARTESIAN_POINT('Ctrl Pts',(6.65963435785827,-13.0027682689653,-8.56288377493212));
#30312=CARTESIAN_POINT('Ctrl Pts',(6.7513219377677,-13.050957789036,-8.49067817166156));
#30313=CARTESIAN_POINT('Ctrl Pts',(6.84370278928156,-13.0985893115687,-8.41801298642698));
#30314=CARTESIAN_POINT('Ctrl Pts',(7.91483960325935,-13.6397807532085,-7.57680655910808));
#30315=CARTESIAN_POINT('Ctrl Pts',(8.9325509112231,-14.0543934435321,-6.75518385076231));
#30316=CARTESIAN_POINT('Ctrl Pts',(11.0192135814157,-14.7040310435559,-5.22065437877307));
#30317=CARTESIAN_POINT('Ctrl Pts',(12.0340542508324,-14.9356992206141,-4.4769598695545));
#30318=CARTESIAN_POINT('Ctrl Pts',(14.1407660172285,-15.2883456800052,-3.1214593369057));
#30319=CARTESIAN_POINT('Ctrl Pts',(15.1616568764318,-15.3931503655329,-2.48732138966201));
#30320=CARTESIAN_POINT('Ctrl Pts',(17.287218760307,-15.5446125872455,-1.36959877283814));
#30321=CARTESIAN_POINT('Ctrl Pts',(18.3145546794907,-15.5707395254148,-0.864902786641509));
#30322=CARTESIAN_POINT('Ctrl Pts',(19.6926214867647,-15.5935126543779,-0.318801403605145));
#30323=CARTESIAN_POINT('Ctrl Pts',(20.19452636269,-15.5977145841048,-0.125373946234776));
#30324=CARTESIAN_POINT('Ctrl Pts',(21.2420076978203,-15.5972978704292,0.248868189963684));
#30325=CARTESIAN_POINT('Ctrl Pts',(22.0575126096201,-15.5901933457539,0.499284562147393));
#30326=CARTESIAN_POINT('Ctrl Pts',(22.7441078663834,-15.5856475377419,0.679992377552246));
#30327=CARTESIAN_POINT('Ctrl Pts',(22.9980856324395,-15.5834353094767,0.745267685418835));
#30328=CARTESIAN_POINT('Ctrl Pts',(23.5177883906687,-15.5778337615218,0.871419538176182));
#30329=CARTESIAN_POINT('Ctrl Pts',(24.1766640555165,-15.569151455817,1.01665680544525));
#30330=CARTESIAN_POINT('Ctrl Pts',(24.8496697365589,-15.560128822227,1.14287321247013));
#30331=CARTESIAN_POINT('Ctrl Pts',(25.3259254544069,-15.554601684436,1.21914041353961));
#30332=CARTESIAN_POINT('Ctrl Pts',(25.5996882691236,-15.5518109321211,1.2590574298324));
#30333=CARTESIAN_POINT('Ctrl Pts',(25.7368188560809,-15.550561003587,1.27770917936971));
#30334=CARTESIAN_POINT('Ctrl Pts',(26.2030586507879,-15.5466206431081,1.33878235986071));
#30335=CARTESIAN_POINT('Ctrl Pts',(27.2845562696213,-15.5388831179539,1.43928616936987));
#30336=CARTESIAN_POINT('Ctrl Pts',(28.3146233763975,-15.534108117874,1.47473229777558));
#30337=CARTESIAN_POINT('Ctrl Pts',(29.1121433593266,-15.5313810124223,1.5053783917148));
#30338=CARTESIAN_POINT('Ctrl Pts',(29.4693616319656,-15.5305221749293,1.51558516408219));
#30339=CARTESIAN_POINT('Ctrl Pts',(29.9425518103672,-15.5299808253862,1.5216968643791));
#30340=CARTESIAN_POINT('Ctrl Pts',(30.4595136734855,-15.5298599056894,1.52312339822458));
#30341=CARTESIAN_POINT('Ctrl Pts',(31.4800666545032,-15.5304501241615,1.51634797661239));
#30342=CARTESIAN_POINT('Ctrl Pts',(32.3507119180564,-15.5319509809364,1.4999128955352));
#30343=CARTESIAN_POINT('Ctrl Pts',(33.1621363777215,-15.5319505779396,1.49995461572564));
#30344=CARTESIAN_POINT('Ctrl Pts',(33.4535196029878,-15.5319505880019,1.49995304854269));
#30345=CARTESIAN_POINT('Ctrl Pts',(33.7812306484551,-15.5319505396377,1.49995788616631));
#30346=CARTESIAN_POINT('Ctrl Pts',(34.2755524327802,-15.531950526851,1.49995898984267));
#30347=CARTESIAN_POINT('Ctrl Pts',(34.8101578274898,-15.5319504091692,1.4999701650853));
#30348=CARTESIAN_POINT('Ctrl Pts',(35.6332135248365,-15.5319503927198,1.49997169422773));
#30349=CARTESIAN_POINT('Ctrl Pts',(36.2914988048216,-15.5319503616369,1.49997464065556));
#30350=CARTESIAN_POINT('Ctrl Pts',(38.1019885414694,-15.5319503187541,1.49997868009126));
#30351=CARTESIAN_POINT('Ctrl Pts',(39.5833333333333,-15.5319500929849,1.5));
#30352=CARTESIAN_POINT('Ctrl Pts',(40.9,-15.5319500929849,1.5));
#30353=CARTESIAN_POINT('Ctrl Pts',(6.47503677058814,-19.2049631177014,-13.6264850125633));
#30354=CARTESIAN_POINT('Ctrl Pts',(6.56582707216344,-19.2807931407427,-13.5206117629928));
#30355=CARTESIAN_POINT('Ctrl Pts',(6.65722187862393,-19.3557456396964,-13.4141026801341));
#30356=CARTESIAN_POINT('Ctrl Pts',(7.71979853459931,-20.2113974185276,-12.1774082172639));
#30357=CARTESIAN_POINT('Ctrl Pts',(8.72714740265586,-20.876585861408,-10.9649265084515));
#30358=CARTESIAN_POINT('Ctrl Pts',(10.792252425961,-21.9312131301472,-8.69413764846817));
#30359=CARTESIAN_POINT('Ctrl Pts',(11.8008983729842,-22.3203974544121,-7.58577239973431));
#30360=CARTESIAN_POINT('Ctrl Pts',(13.892634394048,-22.9231109701401,-5.56042793834188));
#30361=CARTESIAN_POINT('Ctrl Pts',(14.910936596525,-23.1162450123325,-4.60683703173286));
#30362=CARTESIAN_POINT('Ctrl Pts',(17.0374816014601,-23.4053158267904,-2.91606182242837));
#30363=CARTESIAN_POINT('Ctrl Pts',(18.0678529336714,-23.4724397837998,-2.15006970557795));
#30364=CARTESIAN_POINT('Ctrl Pts',(19.4632774216583,-23.5361137002685,-1.31129970902877));
#30365=CARTESIAN_POINT('Ctrl Pts',(19.9690853949367,-23.5527456051548,-1.01646669656859));
#30366=CARTESIAN_POINT('Ctrl Pts',(21.0306109698709,-23.5717577824589,-0.441678056412671));
#30367=CARTESIAN_POINT('Ctrl Pts',(21.8626014988188,-23.5739085372705,-0.0543003442681394));
#30368=CARTESIAN_POINT('Ctrl Pts',(22.5665651705188,-23.576178914363,0.226484889079846));
#30369=CARTESIAN_POINT('Ctrl Pts',(22.8246411038756,-23.5761448043361,0.326902916553467));
#30370=CARTESIAN_POINT('Ctrl Pts',(23.3554232774669,-23.5740054132278,0.522054743089696));
#30371=CARTESIAN_POINT('Ctrl Pts',(24.0293769285439,-23.5680817805141,0.74700585878865));
#30372=CARTESIAN_POINT('Ctrl Pts',(24.7209631427047,-23.560586503548,0.943393581394333));
#30373=CARTESIAN_POINT('Ctrl Pts',(25.2118242719342,-23.5558940963915,1.06233480615607));
#30374=CARTESIAN_POINT('Ctrl Pts',(25.4945546545947,-23.5535795021665,1.12470144437592));
#30375=CARTESIAN_POINT('Ctrl Pts',(25.6362544160062,-23.5525764277763,1.15385183559377));
#30376=CARTESIAN_POINT('Ctrl Pts',(26.1191683853685,-23.5495095529483,1.24953281052836));
#30377=CARTESIAN_POINT('Ctrl Pts',(27.244410780189,-23.5425023713064,1.40715534997208));
#30378=CARTESIAN_POINT('Ctrl Pts',(28.2843056152442,-23.5370396227258,1.46065929315376));
#30379=CARTESIAN_POINT('Ctrl Pts',(29.0843244121809,-23.5344215873996,1.50737208683505));
#30380=CARTESIAN_POINT('Ctrl Pts',(29.4542021761287,-23.5335942286398,1.52336782189617));
#30381=CARTESIAN_POINT('Ctrl Pts',(29.9352997409898,-23.5330734925559,1.53271512054377));
#30382=CARTESIAN_POINT('Ctrl Pts',(30.4610555884278,-23.532957187389,1.5349453613852));
#30383=CARTESIAN_POINT('Ctrl Pts',(31.4919316519535,-23.5335262680548,1.52450364515754));
#30384=CARTESIAN_POINT('Ctrl Pts',(32.3596576160514,-23.5349731541844,1.49979324124414));
#30385=CARTESIAN_POINT('Ctrl Pts',(33.1608710165812,-23.5349736853906,1.49989213988255));
#30386=CARTESIAN_POINT('Ctrl Pts',(33.4539865796869,-23.5349736699323,1.49988845489238));
#30387=CARTESIAN_POINT('Ctrl Pts',(33.780948091659,-23.5349737329761,1.49989993226727));
#30388=CARTESIAN_POINT('Ctrl Pts',(34.275564602361,-23.5349737489117,1.49990256114204));
#30389=CARTESIAN_POINT('Ctrl Pts',(34.810021467207,-23.5349738998239,1.49992910993535));
#30390=CARTESIAN_POINT('Ctrl Pts',(35.6331489543767,-23.5349739207807,1.49993274473986));
#30391=CARTESIAN_POINT('Ctrl Pts',(36.2914097700016,-23.5349739606187,1.4999397448351));
#30392=CARTESIAN_POINT('Ctrl Pts',(38.1019375614968,-23.5349740154737,1.49994934328327));
#30393=CARTESIAN_POINT('Ctrl Pts',(39.5833333333333,-23.5349743044955,1.5));
#30394=CARTESIAN_POINT('Ctrl Pts',(40.9,-23.5349743044955,1.5));
#30395=CARTESIAN_POINT('Ctrl Pts',(6.39840282685635,-25.4797798158266,-18.5950148818));
#30396=CARTESIAN_POINT('Ctrl Pts',(6.48879582230594,-25.5825069307027,-18.455456538043));
#30397=CARTESIAN_POINT('Ctrl Pts',(6.57973810483189,-25.684006582131,-18.3151558806717));
#30398=CARTESIAN_POINT('Ctrl Pts',(7.63881202209715,-26.8457843562122,-16.6821095714367));
#30399=CARTESIAN_POINT('Ctrl Pts',(8.64206536867565,-27.7524045864227,-15.0805562774161));
#30400=CARTESIAN_POINT('Ctrl Pts',(10.6943835463645,-29.194220471563,-12.08639394536));
#30401=CARTESIAN_POINT('Ctrl Pts',(11.6986850371144,-29.7340826089764,-10.6188960618635));
#30402=CARTESIAN_POINT('Ctrl Pts',(13.7736723466472,-30.5724457120527,-7.9480571508383));
#30403=CARTESIAN_POINT('Ctrl Pts',(14.7865355152845,-30.8496813329458,-6.68379951334874));
#30404=CARTESIAN_POINT('Ctrl Pts',(16.895644387614,-31.2681094727719,-4.44867953439714));
#30405=CARTESIAN_POINT('Ctrl Pts',(17.921113585793,-31.3748718553479,-3.42955614780409));
#30406=CARTESIAN_POINT('Ctrl Pts',(19.3111115725317,-31.4778602005301,-2.31180057560694));
#30407=CARTESIAN_POINT('Ctrl Pts',(19.8164097330209,-31.5068304778962,-1.91755167896535));
#30408=CARTESIAN_POINT('Ctrl Pts',(20.8772665291465,-31.5450009606978,-1.1480473205349));
#30409=CARTESIAN_POINT('Ctrl Pts',(21.7126526899651,-31.5565752055434,-0.625757760628935));
#30410=CARTESIAN_POINT('Ctrl Pts',(22.4233939916368,-31.5658469864011,-0.244774266221902));
#30411=CARTESIAN_POINT('Ctrl Pts',(22.68321700305,-31.568070163829,-0.109074102068982));
#30412=CARTESIAN_POINT('Ctrl Pts',(23.2191843843282,-31.5695528321153,0.155714853804437));
#30413=CARTESIAN_POINT('Ctrl Pts',(23.9014490792895,-31.5665856540486,0.461901703286711));
#30414=CARTESIAN_POINT('Ctrl Pts',(24.6052033552109,-31.5607844376464,0.730987709817269));
#30415=CARTESIAN_POINT('Ctrl Pts',(25.1069219885717,-31.5570192016244,0.894795181267933));
#30416=CARTESIAN_POINT('Ctrl Pts',(25.3966703145091,-31.5552253028176,0.98095784259731));
#30417=CARTESIAN_POINT('Ctrl Pts',(25.5420691491796,-31.5544886793522,1.02128571697646));
#30418=CARTESIAN_POINT('Ctrl Pts',(26.0386675456483,-31.5523567719375,1.15405115562807));
#30419=CARTESIAN_POINT('Ctrl Pts',(27.2041996425261,-31.5461367082151,1.37405103438869));
#30420=CARTESIAN_POINT('Ctrl Pts',(28.254481539011,-31.5399727189289,1.44553527377015));
#30421=CARTESIAN_POINT('Ctrl Pts',(29.0567817440806,-31.5374655658645,1.50856328668892));
#30422=CARTESIAN_POINT('Ctrl Pts',(29.4392037716731,-31.5366692491296,1.53093305020556));
#30423=CARTESIAN_POINT('Ctrl Pts',(29.9281985709061,-31.536168682902,1.54360558359609));
#30424=CARTESIAN_POINT('Ctrl Pts',(30.4627354290944,-31.5360567738141,1.54671304059522));
#30425=CARTESIAN_POINT('Ctrl Pts',(31.5039222132188,-31.5366047697957,1.53240580330097));
#30426=CARTESIAN_POINT('Ctrl Pts',(32.3686614831274,-31.5379963364647,1.49961223537189));
#30427=CARTESIAN_POINT('Ctrl Pts',(33.1596379899179,-31.5379973429874,1.49979803313559));
#30428=CARTESIAN_POINT('Ctrl Pts',(33.4544864001145,-31.5379973136915,1.49979103760184));
#30429=CARTESIAN_POINT('Ctrl Pts',(33.7806952343975,-31.5379974331442,1.49981257637976));
#30430=CARTESIAN_POINT('Ctrl Pts',(34.2756055948936,-31.5379974633363,1.49981748473541));
#30431=CARTESIAN_POINT('Ctrl Pts',(34.8099061252942,-31.5379977492716,1.49986722177693));
#30432=CARTESIAN_POINT('Ctrl Pts',(35.6331043028646,-31.5379977889784,1.49987402634113));
#30433=CARTESIAN_POINT('Ctrl Pts',(36.2913385913736,-31.5379978644599,1.49988713966987));
#30434=CARTESIAN_POINT('Ctrl Pts',(38.1019015852784,-31.537997968394,1.49990511666357));
#30435=CARTESIAN_POINT('Ctrl Pts',(39.5833333333333,-31.5379985160061,1.5));
#30436=CARTESIAN_POINT('Ctrl Pts',(40.9,-31.5379985160061,1.5));
#30437=CARTESIAN_POINT('Ctrl Pts',(6.37427268165564,-28.1741189428499,-20.7176664141567));
#30438=CARTESIAN_POINT('Ctrl Pts',(6.46448755772838,-28.2883460540946,-20.5636424771022));
#30439=CARTESIAN_POINT('Ctrl Pts',(6.55522687426754,-28.4011972468989,-20.4088293925213));
#30440=CARTESIAN_POINT('Ctrl Pts',(7.61282240204204,-29.6937878962761,-18.6056139772311));
#30441=CARTESIAN_POINT('Ctrl Pts',(8.61454082730176,-30.703424507615,-16.8370699794085));
#30442=CARTESIAN_POINT('Ctrl Pts',(10.6618274824665,-32.3104201819496,-13.5325068155167));
#30443=CARTESIAN_POINT('Ctrl Pts',(11.6645377987076,-32.9144254040795,-11.9110180488693));
#30444=CARTESIAN_POINT('Ctrl Pts',(13.7331445959134,-33.8529424117878,-8.96386257277558));
#30445=CARTESIAN_POINT('Ctrl Pts',(14.7439932704909,-34.1658004948675,-7.56674532731094));
#30446=CARTESIAN_POINT('Ctrl Pts',(16.8461035490385,-34.6388264066738,-5.10012840374637));
#30447=CARTESIAN_POINT('Ctrl Pts',(17.8695058124616,-34.7622645166785,-3.97333364734334));
#30448=CARTESIAN_POINT('Ctrl Pts',(19.2561174443541,-34.8817349492475,-2.73821070416468));
#30449=CARTESIAN_POINT('Ctrl Pts',(19.7609345646798,-34.9159214541564,-2.30176586395498));
#30450=CARTESIAN_POINT('Ctrl Pts',(20.8205141053453,-34.9621410370326,-1.45015687002428));
#30451=CARTESIAN_POINT('Ctrl Pts',(21.6560023791939,-34.9776907709078,-0.871078443386996));
#30452=CARTESIAN_POINT('Ctrl Pts',(22.3682688599883,-34.989939594886,-0.447778285927136));
#30453=CARTESIAN_POINT('Ctrl Pts',(22.6285200842947,-34.9931281975259,-0.297086276283262));
#30454=CARTESIAN_POINT('Ctrl Pts',(23.1658603614091,-34.9961605697035,-0.00273379297027992));
#30455=CARTESIAN_POINT('Ctrl Pts',(23.8505975407037,-34.9944676948756,0.338068372298851));
#30456=CARTESIAN_POINT('Ctrl Pts',(24.5583968797874,-34.9894056975888,0.638319272935676));
#30457=CARTESIAN_POINT('Ctrl Pts',(25.0640148551739,-34.9860476379143,0.821498314632841));
#30458=CARTESIAN_POINT('Ctrl Pts',(25.3563632502514,-34.9844821378475,0.917977493583092));
#30459=CARTESIAN_POINT('Ctrl Pts',(25.503160007456,-34.9838621425449,0.963163948801066));
#30460=CARTESIAN_POINT('Ctrl Pts',(26.0049713545738,-34.982139121313,1.11209382847184));
#30461=CARTESIAN_POINT('Ctrl Pts',(27.1869304722337,-34.9762666166019,1.35965020681436));
#30462=CARTESIAN_POINT('Ctrl Pts',(28.2418054197051,-34.9698003983093,1.43886806122646));
#30463=CARTESIAN_POINT('Ctrl Pts',(29.0450356043991,-34.9673414359535,1.5089275405599));
#30464=CARTESIAN_POINT('Ctrl Pts',(29.4328041419752,-34.9665583691038,1.53413528152413));
#30465=CARTESIAN_POINT('Ctrl Pts',(29.9251825362975,-34.9660664512209,1.54824951859995));
#30466=CARTESIAN_POINT('Ctrl Pts',(30.4634799414205,-34.9659564211645,1.55174636239756));
#30467=CARTESIAN_POINT('Ctrl Pts',(31.5090833787051,-34.9664954410524,1.53574598606796));
#30468=CARTESIAN_POINT('Ctrl Pts',(32.3725304400172,-34.9678633362529,1.49952340891733));
#30469=CARTESIAN_POINT('Ctrl Pts',(33.1591152593399,-34.9678645826042,1.49975189997366));
#30470=CARTESIAN_POINT('Ctrl Pts',(33.4547063903441,-34.9678645463389,1.49974326694616));
#30471=CARTESIAN_POINT('Ctrl Pts',(33.7805921021893,-34.9678646942577,1.49976974530861));
#30472=CARTESIAN_POINT('Ctrl Pts',(34.2756282408745,-34.9678647316484,1.49977576894615));
#30473=CARTESIAN_POINT('Ctrl Pts',(34.8098603973427,-34.967865085736,1.49983687714898));
#30474=CARTESIAN_POINT('Ctrl Pts',(35.6330886763766,-34.9678651349076,1.49984523535833));
#30475=CARTESIAN_POINT('Ctrl Pts',(36.2913112329655,-34.9678652283802,1.49986134640235));
#30476=CARTESIAN_POINT('Ctrl Pts',(38.1018888107018,-34.9678653570876,1.49988343135295));
#30477=CARTESIAN_POINT('Ctrl Pts',(39.5833333333333,-34.9678660352249,1.5));
#30478=CARTESIAN_POINT('Ctrl Pts',(40.9,-34.9678660352249,1.5));
#30479=CARTESIAN_POINT('',(40.9,-32.9658914637539,1.50000000000002));
#30480=CARTESIAN_POINT('Ctrl Pts',(40.9,-32.9658914637539,1.50000000000002));
#30481=CARTESIAN_POINT('Ctrl Pts',(40.9,-33.466386268912,1.50000000000002));
#30482=CARTESIAN_POINT('Ctrl Pts',(40.9,-33.9668810740701,1.50000000000002));
#30483=CARTESIAN_POINT('Ctrl Pts',(40.9,-34.4673758792282,1.50000000000002));
#30484=CARTESIAN_POINT('',(38.,-32.9658914637539,1.49999999999999));
#30485=CARTESIAN_POINT('Ctrl Pts',(38.,-32.9658914637539,1.5));
#30486=CARTESIAN_POINT('Ctrl Pts',(38.9666666666667,-32.9658914637539,1.5));
#30487=CARTESIAN_POINT('Ctrl Pts',(39.9333333333333,-32.9658914637539,1.5));
#30488=CARTESIAN_POINT('Ctrl Pts',(40.9,-32.9658914637539,1.5));
#30489=CARTESIAN_POINT('Ctrl Pts',(37.4997714574611,-32.3652585803353,1.49990106437153));
#30490=CARTESIAN_POINT('Ctrl Pts',(37.6667294826967,-32.5658056765356,1.4999047077905));
#30491=CARTESIAN_POINT('Ctrl Pts',(37.8334450600886,-32.7660568372682,1.49990923999261));
#30492=CARTESIAN_POINT('Ctrl Pts',(37.9998166694663,-32.9658909678229,1.49991439209149));
#30493=CARTESIAN_POINT('',(6.9,-24.7737885487526,-16.9192021366758));
#30494=CARTESIAN_POINT('Ctrl Pts',(6.9,-24.7737885487526,-16.9192021366758));
#30495=CARTESIAN_POINT('Ctrl Pts',(6.9,-22.645444622876,-15.3881766950258));
#30496=CARTESIAN_POINT('Ctrl Pts',(6.90000000000115,-20.4978726403359,-13.8353835251886));
#30497=CARTESIAN_POINT('Ctrl Pts',(6.90000000000115,-15.662481608859,-10.3082122779765));
#30498=CARTESIAN_POINT('Ctrl Pts',(6.9,-12.4764228571341,-7.95935811114668));
#30499=CARTESIAN_POINT('Ctrl Pts',(6.9,-9.46599415782505,-5.6597919716369));
#30500=CARTESIAN_POINT('',(22.9245129145126,-31.7706052331164,3.89077700057102E-15));
#30501=CARTESIAN_POINT('Ctrl Pts',(22.9245129145126,-31.7706052331164,8.19538942818498E-15));
#30502=CARTESIAN_POINT('Ctrl Pts',(22.7202811020963,-31.7014549124251,-0.0979233563002608));
#30503=CARTESIAN_POINT('Ctrl Pts',(22.5089075447093,-31.6320805544326,-0.203440182623869));
#30504=CARTESIAN_POINT('Ctrl Pts',(22.2913349439917,-31.5632247707622,-0.316637134194163));
#30505=CARTESIAN_POINT('Ctrl Pts',(21.4451770585293,-31.2954389184984,-0.756869465221139));
#30506=CARTESIAN_POINT('Ctrl Pts',(20.5220951556669,-31.0475106147151,-1.35418571023217));
#30507=CARTESIAN_POINT('Ctrl Pts',(19.767142881954,-30.8612920963158,-1.89915402350694));
#30508=CARTESIAN_POINT('Ctrl Pts',(19.5194773058392,-30.8002022522972,-2.07793339270825));
#30509=CARTESIAN_POINT('Ctrl Pts',(19.2865716386091,-30.7444068279678,-2.2520483595932));
#30510=CARTESIAN_POINT('Ctrl Pts',(19.0728538401323,-30.6939488833522,-2.41532203906683));
#30511=CARTESIAN_POINT('Ctrl Pts',(18.7028555998036,-30.6065937315988,-2.69798906318808));
#30512=CARTESIAN_POINT('Ctrl Pts',(18.4144703596236,-30.539966063932,-2.9337393828771));
#30513=CARTESIAN_POINT('Ctrl Pts',(18.0642874871539,-30.4582462938821,-3.23398234069981));
#30514=CARTESIAN_POINT('Ctrl Pts',(17.4420927116722,-30.3130489756353,-3.76744532366912));
#30515=CARTESIAN_POINT('Ctrl Pts',(16.7224564418219,-30.1446863488622,-4.43872907330226));
#30516=CARTESIAN_POINT('Ctrl Pts',(15.9202806616111,-29.9321297384067,-5.24401550821529));
#30517=CARTESIAN_POINT('Ctrl Pts',(15.4090529834519,-29.7966671314304,-5.75722561070116));
#30518=CARTESIAN_POINT('Ctrl Pts',(14.8739602945715,-29.6418940055915,-6.33424649579652));
#30519=CARTESIAN_POINT('Ctrl Pts',(14.3169794331156,-29.4557634846122,-6.96996102647202));
#30520=CARTESIAN_POINT('Ctrl Pts',(13.8864206762837,-29.3118803976569,-7.4613826837838));
#30521=CARTESIAN_POINT('Ctrl Pts',(13.3867890027805,-29.1311705407939,-8.05270459511993));
#30522=CARTESIAN_POINT('Ctrl Pts',(12.8146824059514,-28.8915984033895,-8.75043091662868));
#30523=CARTESIAN_POINT('Ctrl Pts',(12.2526665517595,-28.6562518085588,-9.4358508309389));
#30524=CARTESIAN_POINT('Ctrl Pts',(11.6379478462804,-28.3625845909803,-10.231366276768));
#30525=CARTESIAN_POINT('Ctrl Pts',(10.9739250490309,-27.981021293096,-11.1267230319105));
#30526=CARTESIAN_POINT('Ctrl Pts',(10.5683455447964,-27.747965660321,-11.6735993596027));
#30527=CARTESIAN_POINT('Ctrl Pts',(10.1437415406956,-27.4801235315866,-12.2581093618546));
#30528=CARTESIAN_POINT('Ctrl Pts',(9.74137929176525,-27.2046666925187,-12.8142541611144));
#30529=CARTESIAN_POINT('Ctrl Pts',(8.72285779294234,-26.5073877769786,-14.2220538143138));
#30530=CARTESIAN_POINT('Ctrl Pts',(7.81323138778195,-25.7100913255874,-15.580948814124));
#30531=CARTESIAN_POINT('Ctrl Pts',(6.9,-24.7737885487526,-16.9192021366758));
#30532=CARTESIAN_POINT('Ctrl Pts',(30.5,-34.9656486014478,1.55029606206997));
#30533=CARTESIAN_POINT('Ctrl Pts',(29.9560179420817,-34.7222276068062,1.55343104498103));
#30534=CARTESIAN_POINT('Ctrl Pts',(29.4152668325132,-34.4790656554127,1.54030953139106));
#30535=CARTESIAN_POINT('Ctrl Pts',(28.8740459957565,-34.2361296888632,1.49470250846617));
#30536=CARTESIAN_POINT('Ctrl Pts',(28.3535277923439,-34.0024864433252,1.45084003307051));
#30537=CARTESIAN_POINT('Ctrl Pts',(27.8179515912466,-33.7608540997398,1.40923473841146));
#30538=CARTESIAN_POINT('Ctrl Pts',(27.2695051149491,-33.5168388499063,1.33972398862116));
#30539=CARTESIAN_POINT('Ctrl Pts',(26.9554553615883,-33.3771115796287,1.29992095446743));
#30540=CARTESIAN_POINT('Ctrl Pts',(26.6378099296971,-33.2369493090937,1.25106463707208));
#30541=CARTESIAN_POINT('Ctrl Pts',(26.3179304017917,-33.0983258448229,1.18777049128279));
#30542=CARTESIAN_POINT('Ctrl Pts',(26.1078196745982,-33.0072719500184,1.14619615520081));
#30543=CARTESIAN_POINT('Ctrl Pts',(25.8967402232745,-32.9168907470981,1.09839525532295));
#30544=CARTESIAN_POINT('Ctrl Pts',(25.6850706236774,-32.8277596053404,1.04282885388103));
#30545=CARTESIAN_POINT('Ctrl Pts',(25.6562210027417,-32.8156114288513,1.03525540156945));
#30546=CARTESIAN_POINT('Ctrl Pts',(25.6277737638215,-32.8036595933923,1.0276506122434));
#30547=CARTESIAN_POINT('Ctrl Pts',(25.5983858063598,-32.7913423709803,1.01964325944536));
#30548=CARTESIAN_POINT('Ctrl Pts',(25.1249357452756,-32.5929076988546,0.890642063078175));
#30549=CARTESIAN_POINT('Ctrl Pts',(24.1510084067019,-32.1858811669087,0.588069770626606));
#30550=CARTESIAN_POINT('Ctrl Pts',(22.9245129145126,-31.7706052331164,8.19538942818498E-15));
#30551=CARTESIAN_POINT('Origin',(40.65,0.,0.));
#30552=CARTESIAN_POINT('',(40.4,-29.5330398077868,-18.7829592905825));
#30553=CARTESIAN_POINT('',(40.9,-29.0996231131986,-18.5327260452907));
#30554=CARTESIAN_POINT('Ctrl Pts',(40.4,-29.5330398077868,-18.7829592905825));
#30555=CARTESIAN_POINT('Ctrl Pts',(40.5666590133561,-29.3885761367562,-18.6995531512249));
#30556=CARTESIAN_POINT('Ctrl Pts',(40.7333430448979,-29.2440888807198,-18.6161333950578));
#30557=CARTESIAN_POINT('Ctrl Pts',(40.9,-29.0996231131986,-18.5327260452907));
#30558=CARTESIAN_POINT('',(40.9,-30.5996231131986,-15.9346498339374));
#30559=CARTESIAN_POINT('Origin',(40.9,0.,0.));
#30560=CARTESIAN_POINT('',(40.4,-31.0330398077868,-16.1848830792292));
#30561=CARTESIAN_POINT('Ctrl Pts',(40.9,-30.5996231131986,-15.9346498339374));
#30562=CARTESIAN_POINT('Ctrl Pts',(40.7333430441722,-30.7440888813489,-16.0180571840677));
#30563=CARTESIAN_POINT('Ctrl Pts',(40.566659012132,-30.8885761378173,-16.1014769404842));
#30564=CARTESIAN_POINT('Ctrl Pts',(40.4,-31.0330398077868,-16.1848830792292));
#30565=CARTESIAN_POINT('Origin',(40.4,0.,0.));
#30566=CARTESIAN_POINT('Origin',(35.7,0.,0.));
#30567=CARTESIAN_POINT('',(30.5,-31.0562879796886,-16.1402285275843));
#30568=CARTESIAN_POINT('Ctrl Pts',(40.3999012894849,-31.0330346270951,-16.1848928782182));
#30569=CARTESIAN_POINT('Ctrl Pts',(39.2494626810401,-31.0330116996609,-16.1849362443212));
#30570=CARTESIAN_POINT('Ctrl Pts',(38.0976708836827,-31.0329190263647,-16.1851115327779));
#30571=CARTESIAN_POINT('Ctrl Pts',(36.9467340384722,-31.0328856894587,-16.1851746119074));
#30572=CARTESIAN_POINT('Ctrl Pts',(36.745427730736,-31.0328798586179,-16.1851856448556));
#30573=CARTESIAN_POINT('Ctrl Pts',(36.5441475779312,-31.0328758430124,-16.1851932450652));
#30574=CARTESIAN_POINT('Ctrl Pts',(36.3429119519248,-31.0328722727085,-16.1852000001162));
#30575=CARTESIAN_POINT('Ctrl Pts',(36.2102758775793,-31.0328699194915,-16.1852044524264));
#30576=CARTESIAN_POINT('Ctrl Pts',(36.0822774296292,-31.0328678560427,-16.1852084224022));
#30577=CARTESIAN_POINT('Ctrl Pts',(35.9587202262685,-31.0328657167444,-16.1852125810273));
#30578=CARTESIAN_POINT('Ctrl Pts',(35.7925662245339,-31.0328628399153,-16.1852181733537));
#30579=CARTESIAN_POINT('Ctrl Pts',(35.6344388155495,-31.0328598211428,-16.1852241162451));
#30580=CARTESIAN_POINT('Ctrl Pts',(35.4837714463462,-31.0328562161519,-16.1852312078525));
#30581=CARTESIAN_POINT('Ctrl Pts',(35.3175474553587,-31.0328522389406,-16.1852390316785));
#30582=CARTESIAN_POINT('Ctrl Pts',(35.1604041224823,-31.0328475520712,-16.1852482463283));
#30583=CARTESIAN_POINT('Ctrl Pts',(35.0116427948696,-31.0328419178902,-16.1852592402396));
#30584=CARTESIAN_POINT('Ctrl Pts',(34.9979272091156,-31.0328413984266,-16.1852602538628));
#30585=CARTESIAN_POINT('Ctrl Pts',(34.9842829110377,-31.0328408711131,-16.1852612822245));
#30586=CARTESIAN_POINT('Ctrl Pts',(34.9707093736271,-31.0328403358796,-16.1852623254083));
#30587=CARTESIAN_POINT('Ctrl Pts',(34.8522491799022,-31.0328356647415,-16.1852714295753));
#30588=CARTESIAN_POINT('Ctrl Pts',(34.7391835006528,-31.0328304196802,-16.1852816068676));
#30589=CARTESIAN_POINT('Ctrl Pts',(34.6312849042886,-31.0328252639046,-16.1852915612822));
#30590=CARTESIAN_POINT('Ctrl Pts',(34.509679526085,-31.0328194531707,-16.1853027802452));
#30591=CARTESIAN_POINT('Ctrl Pts',(34.3946370581325,-31.0328137541412,-16.1853137193613));
#30592=CARTESIAN_POINT('Ctrl Pts',(34.2857585821187,-31.0328086821745,-16.1853233495613));
#30593=CARTESIAN_POINT('Ctrl Pts',(34.178680190815,-31.0328036940624,-16.1853328205454));
#30594=CARTESIAN_POINT('Ctrl Pts',(34.0775620514826,-31.03279930319,-16.1853410431659));
#30595=CARTESIAN_POINT('Ctrl Pts',(33.9819758246426,-31.0327957057951,-16.1853475980774));
#30596=CARTESIAN_POINT('Ctrl Pts',(33.9184449689726,-31.0327933148066,-16.185351954763));
#30597=CARTESIAN_POINT('Ctrl Pts',(33.8573517602304,-31.0327912624253,-16.1853555977386));
#30598=CARTESIAN_POINT('Ctrl Pts',(33.7984399511825,-31.0327894081823,-16.1853587887284));
#30599=CARTESIAN_POINT('Ctrl Pts',(33.7337970612212,-31.0327873735542,-16.1853622901452));
#30600=CARTESIAN_POINT('Ctrl Pts',(33.671780974268,-31.0327855776264,-16.1853652470741));
#30601=CARTESIAN_POINT('Ctrl Pts',(33.6121191806453,-31.0327838881566,-16.1853678991827));
#30602=CARTESIAN_POINT('Ctrl Pts',(33.5695978710647,-31.0327826840616,-16.185369789356));
#30603=CARTESIAN_POINT('Ctrl Pts',(33.5282738752656,-31.0327815352148,-16.1853715223629));
#30604=CARTESIAN_POINT('Ctrl Pts',(33.4880643388297,-31.0327804070619,-16.1853731585247));
#30605=CARTESIAN_POINT('Ctrl Pts',(33.4508270573206,-31.0327793623012,-16.1853746737427));
#30606=CARTESIAN_POINT('Ctrl Pts',(33.4145509216557,-31.0327783314861,-16.1853761126591));
#30607=CARTESIAN_POINT('Ctrl Pts',(33.3793439789548,-31.0327771639656,-16.1853777420672));
#30608=CARTESIAN_POINT('Ctrl Pts',(33.3411337035362,-31.0327758968497,-16.1853795104722));
#30609=CARTESIAN_POINT('Ctrl Pts',(33.3041826660689,-31.032774468878,-16.1853815029501));
#30610=CARTESIAN_POINT('Ctrl Pts',(33.2685652776782,-31.0327727495065,-16.1853839484228));
#30611=CARTESIAN_POINT('Ctrl Pts',(33.2310094474552,-31.0327709365598,-16.185386526988));
#30612=CARTESIAN_POINT('Ctrl Pts',(33.1949357943683,-31.0327688002291,-16.1853896081159));
#30613=CARTESIAN_POINT('Ctrl Pts',(33.1603699172396,-31.0327662471214,-16.1853933524012));
#30614=CARTESIAN_POINT('Ctrl Pts',(33.1223715679422,-31.032763440484,-16.1853974685027));
#30615=CARTESIAN_POINT('Ctrl Pts',(33.0861949166479,-31.0327601306122,-16.1854023852332));
#30616=CARTESIAN_POINT('Ctrl Pts',(33.0518089354077,-31.0327562557941,-16.1854082033113));
#30617=CARTESIAN_POINT('Ctrl Pts',(33.0341030813061,-31.0327542605925,-16.1854111991264));
#30618=CARTESIAN_POINT('Ctrl Pts',(33.0168710360022,-31.0327521165229,-16.1854144322605));
#30619=CARTESIAN_POINT('Ctrl Pts',(33.0001033802534,-31.0327498200703,-16.1854179076006));
#30620=CARTESIAN_POINT('Ctrl Pts',(32.9420348133411,-31.0327418671572,-16.1854299431543));
#30621=CARTESIAN_POINT('Ctrl Pts',(32.8874145324496,-31.0328461364756,-16.1852296143113));
#30622=CARTESIAN_POINT('Ctrl Pts',(32.8357863520581,-31.0330149777622,-16.1849068811705));
#30623=CARTESIAN_POINT('Ctrl Pts',(32.7779739682631,-31.0332040434466,-16.1845454899291));
#30624=CARTESIAN_POINT('Ctrl Pts',(32.7239136589684,-31.0334742654592,-16.1840302574574));
#30625=CARTESIAN_POINT('Ctrl Pts',(32.6729278684753,-31.0337854095719,-16.1834371021678));
#30626=CARTESIAN_POINT('Ctrl Pts',(32.618080133626,-31.0341201214521,-16.1827990180322));
#30627=CARTESIAN_POINT('Ctrl Pts',(32.5667902508429,-31.0345025939174,-16.1820699950121));
#30628=CARTESIAN_POINT('Ctrl Pts',(32.5181731636795,-31.0349066963829,-16.1812992842338));
#30629=CARTESIAN_POINT('Ctrl Pts',(32.4659536029864,-31.0353407424037,-16.1804714646211));
#30630=CARTESIAN_POINT('Ctrl Pts',(32.4168175136244,-31.0358001425893,-16.1795947944395));
#30631=CARTESIAN_POINT('Ctrl Pts',(32.3696233879008,-31.0362725138778,-16.1786925325961));
#30632=CARTESIAN_POINT('Ctrl Pts',(32.3182581618429,-31.0367866341766,-16.1777105272545));
#30633=CARTESIAN_POINT('Ctrl Pts',(32.2691934412647,-31.0373164741887,-16.1766975364928));
#30634=CARTESIAN_POINT('Ctrl Pts',(32.2209064724826,-31.0378627004432,-16.1756521425246));
#30635=CARTESIAN_POINT('Ctrl Pts',(32.1715370438648,-31.0384211715745,-16.1745833137247));
#30636=CARTESIAN_POINT('Ctrl Pts',(32.1229805798606,-31.0389971805318,-16.173479840102));
#30637=CARTESIAN_POINT('Ctrl Pts',(32.0735591134784,-31.0396018563639,-16.1723205501866));
#30638=CARTESIAN_POINT('Ctrl Pts',(32.0254239419645,-31.0401907942691,-16.1711914331652));
#30639=CARTESIAN_POINT('Ctrl Pts',(31.9764682879415,-31.04080728099,-16.1700086968176));
#30640=CARTESIAN_POINT('Ctrl Pts',(31.9250947921527,-31.0414657598839,-16.1687449477338));
#30641=CARTESIAN_POINT('Ctrl Pts',(31.8952919104886,-31.0418477578043,-16.168011819419));
#30642=CARTESIAN_POINT('Ctrl Pts',(31.8646744620481,-31.0422439429541,-16.1672513233695));
#30643=CARTESIAN_POINT('Ctrl Pts',(31.8329224323944,-31.0426570718778,-16.1664582369103));
#30644=CARTESIAN_POINT('Ctrl Pts',(31.7319354368356,-31.0439710240641,-16.163935833788));
#30645=CARTESIAN_POINT('Ctrl Pts',(31.6284526822056,-31.0453389332578,-16.1613063818565));
#30646=CARTESIAN_POINT('Ctrl Pts',(31.5232336354318,-31.0466795487251,-16.1587277943726));
#30647=CARTESIAN_POINT('Ctrl Pts',(31.4188807866258,-31.0480091278027,-16.156170434673));
#30648=CARTESIAN_POINT('Ctrl Pts',(31.3128198672039,-31.0493111005242,-16.1536645426213));
#30649=CARTESIAN_POINT('Ctrl Pts',(31.205840297043,-31.0505011542276,-16.1513736799427));
#30650=CARTESIAN_POINT('Ctrl Pts',(31.1464339374067,-31.0511619977717,-16.1501015509562));
#30651=CARTESIAN_POINT('Ctrl Pts',(31.0867451889522,-31.0517883042759,-16.1488957763821));
#30652=CARTESIAN_POINT('Ctrl Pts',(31.0269161235858,-31.0523662912129,-16.1477831210733));
#30653=CARTESIAN_POINT('Ctrl Pts',(30.9223727403119,-31.0533762469847,-16.1458389029967));
#30654=CARTESIAN_POINT('Ctrl Pts',(30.8173993541569,-31.0542375463395,-16.1441811147896));
#30655=CARTESIAN_POINT('Ctrl Pts',(30.7129204018003,-31.0548748925162,-16.1429541726494));
#30656=CARTESIAN_POINT('Ctrl Pts',(30.6397146645873,-31.0553214647268,-16.1420944855846));
#30657=CARTESIAN_POINT('Ctrl Pts',(30.5667525557982,-31.0556583368408,-16.1414458510594));
#30658=CARTESIAN_POINT('Ctrl Pts',(30.4943593393941,-31.055866014916,-16.1410459118957));
#30659=CARTESIAN_POINT('',(30.5,-29.559989655385,-18.7405179110273));
#30660=CARTESIAN_POINT('Origin',(30.5,0.,0.));
#30661=CARTESIAN_POINT('Ctrl Pts',(30.5049791805003,-29.5605178050973,-18.7395177484758));
#30662=CARTESIAN_POINT('Ctrl Pts',(30.5973676827744,-29.560162264643,-18.7400797009803));
#30663=CARTESIAN_POINT('Ctrl Pts',(30.6891105694845,-29.559542510155,-18.7410567560113));
#30664=CARTESIAN_POINT('Ctrl Pts',(30.780677479308,-29.5587264396735,-18.7423441244048));
#30665=CARTESIAN_POINT('Ctrl Pts',(30.8441888930629,-29.5581604077948,-18.7432370516298));
#30666=CARTESIAN_POINT('Ctrl Pts',(30.9076166453417,-29.5574994222392,-18.7442800408076));
#30667=CARTESIAN_POINT('Ctrl Pts',(30.971128809674,-29.5567612578201,-18.7454455999911));
#30668=CARTESIAN_POINT('Ctrl Pts',(31.0735567068111,-29.5555707987955,-18.7473253308648));
#30669=CARTESIAN_POINT('Ctrl Pts',(31.1762019082914,-29.5541800414699,-18.7495231556641));
#30670=CARTESIAN_POINT('Ctrl Pts',(31.2798872709469,-29.5526737444515,-18.7519033574722));
#30671=CARTESIAN_POINT('Ctrl Pts',(31.3828989348284,-29.5511772346435,-18.7542680938472));
#30672=CARTESIAN_POINT('Ctrl Pts',(31.4869372222156,-29.5495656759358,-18.7568144117911));
#30673=CARTESIAN_POINT('Ctrl Pts',(31.5928574097494,-29.5479181178243,-18.7594156373086));
#30674=CARTESIAN_POINT('Ctrl Pts',(31.6516459294338,-29.5470036792766,-18.7608593866173));
#30675=CARTESIAN_POINT('Ctrl Pts',(31.7110150391233,-29.5460781618907,-18.7623200347852));
#30676=CARTESIAN_POINT('Ctrl Pts',(31.7711176725243,-29.5451562912556,-18.763774049131));
#30677=CARTESIAN_POINT('Ctrl Pts',(31.8409082760365,-29.5440858238842,-18.7654624366936));
#30678=CARTESIAN_POINT('Ctrl Pts',(31.9056373311747,-29.5431152615715,-18.7669933631241));
#30679=CARTESIAN_POINT('Ctrl Pts',(31.9658882086283,-29.5422441375119,-18.768367583494));
#30680=CARTESIAN_POINT('Ctrl Pts',(32.0341093482756,-29.5412577771694,-18.7699235920325));
#30681=CARTESIAN_POINT('Ctrl Pts',(32.0965888127923,-29.5403982847666,-18.7712796560443));
#30682=CARTESIAN_POINT('Ctrl Pts',(32.1542362617661,-29.5396480149485,-18.7724634074923));
#30683=CARTESIAN_POINT('Ctrl Pts',(32.2151538519835,-29.5388551849075,-18.773714309083));
#30684=CARTESIAN_POINT('Ctrl Pts',(32.2706761902198,-29.5381836213574,-18.7747738843965));
#30685=CARTESIAN_POINT('Ctrl Pts',(32.3219402247771,-29.5376060245818,-18.7756849339009));
#30686=CARTESIAN_POINT('Ctrl Pts',(32.3761674213258,-29.536995041577,-18.776648643858));
#30687=CARTESIAN_POINT('Ctrl Pts',(32.4256304058851,-29.5364887148648,-18.7774469218492));
#30688=CARTESIAN_POINT('Ctrl Pts',(32.4717350314077,-29.5360572749797,-18.7781265619113));
#30689=CARTESIAN_POINT('Ctrl Pts',(32.5214923281262,-29.5355916539681,-18.7788600469327));
#30690=CARTESIAN_POINT('Ctrl Pts',(32.5673384642532,-29.5352128774493,-18.7794559410667));
#30691=CARTESIAN_POINT('Ctrl Pts',(32.6111004962934,-29.5348934788928,-18.7799576530151));
#30692=CARTESIAN_POINT('Ctrl Pts',(32.6551147163181,-29.5345722397344,-18.780462256185));
#30693=CARTESIAN_POINT('Ctrl Pts',(32.6970214084871,-29.5343108907558,-18.7808718608789));
#30694=CARTESIAN_POINT('Ctrl Pts',(32.7387279964579,-29.5340950825232,-18.7812095285095));
#30695=CARTESIAN_POINT('Ctrl Pts',(32.7800761354879,-29.5338811290631,-18.781544294042));
#30696=CARTESIAN_POINT('Ctrl Pts',(32.8212277342351,-29.5337116838824,-18.7818087481603));
#30697=CARTESIAN_POINT('Ctrl Pts',(32.8640829337527,-29.5335890251804,-18.782000095504));
#30698=CARTESIAN_POINT('Ctrl Pts',(32.9037320332532,-29.5334755428695,-18.7821771276952));
#30699=CARTESIAN_POINT('Ctrl Pts',(32.9448394203921,-29.5334018918637,-18.7822919200911));
#30700=CARTESIAN_POINT('Ctrl Pts',(32.9889438598256,-29.5333868654406,-18.7823158450367));
#30701=CARTESIAN_POINT('Ctrl Pts',(32.992510226926,-29.5333856503761,-18.7823177796524));
#30702=CARTESIAN_POINT('Ctrl Pts',(32.9960962106242,-29.5333848297968,-18.7823191027633));
#30703=CARTESIAN_POINT('Ctrl Pts',(32.9997026353889,-29.5333844198653,-18.7823197895506));
#30704=CARTESIAN_POINT('Ctrl Pts',(33.0361388185046,-29.5333802782743,-18.7823267282529));
#30705=CARTESIAN_POINT('Ctrl Pts',(33.0740002606605,-29.5333765562528,-18.7823330770045));
#30706=CARTESIAN_POINT('Ctrl Pts',(33.1140504028668,-29.5333733966326,-18.7823389179975));
#30707=CARTESIAN_POINT('Ctrl Pts',(33.2460690464807,-29.5333629814689,-18.7823581718611));
#30708=CARTESIAN_POINT('Ctrl Pts',(33.3720922029406,-29.5333587011923,-18.7823661897829));
#30709=CARTESIAN_POINT('Ctrl Pts',(33.4992849360726,-29.5333546566756,-18.782373736073));
#30710=CARTESIAN_POINT('Ctrl Pts',(33.6626792864138,-29.5333494610079,-18.7823834301894));
#30711=CARTESIAN_POINT('Ctrl Pts',(33.8280037294637,-29.5333446544026,-18.7823923459959));
#30712=CARTESIAN_POINT('Ctrl Pts',(33.9928746198634,-29.5333373313072,-18.7824059536077));
#30713=CARTESIAN_POINT('Ctrl Pts',(34.322616400663,-29.5333226851165,-18.7824331688313));
#30714=CARTESIAN_POINT('Ctrl Pts',(34.6505439708621,-29.5332979729652,-18.7824791512758));
#30715=CARTESIAN_POINT('Ctrl Pts',(34.979144925286,-29.5332814027048,-18.7825099763789));
#30716=CARTESIAN_POINT('Ctrl Pts',(35.30774587971,-29.5332648324445,-18.782540801482));
#30717=CARTESIAN_POINT('Ctrl Pts',(35.6370202183589,-29.5332564040751,-18.7825564692435));
#30718=CARTESIAN_POINT('Ctrl Pts',(35.9661418060973,-29.5332492722834,-18.7825697306317));
#30719=CARTESIAN_POINT('Ctrl Pts',(36.2952633938358,-29.5332421404917,-18.7825829920199));
#30720=CARTESIAN_POINT('Ctrl Pts',(36.6242322306637,-29.5332363052777,-18.7825938470347));
#30721=CARTESIAN_POINT('Ctrl Pts',(36.9531363303404,-29.5332247108411,-18.7826154119861));
#30722=CARTESIAN_POINT('Ctrl Pts',(38.1022190076918,-29.5331842036954,-18.7826907528288));
#30723=CARTESIAN_POINT('Ctrl Pts',(39.2505115204485,-29.5330734009978,-18.782896816333));
#30724=CARTESIAN_POINT('Ctrl Pts',(40.400093943525,-29.533045998731,-18.7829477771169));
#30725=CARTESIAN_POINT('Ctrl Pts',(6.89999999997365,-5.3678954269134,-9.63452070648359));
#30726=CARTESIAN_POINT('Ctrl Pts',(6.99168932310453,-5.42175501956,-9.60499723839754));
#30727=CARTESIAN_POINT('Ctrl Pts',(7.08383915760479,-5.47527828673705,-9.57508016834563));
#30728=CARTESIAN_POINT('Ctrl Pts',(8.15762752947026,-6.09209251732962,-9.22342495405909));
#30729=CARTESIAN_POINT('Ctrl Pts',(9.16608342448598,-6.61836595106258,-8.84591675027098));
#30730=CARTESIAN_POINT('Ctrl Pts',(11.2535425311854,-7.53037930120419,-8.09542754093137));
#30731=CARTESIAN_POINT('Ctrl Pts',(12.2577133097063,-7.91666449612081,-7.7072500137176));
#30732=CARTESIAN_POINT('Ctrl Pts',(14.356433377742,-8.58141250110813,-6.97440810645327));
#30733=CARTESIAN_POINT('Ctrl Pts',(15.3659105035251,-8.8532231228606,-6.61345583116597));
#30734=CARTESIAN_POINT('Ctrl Pts',(17.4728641219044,-9.31281879192961,-5.96623757129007));
#30735=CARTESIAN_POINT('Ctrl Pts',(18.4890996814195,-9.49384943617776,-5.66020885204394));
#30736=CARTESIAN_POINT('Ctrl Pts',(19.8476172011441,-9.68599953593306,-5.32865724601648));
#30737=CARTESIAN_POINT('Ctrl Pts',(20.3454889307686,-9.75195458239816,-5.20930542916259));
#30738=CARTESIAN_POINT('Ctrl Pts',(21.3782040612024,-9.87366876552717,-4.97678151322346));
#30739=CARTESIAN_POINT('Ctrl Pts',(22.1792648896895,-9.95072592994711,-4.81935607344485));
#30740=CARTESIAN_POINT('Ctrl Pts',(22.8542621828908,-10.0067883222623,-4.70591921690553));
#30741=CARTESIAN_POINT('Ctrl Pts',(23.1054579010966,-10.0267605301623,-4.66456206383026));
#30742=CARTESIAN_POINT('Ctrl Pts',(23.6171513959784,-10.0644076466806,-4.58448144656257));
#30743=CARTESIAN_POINT('Ctrl Pts',(24.1360713221936,-10.0979855598765,-4.51012725444833));
#30744=CARTESIAN_POINT('Ctrl Pts',(24.6624927871863,-10.1277002159265,-4.44285620865164));
#30745=CARTESIAN_POINT('Ctrl Pts',(25.1928168818087,-10.1547862564439,-4.38095271718119));
#30746=CARTESIAN_POINT('Ctrl Pts',(25.5948982287614,-10.1721457030178,-4.34117176259642));
#30747=CARTESIAN_POINT('Ctrl Pts',(26.123203188965,-10.1922876384417,-4.29604941535506));
#30748=CARTESIAN_POINT('Ctrl Pts',(27.1768897027567,-10.2241871753182,-4.22326129112039));
#30749=CARTESIAN_POINT('Ctrl Pts',(28.2111297865347,-10.2325109692973,-4.19969555688312));
#30750=CARTESIAN_POINT('Ctrl Pts',(29.1277555719712,-10.2421056253617,-4.17661492679513));
#30751=CARTESIAN_POINT('Ctrl Pts',(29.4767605677586,-10.2448788784735,-4.17005614900019));
#30752=CARTESIAN_POINT('Ctrl Pts',(30.1601418995912,-10.2473221772452,-4.16421367130871));
#30753=CARTESIAN_POINT('Ctrl Pts',(31.3500242312262,-10.2457563290907,-4.16794387579263));
#30754=CARTESIAN_POINT('Ctrl Pts',(32.3461596131127,-10.2405791191156,-4.18040640609125));
#30755=CARTESIAN_POINT('Ctrl Pts',(33.1614718826737,-10.2405840900447,-4.18039330945983));
#30756=CARTESIAN_POINT('Ctrl Pts',(33.4925794155278,-10.2405841444578,-4.18039253080267));
#30757=CARTESIAN_POINT('Ctrl Pts',(34.1499904318885,-10.2405848392549,-4.18039030822713));
#30758=CARTESIAN_POINT('Ctrl Pts',(34.9738731541178,-10.2405865289643,-4.18038393925504));
#30759=CARTESIAN_POINT('Ctrl Pts',(35.9612754428241,-10.2405873001735,-4.18038119412747));
#30760=CARTESIAN_POINT('Ctrl Pts',(37.9366467881619,-10.2405882857914,-4.18037753677863));
#30761=CARTESIAN_POINT('Ctrl Pts',(39.5833333333333,-10.2405934798255,-4.18035859466987));
#30762=CARTESIAN_POINT('Ctrl Pts',(40.9,-10.2405934798255,-4.18035859466987));
#30763=CARTESIAN_POINT('Ctrl Pts',(6.71972576838711,-6.5764381714634,-12.8464244365415));
#30764=CARTESIAN_POINT('Ctrl Pts',(6.81144220747046,-6.6482837686261,-12.8102053989753));
#30765=CARTESIAN_POINT('Ctrl Pts',(6.90362823998598,-6.71971524922859,-12.7734498343709));
#30766=CARTESIAN_POINT('Ctrl Pts',(7.97787811486329,-7.54294881554194,-12.3410744046091));
#30767=CARTESIAN_POINT('Ctrl Pts',(8.98681832185142,-8.24809748747637,-11.871220138602));
#30768=CARTESIAN_POINT('Ctrl Pts',(11.0806583453373,-9.47774891389534,-10.9274240314556));
#30769=CARTESIAN_POINT('Ctrl Pts',(12.0862475175457,-10.0005505115845,-10.4368998098017));
#30770=CARTESIAN_POINT('Ctrl Pts',(14.197639322261,-10.906656993414,-9.50280276487817));
#30771=CARTESIAN_POINT('Ctrl Pts',(15.2100862637121,-11.2785931828498,-9.04203633254719));
#30772=CARTESIAN_POINT('Ctrl Pts',(17.3364698493953,-11.9121957711897,-8.20932952666152));
#30773=CARTESIAN_POINT('Ctrl Pts',(18.357279581038,-12.1627870018009,-7.81594677169137));
#30774=CARTESIAN_POINT('Ctrl Pts',(19.7331217809844,-12.4307568384137,-7.38628119283514));
#30775=CARTESIAN_POINT('Ctrl Pts',(20.2341927100357,-12.5225360922773,-7.23233618870703));
#30776=CARTESIAN_POINT('Ctrl Pts',(21.2777139275315,-12.6928916013278,-6.93114017240203));
#30777=CARTESIAN_POINT('Ctrl Pts',(22.0885637816417,-12.8012350092453,-6.72673758680645));
#30778=CARTESIAN_POINT('Ctrl Pts',(22.7734874647763,-12.8801738355232,-6.57909772915769));
#30779=CARTESIAN_POINT('Ctrl Pts',(23.0269571312138,-12.9082278965573,-6.52549682636865));
#30780=CARTESIAN_POINT('Ctrl Pts',(23.5444618566096,-12.9612738268022,-6.421485113254));
#30781=CARTESIAN_POINT('Ctrl Pts',(24.069438315646,-13.0087020921734,-6.32485290039691));
#30782=CARTESIAN_POINT('Ctrl Pts',(24.6027295908464,-13.0507741241225,-6.23730008137708));
#30783=CARTESIAN_POINT('Ctrl Pts',(25.140319252314,-13.0891677302171,-6.15667530541497));
#30784=CARTESIAN_POINT('Ctrl Pts',(25.5484689870705,-13.1137995888261,-6.1047965908769));
#30785=CARTESIAN_POINT('Ctrl Pts',(26.0852808149066,-13.1423647911197,-6.04589855121053));
#30786=CARTESIAN_POINT('Ctrl Pts',(27.1586857291268,-13.1877077660313,-5.95074158602806));
#30787=CARTESIAN_POINT('Ctrl Pts',(28.1995312980844,-13.1995114624862,-5.92039197700572));
#30788=CARTESIAN_POINT('Ctrl Pts',(29.1157533315887,-13.2130297822556,-5.89061060808304));
#30789=CARTESIAN_POINT('Ctrl Pts',(29.4698938670485,-13.2169740538761,-5.88204921070821));
#30790=CARTESIAN_POINT('Ctrl Pts',(30.1587234046997,-13.220429005539,-5.87447683559578));
#30791=CARTESIAN_POINT('Ctrl Pts',(31.3557311956059,-13.2182120926508,-5.87931523414857));
#30792=CARTESIAN_POINT('Ctrl Pts',(32.3501802435609,-13.2109234983781,-5.89537176970749));
#30793=CARTESIAN_POINT('Ctrl Pts',(33.1605031382465,-13.2109314016451,-5.89535013085606));
#30794=CARTESIAN_POINT('Ctrl Pts',(33.4922179295251,-13.2109314596682,-5.89534881762642));
#30795=CARTESIAN_POINT('Ctrl Pts',(34.1493400019897,-13.2109325467446,-5.89534512891166));
#30796=CARTESIAN_POINT('Ctrl Pts',(34.9735241318651,-13.2109351472382,-5.89533452524068));
#30797=CARTESIAN_POINT('Ctrl Pts',(35.9608954520826,-13.2109363413972,-5.8953299596426));
#30798=CARTESIAN_POINT('Ctrl Pts',(37.9363824842975,-13.2109378608691,-5.89532387223529));
#30799=CARTESIAN_POINT('Ctrl Pts',(39.5833333333333,-13.2109458830841,-5.89529235427929));
#30800=CARTESIAN_POINT('Ctrl Pts',(40.9,-13.2109458830841,-5.89529235427929));
#30801=CARTESIAN_POINT('Ctrl Pts',(6.48177011792014,-9.40621265917915,-20.336764848396));
#30802=CARTESIAN_POINT('Ctrl Pts',(6.57271435585529,-9.51911083717172,-20.2851799357091));
#30803=CARTESIAN_POINT('Ctrl Pts',(6.66411141569866,-9.63139437446865,-20.2327517601295));
#30804=CARTESIAN_POINT('Ctrl Pts',(7.73048017258431,-10.9276768808967,-19.614616528956));
#30805=CARTESIAN_POINT('Ctrl Pts',(8.73292722985417,-12.0456324995183,-18.9319609573801));
#30806=CARTESIAN_POINT('Ctrl Pts',(10.8102906905198,-14.0013807284478,-17.5485371602851));
#30807=CARTESIAN_POINT('Ctrl Pts',(11.8125687231201,-14.8418955382559,-16.8218444562665));
#30808=CARTESIAN_POINT('Ctrl Pts',(13.9177445864075,-16.3050153868123,-15.4271303717406));
#30809=CARTESIAN_POINT('Ctrl Pts',(14.9296562678442,-16.9116612373854,-14.7350649820735));
#30810=CARTESIAN_POINT('Ctrl Pts',(17.0680844879216,-17.9535844659564,-13.4708635112562));
#30811=CARTESIAN_POINT('Ctrl Pts',(18.0932339179161,-18.3688941094638,-12.8729609429));
#30812=CARTESIAN_POINT('Ctrl Pts',(19.4933464326808,-18.8183285494773,-12.2099892645604));
#30813=CARTESIAN_POINT('Ctrl Pts',(19.9993272808496,-18.971430097181,-11.9744841299437));
#30814=CARTESIAN_POINT('Ctrl Pts',(21.0600020168761,-19.2581324129063,-11.5100300116438));
#30815=CARTESIAN_POINT('Ctrl Pts',(21.8888875769482,-19.4420158954032,-11.1928649299996));
#30816=CARTESIAN_POINT('Ctrl Pts',(22.5933490549502,-19.5764520117207,-10.9625055113849));
#30817=CARTESIAN_POINT('Ctrl Pts',(22.8513437851798,-19.6238525927721,-10.8796937171905));
#30818=CARTESIAN_POINT('Ctrl Pts',(23.3805933886565,-19.7139851739533,-10.7182299385361));
#30819=CARTESIAN_POINT('Ctrl Pts',(23.9182257576784,-19.7948254980796,-10.5680285062335));
#30820=CARTESIAN_POINT('Ctrl Pts',(24.4662138806867,-19.8668205194741,-10.4315004891655));
#30821=CARTESIAN_POINT('Ctrl Pts',(25.0195744741821,-19.9326328666884,-10.3055778221167));
#30822=CARTESIAN_POINT('Ctrl Pts',(25.4412458088222,-19.9749776253081,-10.2242864909386));
#30823=CARTESIAN_POINT('Ctrl Pts',(25.9971983460992,-20.0240850656221,-10.1317971075869));
#30824=CARTESIAN_POINT('Ctrl Pts',(27.1157050405651,-20.102368552767,-9.98182332250459));
#30825=CARTESIAN_POINT('Ctrl Pts',(28.1723100127449,-20.1222437541334,-9.93573708068021));
#30826=CARTESIAN_POINT('Ctrl Pts',(29.0876106506765,-20.1449463132816,-9.89029022572782));
#30827=CARTESIAN_POINT('Ctrl Pts',(29.4537207931442,-20.1517438988728,-9.87684873205161));
#30828=CARTESIAN_POINT('Ctrl Pts',(30.1552759232945,-20.1576060163182,-9.86516345924734));
#30829=CARTESIAN_POINT('Ctrl Pts',(31.3689241276359,-20.1538463873916,-9.87263514017789));
#30830=CARTESIAN_POINT('Ctrl Pts',(32.359478715431,-20.1416711708076,-9.8970230216562));
#30831=CARTESIAN_POINT('Ctrl Pts',(33.1581760188913,-20.1416983285704,-9.89696607979063));
#30832=CARTESIAN_POINT('Ctrl Pts',(33.4913102145728,-20.141699805843,-9.89696201382191));
#30833=CARTESIAN_POINT('Ctrl Pts',(34.1477617736106,-20.1417043298969,-9.8969519305241));
#30834=CARTESIAN_POINT('Ctrl Pts',(34.9726616332632,-20.1417171222834,-9.8969221857378));
#30835=CARTESIAN_POINT('Ctrl Pts',(35.9599657908141,-20.1417226604566,-9.8969094863839));
#30836=CARTESIAN_POINT('Ctrl Pts',(37.9357298104642,-20.1417300151411,-9.89689244880614));
#30837=CARTESIAN_POINT('Ctrl Pts',(39.5833333333333,-20.1417681573542,-9.8968044600346));
#30838=CARTESIAN_POINT('Ctrl Pts',(40.9,-20.1417681573542,-9.8968044600346));
#30839=CARTESIAN_POINT('Ctrl Pts',(6.40644620858992,-12.3446157076951,-27.7818319413302));
#30840=CARTESIAN_POINT('Ctrl Pts',(6.49686818484384,-12.4976194141968,-27.7146057723315));
#30841=CARTESIAN_POINT('Ctrl Pts',(6.58771883172007,-12.6497754970257,-27.6462615383487));
#30842=CARTESIAN_POINT('Ctrl Pts',(7.64885870107047,-14.4089312086777,-26.838967465877));
#30843=CARTESIAN_POINT('Ctrl Pts',(8.64786699401838,-15.9309901815184,-25.9406999974137));
#30844=CARTESIAN_POINT('Ctrl Pts',(10.7071344443812,-18.5841088194585,-24.1258468463739));
#30845=CARTESIAN_POINT('Ctrl Pts',(11.7059636153276,-19.7351568023896,-23.1640388241121));
#30846=CARTESIAN_POINT('Ctrl Pts',(13.7894167134297,-21.7274097031724,-21.32755345859));
#30847=CARTESIAN_POINT('Ctrl Pts',(14.7964804448639,-22.5625068415353,-20.4089660621499));
#30848=CARTESIAN_POINT('Ctrl Pts',(16.9150096963281,-23.9923642448818,-18.7347867871849));
#30849=CARTESIAN_POINT('Ctrl Pts',(17.9356563974909,-24.568778311437,-17.9376031564435));
#30850=CARTESIAN_POINT('Ctrl Pts',(19.3316378726113,-25.1942531765858,-17.0495061236354));
#30851=CARTESIAN_POINT('Ctrl Pts',(19.8373783148987,-25.4080883980548,-16.733671277521));
#30852=CARTESIAN_POINT('Ctrl Pts',(20.898614645132,-25.8097110946141,-16.1088561234904));
#30853=CARTESIAN_POINT('Ctrl Pts',(21.7322089233614,-26.069558105635,-15.6790344990821));
#30854=CARTESIAN_POINT('Ctrl Pts',(22.4452152218926,-26.2607608176431,-15.3644450466694));
#30855=CARTESIAN_POINT('Ctrl Pts',(22.7053175952386,-26.327863353572,-15.2520352575854));
#30856=CARTESIAN_POINT('Ctrl Pts',(23.2405350109147,-26.4560495577168,-15.0319031635371));
#30857=CARTESIAN_POINT('Ctrl Pts',(23.7856351879594,-26.5714803865858,-14.8265027181048));
#30858=CARTESIAN_POINT('Ctrl Pts',(24.3434088150881,-26.6748081507041,-14.6389049166986));
#30859=CARTESIAN_POINT('Ctrl Pts',(24.9080926446007,-26.7695587595052,-14.4653482504621));
#30860=CARTESIAN_POINT('Ctrl Pts',(25.3404979553363,-26.8308622015487,-14.3526452692475));
#30861=CARTESIAN_POINT('Ctrl Pts',(25.9125607075503,-26.9021372597286,-14.2239063651395));
#30862=CARTESIAN_POINT('Ctrl Pts',(27.0720378258712,-27.0165941086124,-14.0136986134134));
#30863=CARTESIAN_POINT('Ctrl Pts',(28.1454151442858,-27.0445191043407,-13.9518646781024));
#30864=CARTESIAN_POINT('Ctrl Pts',(29.0596751952943,-27.0764264216484,-13.890725520751));
#30865=CARTESIAN_POINT('Ctrl Pts',(29.4376599373187,-27.0863532011148,-13.8719255145711));
#30866=CARTESIAN_POINT('Ctrl Pts',(30.1519376760717,-27.0947220176403,-13.855954576287));
#30867=CARTESIAN_POINT('Ctrl Pts',(31.3821999577688,-27.0893514143296,-13.8661782937676));
#30868=CARTESIAN_POINT('Ctrl Pts',(32.3688386893656,-27.0723527225426,-13.898788121758));
#30869=CARTESIAN_POINT('Ctrl Pts',(33.1558986739573,-27.0724155351931,-13.8986675947835));
#30870=CARTESIAN_POINT('Ctrl Pts',(33.4904503866599,-27.0724198047059,-13.8986584195583));
#30871=CARTESIAN_POINT('Ctrl Pts',(34.1462287076183,-27.0724307945235,-13.8986367255002));
#30872=CARTESIAN_POINT('Ctrl Pts',(34.9718350023127,-27.0724629552155,-13.898572048806));
#30873=CARTESIAN_POINT('Ctrl Pts',(35.9590682028414,-27.07247672176,-13.8985445297567));
#30874=CARTESIAN_POINT('Ctrl Pts',(37.9351039480424,-27.0724951558979,-13.8985075170898));
#30875=CARTESIAN_POINT('Ctrl Pts',(39.5833333333333,-27.0725904316243,-13.8983165657899));
#30876=CARTESIAN_POINT('Ctrl Pts',(40.9,-27.0725904316243,-13.8983165657899));
#30877=CARTESIAN_POINT('Ctrl Pts',(6.37427268165564,-14.0406695266741,-32.0290848932163));
#30878=CARTESIAN_POINT('Ctrl Pts',(6.46448755772839,-14.2166050753401,-31.9528098065586));
#30879=CARTESIAN_POINT('Ctrl Pts',(6.55512327887566,-14.3915605358513,-31.8752581000468));
#30880=CARTESIAN_POINT('Ctrl Pts',(7.61410360785655,-16.4151695040825,-30.958672886913));
#30881=CARTESIAN_POINT('Ctrl Pts',(8.61142775869687,-18.1677152487792,-29.9361952854453));
#30882=CARTESIAN_POINT('Ctrl Pts',(10.6634825022472,-21.2183968262284,-27.8730682250753));
#30883=CARTESIAN_POINT('Ctrl Pts',(11.6607542873627,-22.5462154536683,-26.7761583709751));
#30884=CARTESIAN_POINT('Ctrl Pts',(13.7353039743977,-24.8383185913233,-24.6873364683673));
#30885=CARTESIAN_POINT('Ctrl Pts',(14.7402095633116,-25.8029859119439,-23.6392130729629));
#30886=CARTESIAN_POINT('Ctrl Pts',(16.8490881066137,-27.4503074906309,-21.733995182915));
#30887=CARTESIAN_POINT('Ctrl Pts',(17.8672038783314,-28.117536242687,-20.8239061433235));
#30888=CARTESIAN_POINT('Ctrl Pts',(19.2585933984996,-28.8404836901117,-19.811022849419));
#30889=CARTESIAN_POINT('Ctrl Pts',(19.7636418533907,-29.0884650342025,-19.4499572035579));
#30890=CARTESIAN_POINT('Ctrl Pts',(20.8231816497994,-29.5540603372583,-18.7357747989967));
#30891=CARTESIAN_POINT('Ctrl Pts',(21.6568670511734,-29.8562628482712,-18.2431916560479));
#30892=CARTESIAN_POINT('Ctrl Pts',(22.3720072062876,-30.079259337671,-17.8815051531587));
#30893=CARTESIAN_POINT('Ctrl Pts',(22.6326824787812,-30.1574913312726,-17.7523977438431));
#30894=CARTESIAN_POINT('Ctrl Pts',(23.1697036949936,-30.3071564102285,-17.4991937768335));
#30895=CARTESIAN_POINT('Ctrl Pts',(23.7174377716561,-30.4422233412818,-17.2625030946595));
#30896=CARTESIAN_POINT('Ctrl Pts',(24.2790946262572,-30.5634410393028,-17.0457855087881));
#30897=CARTESIAN_POINT('Ctrl Pts',(24.8485847331463,-30.6748008187178,-16.8449230908939));
#30898=CARTESIAN_POINT('Ctrl Pts',(25.2859632686136,-30.7471152582868,-16.7140007344129));
#30899=CARTESIAN_POINT('Ctrl Pts',(25.8659001690754,-30.8313513860032,-16.5640760155963));
#30900=CARTESIAN_POINT('Ctrl Pts',(27.0467877055031,-30.9672841404843,-16.3181083484214));
#30901=CARTESIAN_POINT('Ctrl Pts',(28.1301993946288,-30.9999203594232,-16.2470842981322));
#30902=CARTESIAN_POINT('Ctrl Pts',(29.0438132065911,-31.0370949113971,-16.1769735529555));
#30903=CARTESIAN_POINT('Ctrl Pts',(29.4285323170642,-31.0489002942268,-16.1549555741443));
#30904=CARTESIAN_POINT('Ctrl Pts',(30.1500796604944,-31.0587367393327,-16.1364761766635));
#30905=CARTESIAN_POINT('Ctrl Pts',(31.3898224001987,-31.0524272220083,-16.1483068856791));
#30906=CARTESIAN_POINT('Ctrl Pts',(32.3742147772172,-31.032701705164,-16.1855693458549));
#30907=CARTESIAN_POINT('Ctrl Pts',(33.1546196294425,-31.0327939306213,-16.1853991323254));
#30908=CARTESIAN_POINT('Ctrl Pts',(33.4899805045661,-31.0328008093451,-16.1853856345319));
#30909=CARTESIAN_POINT('Ctrl Pts',(34.1453728987308,-31.0328173216773,-16.1853546639145));
#30910=CARTESIAN_POINT('Ctrl Pts',(34.9713787068035,-31.0328663827335,-16.1852616946182));
#30911=CARTESIAN_POINT('Ctrl Pts',(35.9585696612046,-31.0328872804502,-16.1852222245756));
#30912=CARTESIAN_POINT('Ctrl Pts',(37.9347583211501,-31.0329153648958,-16.1851690519236));
#30913=CARTESIAN_POINT('Ctrl Pts',(39.5833333333333,-31.0330603026358,-16.1848949119358));
#30914=CARTESIAN_POINT('Ctrl Pts',(40.9,-31.0330603026358,-16.1848949119358));
#30915=CARTESIAN_POINT('',(40.9,-29.2992994660114,-15.1839076262003));
#30916=CARTESIAN_POINT('Ctrl Pts',(40.9,-29.2992994660114,-15.1839076262003));
#30917=CARTESIAN_POINT('Ctrl Pts',(40.9,-29.7327406817405,-15.4341550287793));
#30918=CARTESIAN_POINT('Ctrl Pts',(40.9,-30.1661818974696,-15.6844024313584));
#30919=CARTESIAN_POINT('Ctrl Pts',(40.9,-30.5996231131986,-15.9346498339374));
#30920=CARTESIAN_POINT('',(38.,-29.2992994660114,-15.1839076262003));
#30921=CARTESIAN_POINT('Ctrl Pts',(38.,-29.2992994660114,-15.1839076262003));
#30922=CARTESIAN_POINT('Ctrl Pts',(38.9666666666667,-29.2992994660114,-15.1839076262003));
#30923=CARTESIAN_POINT('Ctrl Pts',(39.9333333333333,-29.2992994660114,-15.1839076262003));
#30924=CARTESIAN_POINT('Ctrl Pts',(40.9,-29.2992994660114,-15.1839076262003));
#30925=CARTESIAN_POINT('Ctrl Pts',(37.4974382384971,-28.7790269720418,-14.8838038109906));
#30926=CARTESIAN_POINT('Ctrl Pts',(37.6645213547145,-28.9527098777879,-14.9840691120819));
#30927=CARTESIAN_POINT('Ctrl Pts',(37.8313739960415,-29.1261374112004,-15.084184715056));
#30928=CARTESIAN_POINT('Ctrl Pts',(37.9978889629902,-29.2992044501374,-15.1840905833949));
#30929=CARTESIAN_POINT('',(6.9,-12.9951291628659,-27.0393531365015));
#30930=CARTESIAN_POINT('Ctrl Pts',(6.9,-12.9951291628659,-27.0393531365015));
#30931=CARTESIAN_POINT('Ctrl Pts',(6.9,-11.9174419758914,-24.649274247254));
#30932=CARTESIAN_POINT('Ctrl Pts',(6.90000000000115,-10.8339866674746,-22.230729924082));
#30933=CARTESIAN_POINT('Ctrl Pts',(6.90000000000115,-8.41000082059024,-16.7584145047598));
#30934=CARTESIAN_POINT('Ctrl Pts',(6.9,-6.82522008706163,-13.1312177506378));
#30935=CARTESIAN_POINT('Ctrl Pts',(6.9,-5.36789542693312,-9.63452070648529));
#30936=CARTESIAN_POINT('',(22.9245129145126,-27.5141512254857,-15.8853026165582));
#30937=CARTESIAN_POINT('Ctrl Pts',(22.9245129145126,-27.5141512254857,-15.8853026165582));
#30938=CARTESIAN_POINT('Ctrl Pts',(22.7202811020963,-27.405303612937,-15.9355315703924));
#30939=CARTESIAN_POINT('Ctrl Pts',(22.5089075447093,-27.2924652433825,-15.9922246435191));
#30940=CARTESIAN_POINT('Ctrl Pts',(22.2913349439917,-27.1762359097413,-16.0558281873747));
#30941=CARTESIAN_POINT('Ctrl Pts',(21.4451770585291,-26.7242103933931,-16.3031876434795));
#30942=CARTESIAN_POINT('Ctrl Pts',(20.5220951556666,-26.2108400614941,-16.6965145338606));
#30943=CARTESIAN_POINT('Ctrl Pts',(19.7671428819536,-25.7770859372677,-17.0753616782145));
#30944=CARTESIAN_POINT('Ctrl Pts',(19.519477305839,-25.6347908958338,-17.1996442316061));
#30945=CARTESIAN_POINT('Ctrl Pts',(19.286571638609,-25.4994131575072,-17.3225345039427));
#30946=CARTESIAN_POINT('Ctrl Pts',(19.0728538401323,-25.3740784559106,-17.4387046858284));
#30947=CARTESIAN_POINT('Ctrl Pts',(18.7028555998035,-25.15709316328,-17.6398239336529));
#30948=CARTESIAN_POINT('Ctrl Pts',(18.4144703596235,-24.9815167506411,-17.8106758656205));
#30949=CARTESIAN_POINT('Ctrl Pts',(18.0642874871537,-24.7606238748751,-18.0298340093775));
#30950=CARTESIAN_POINT('Ctrl Pts',(17.442092711672,-24.3681478172274,-18.4192278454841));
#30951=CARTESIAN_POINT('Ctrl Pts',(16.7224564418218,-23.8866996305775,-18.9163953124275));
#30952=CARTESIAN_POINT('Ctrl Pts',(15.9202806616111,-23.2999769887242,-19.5075155171573));
#30953=CARTESIAN_POINT('Ctrl Pts',(15.4090529834512,-22.9260578785765,-19.8842371999013));
#30954=CARTESIAN_POINT('Ctrl Pts',(14.8739602945702,-22.5035099772286,-20.3065653819892));
#30955=CARTESIAN_POINT('Ctrl Pts',(14.3169794331135,-22.0244589523024,-20.7640450546201));
#30956=CARTESIAN_POINT('Ctrl Pts',(13.8864206762823,-21.6541417151688,-21.1176871503438));
#30957=CARTESIAN_POINT('Ctrl Pts',(13.3867890027795,-21.2019814327435,-21.5394320189433));
#30958=CARTESIAN_POINT('Ctrl Pts',(12.8146824059514,-20.6456427149589,-22.0238946695559));
#30959=CARTESIAN_POINT('Ctrl Pts',(12.2526665517595,-20.0991166279862,-22.499812430193));
#30960=CARTESIAN_POINT('Ctrl Pts',(11.6379478462803,-19.44703563439,-23.0419154065947));
#30961=CARTESIAN_POINT('Ctrl Pts',(10.9739250490308,-18.6689137476991,-23.626535453056));
#30962=CARTESIAN_POINT('Ctrl Pts',(10.5683455447963,-18.1936434853748,-23.9836164291783));
#30963=CARTESIAN_POINT('Ctrl Pts',(10.1437415406956,-17.6694303965612,-24.3558958755273));
#30964=CARTESIAN_POINT('Ctrl Pts',(9.74137929176525,-17.1528053766524,-24.6998029803349));
#30965=CARTESIAN_POINT('Ctrl Pts',(8.72285779294234,-15.8450442956717,-25.5703537856744));
#30966=CARTESIAN_POINT('Ctrl Pts',(7.81323138778195,-14.4751178145146,-26.3485431508901));
#30967=CARTESIAN_POINT('Ctrl Pts',(6.9,-12.9951291628659,-27.0393531365015));
#30968=CARTESIAN_POINT('Ctrl Pts',(30.5,-31.0562879796886,-16.1402285275843));
#30969=CARTESIAN_POINT('Ctrl Pts',(29.9560179420817,-30.8470467059701,-16.0158030554221));
#30970=CARTESIAN_POINT('Ctrl Pts',(29.4152668325132,-30.6299015220344,-15.9055856438303));
#30971=CARTESIAN_POINT('Ctrl Pts',(28.8740459957565,-30.3967092920472,-15.8236145009996));
#30972=CARTESIAN_POINT('Ctrl Pts',(28.353527792344,-30.1724370682909,-15.7447788961961));
#30973=CARTESIAN_POINT('Ctrl Pts',(27.8179515912467,-29.9423746730404,-15.6599939665101));
#30974=CARTESIAN_POINT('Ctrl Pts',(27.2695051149491,-29.6962958928787,-15.5981844167478));
#30975=CARTESIAN_POINT('Ctrl Pts',(26.9554553615883,-29.5553870101399,-15.5627912203338));
#30976=CARTESIAN_POINT('Ctrl Pts',(26.6378099296971,-29.4095747645068,-15.5350208970661));
#30977=CARTESIAN_POINT('Ctrl Pts',(26.3179304017917,-29.2578762499931,-15.520523503095));
#30978=CARTESIAN_POINT('Ctrl Pts',(26.1078196745982,-29.1582340959379,-15.5110009868852));
#30979=CARTESIAN_POINT('Ctrl Pts',(25.8967402232745,-29.0560612282453,-15.5072071790431));
#30980=CARTESIAN_POINT('Ctrl Pts',(25.6850706236774,-28.9510881944939,-15.5107635234098));
#30981=CARTESIAN_POINT('Ctrl Pts',(25.6562210027417,-28.9367808388889,-15.5112482372614));
#30982=CARTESIAN_POINT('Ctrl Pts',(25.6277737638215,-28.9226278510966,-15.5118582602787));
#30983=CARTESIAN_POINT('Ctrl Pts',(25.5983858063598,-28.9079571471847,-15.5126342200129));
#30984=CARTESIAN_POINT('Ctrl Pts',(25.1249357452756,-28.6716070819486,-15.5251351971226));
#30985=CARTESIAN_POINT('Ctrl Pts',(24.1510084067019,-28.1678256190434,-15.5836572228941));
#30986=CARTESIAN_POINT('Ctrl Pts',(22.9245129145126,-27.5141512254857,-15.8853026165582));
#30987=CARTESIAN_POINT('Origin',(40.65,0.,0.));
#30988=CARTESIAN_POINT('',(40.4,-16.1848830792292,-31.0330398077868));
#30989=CARTESIAN_POINT('',(40.9,-15.9346498339374,-30.5996231131986));
#30990=CARTESIAN_POINT('Ctrl Pts',(40.4,-16.1848830792292,-31.0330398077868));
#30991=CARTESIAN_POINT('Ctrl Pts',(40.5666590138495,-16.1014769396247,-30.8885761363286));
#30992=CARTESIAN_POINT('Ctrl Pts',(40.7333430451341,-16.0180571835863,-30.744088880515));
#30993=CARTESIAN_POINT('Ctrl Pts',(40.9,-15.9346498339374,-30.5996231131986));
#30994=CARTESIAN_POINT('',(40.9,-18.5327260452908,-29.0996231131986));
#30995=CARTESIAN_POINT('Origin',(40.9,0.,0.));
#30996=CARTESIAN_POINT('',(40.4,-18.7829592905825,-29.5330398077868));
#30997=CARTESIAN_POINT('Ctrl Pts',(40.9,-18.5327260452908,-29.0996231131986));
#30998=CARTESIAN_POINT('Ctrl Pts',(40.7333430447101,-18.6161333951518,-29.2440888808826));
#30999=CARTESIAN_POINT('Ctrl Pts',(40.5666590132533,-18.6995531512764,-29.3885761368453));
#31000=CARTESIAN_POINT('Ctrl Pts',(40.4,-18.7829592905825,-29.5330398077868));
#31001=CARTESIAN_POINT('Origin',(40.4,0.,0.));
#31002=CARTESIAN_POINT('Origin',(35.7,0.,0.));
#31003=CARTESIAN_POINT('',(30.5,-18.8254200738635,-29.5059919176187));
#31004=CARTESIAN_POINT('Ctrl Pts',(40.3998805977105,-18.782947901926,-29.5330468723878));
#31005=CARTESIAN_POINT('Ctrl Pts',(39.2493532038275,-18.7828975281295,-29.5330781201994));
#31006=CARTESIAN_POINT('Ctrl Pts',(38.0972325173599,-18.7826942098824,-29.5332042421555));
#31007=CARTESIAN_POINT('Ctrl Pts',(36.9466403234098,-18.782625610211,-29.5332467931397));
#31008=CARTESIAN_POINT('Ctrl Pts',(36.745394297411,-18.7826136116842,-29.5332542355824));
#31009=CARTESIAN_POINT('Ctrl Pts',(36.5441950314761,-18.7826057345052,-29.5332591213989));
#31010=CARTESIAN_POINT('Ctrl Pts',(36.3429831482489,-18.7825981392881,-29.5332638326403));
#31011=CARTESIAN_POINT('Ctrl Pts',(36.2103627229667,-18.7825931332173,-29.5332669378586));
#31012=CARTESIAN_POINT('Ctrl Pts',(36.0823539051257,-18.7825884046849,-29.5332699079689));
#31013=CARTESIAN_POINT('Ctrl Pts',(35.9587472612939,-18.7825830316391,-29.5332733040083));
#31014=CARTESIAN_POINT('Ctrl Pts',(35.7554552091584,-18.7825741947555,-29.5332788893701));
#31015=CARTESIAN_POINT('Ctrl Pts',(35.5640774639622,-18.7825638026986,-29.5332855100023));
#31016=CARTESIAN_POINT('Ctrl Pts',(35.3838244596856,-18.782553672802,-29.5332919882553));
#31017=CARTESIAN_POINT('Ctrl Pts',(35.2391029657229,-18.7825455397126,-29.5332971895137));
#31018=CARTESIAN_POINT('Ctrl Pts',(35.1015509582127,-18.7825375448577,-29.5333023181014));
#31019=CARTESIAN_POINT('Ctrl Pts',(34.9707359993668,-18.7825301857251,-29.53330703978));
#31020=CARTESIAN_POINT('Ctrl Pts',(34.8578981782314,-18.7825238379151,-29.5333111125858));
#31021=CARTESIAN_POINT('Ctrl Pts',(34.7500670454672,-18.7825179390022,-29.5333148977088));
#31022=CARTESIAN_POINT('Ctrl Pts',(34.6468496336297,-18.782512339199,-29.5333184739616));
#31023=CARTESIAN_POINT('Ctrl Pts',(34.5887227637969,-18.7825091856706,-29.5333204879278));
#31024=CARTESIAN_POINT('Ctrl Pts',(34.5320601650633,-18.7825061280823,-29.5333224349598));
#31025=CARTESIAN_POINT('Ctrl Pts',(34.4767987085459,-18.7825031467929,-29.5333243245742));
#31026=CARTESIAN_POINT('Ctrl Pts',(34.3959515551434,-18.7824987851858,-29.5333270890679));
#31027=CARTESIAN_POINT('Ctrl Pts',(34.3181086379454,-18.7824945796072,-29.533329735068));
#31028=CARTESIAN_POINT('Ctrl Pts',(34.2432236356786,-18.7824903289018,-29.5333323757534));
#31029=CARTESIAN_POINT('Ctrl Pts',(34.1622675304678,-18.7824857335818,-29.5333352305253));
#31030=CARTESIAN_POINT('Ctrl Pts',(34.0847679660331,-18.7824810863437,-29.5333380785848));
#31031=CARTESIAN_POINT('Ctrl Pts',(34.0106064145705,-18.7824762391415,-29.533340998409));
#31032=CARTESIAN_POINT('Ctrl Pts',(34.0011740964187,-18.7824756226448,-29.53334136977));
#31033=CARTESIAN_POINT('Ctrl Pts',(33.9917957065823,-18.7824750030335,-29.5333417422189));
#31034=CARTESIAN_POINT('Ctrl Pts',(33.9824709442606,-18.7824743801028,-29.5333421158564));
#31035=CARTESIAN_POINT('Ctrl Pts',(33.9223617768599,-18.7824703645751,-29.533344524394));
#31036=CARTESIAN_POINT('Ctrl Pts',(33.8644761964478,-18.7824662176988,-29.5333469783448));
#31037=CARTESIAN_POINT('Ctrl Pts',(33.8085662292047,-18.7824621301166,-29.5333493560321));
#31038=CARTESIAN_POINT('Ctrl Pts',(33.7474237016288,-18.7824576599816,-29.533351956245));
#31039=CARTESIAN_POINT('Ctrl Pts',(33.6886441629994,-18.782453260435,-29.5333544654464));
#31040=CARTESIAN_POINT('Ctrl Pts',(33.6319696815835,-18.7824490897764,-29.5333567795391));
#31041=CARTESIAN_POINT('Ctrl Pts',(33.5826925637836,-18.7824454634877,-29.5333587915877));
#31042=CARTESIAN_POINT('Ctrl Pts',(33.5350083429209,-18.7824420082021,-29.5333606573655));
#31043=CARTESIAN_POINT('Ctrl Pts',(33.4887791610839,-18.7824387840041,-29.5333623350385));
#31044=CARTESIAN_POINT('Ctrl Pts',(33.4518540160536,-18.7824362087048,-29.5333636750648));
#31045=CARTESIAN_POINT('Ctrl Pts',(33.4158630419527,-18.7824337707087,-29.5333649012377));
#31046=CARTESIAN_POINT('Ctrl Pts',(33.3809178974527,-18.7824311830501,-29.5333661853037));
#31047=CARTESIAN_POINT('Ctrl Pts',(33.3430135142412,-18.7824283762623,-29.5333675781075));
#31048=CARTESIAN_POINT('Ctrl Pts',(33.3063394414416,-18.7824253936822,-29.5333690388471));
#31049=CARTESIAN_POINT('Ctrl Pts',(33.2709744550635,-18.7824219844966,-29.5333707164935));
#31050=CARTESIAN_POINT('Ctrl Pts',(33.2337091834356,-18.7824183921235,-29.5333724842856));
#31051=CARTESIAN_POINT('Ctrl Pts',(33.1978968817727,-18.7824143271502,-29.5333744922618));
#31052=CARTESIAN_POINT('Ctrl Pts',(33.1635680440812,-18.7824096073364,-29.5333768470679));
#31053=CARTESIAN_POINT('Ctrl Pts',(33.125851795334,-18.7824044217933,-29.5333794342353));
#31054=CARTESIAN_POINT('Ctrl Pts',(33.0899258347182,-18.7823984465448,-29.5333824396031));
#31055=CARTESIAN_POINT('Ctrl Pts',(33.0557653925381,-18.7823915567442,-29.5333859335397));
#31056=CARTESIAN_POINT('Ctrl Pts',(33.0368719877466,-18.7823877461438,-29.5333878659608));
#31057=CARTESIAN_POINT('Ctrl Pts',(33.0185175727353,-18.7823836577058,-29.5333899466652));
#31058=CARTESIAN_POINT('Ctrl Pts',(33.0006913489163,-18.7823792820484,-29.5333921804186));
#31059=CARTESIAN_POINT('Ctrl Pts',(32.9433364918128,-18.7823652036207,-29.5333993673924));
#31060=CARTESIAN_POINT('Ctrl Pts',(32.889323201888,-18.78254762761,-29.5332829792212));
#31061=CARTESIAN_POINT('Ctrl Pts',(32.8382230276384,-18.7828441879673,-29.5330947066102));
#31062=CARTESIAN_POINT('Ctrl Pts',(32.7810653124613,-18.7831759033222,-29.5328841156987));
#31063=CARTESIAN_POINT('Ctrl Pts',(32.727552456734,-18.7836507315896,-29.5325833908465));
#31064=CARTESIAN_POINT('Ctrl Pts',(32.6770430180203,-18.7841988326963,-29.532236338609));
#31065=CARTESIAN_POINT('Ctrl Pts',(32.6227203152382,-18.7847883132819,-29.5318630852917));
#31066=CARTESIAN_POINT('Ctrl Pts',(32.5718714572479,-18.785463223046,-29.5314358211882));
#31067=CARTESIAN_POINT('Ctrl Pts',(32.5236533105896,-18.7861776883228,-29.5309832901274));
#31068=CARTESIAN_POINT('Ctrl Pts',(32.4718100172051,-18.7869458686765,-29.5304967367823));
#31069=CARTESIAN_POINT('Ctrl Pts',(32.4230076638009,-18.7877604440451,-29.5299805544879));
#31070=CARTESIAN_POINT('Ctrl Pts',(32.3761512173999,-18.7885990068259,-29.5294487410664));
#31071=CARTESIAN_POINT('Ctrl Pts',(32.3248096593241,-18.789517837062,-29.5288660223209));
#31072=CARTESIAN_POINT('Ctrl Pts',(32.2758043952268,-18.7904660501636,-29.5282641699575));
#31073=CARTESIAN_POINT('Ctrl Pts',(32.2276418902244,-18.7914438969209,-29.5276429421487));
#31074=CARTESIAN_POINT('Ctrl Pts',(32.1780484881789,-18.7924507952825,-29.5270032578033));
#31075=CARTESIAN_POINT('Ctrl Pts',(32.129348520974,-18.7934898292201,-29.5263425802702));
#31076=CARTESIAN_POINT('Ctrl Pts',(32.0798596724228,-18.7945806304077,-29.525648507911));
#31077=CARTESIAN_POINT('Ctrl Pts',(32.031031972984,-18.7956568589742,-29.5249637080513));
#31078=CARTESIAN_POINT('Ctrl Pts',(31.9814363681891,-18.7967841298918,-29.5242459916461));
#31079=CARTESIAN_POINT('Ctrl Pts',(31.9294088358078,-18.7979897030586,-29.5234781935338));
#31080=CARTESIAN_POINT('Ctrl Pts',(31.898016936455,-18.7987171108326,-29.523014926491));
#31081=CARTESIAN_POINT('Ctrl Pts',(31.8657387727398,-18.7994731540541,-29.5225333463335));
#31082=CARTESIAN_POINT('Ctrl Pts',(31.8321995512669,-18.8002637764333,-29.5220297160307));
#31083=CARTESIAN_POINT('Ctrl Pts',(31.7313430764712,-18.8026412730644,-29.5205152391074));
#31084=CARTESIAN_POINT('Ctrl Pts',(31.6280303047182,-18.8051208626313,-29.5189339807854));
#31085=CARTESIAN_POINT('Ctrl Pts',(31.5230436279567,-18.8075570028383,-29.5173797885034));
#31086=CARTESIAN_POINT('Ctrl Pts',(31.4165412786074,-18.8100283131358,-29.5158031586445));
#31087=CARTESIAN_POINT('Ctrl Pts',(31.308316172914,-18.8124535008248,-29.5142552682412));
#31088=CARTESIAN_POINT('Ctrl Pts',(31.1992361814705,-18.8146708543332,-29.512840201736));
#31089=CARTESIAN_POINT('Ctrl Pts',(31.1417800745714,-18.8158388091388,-29.5120948385276));
#31090=CARTESIAN_POINT('Ctrl Pts',(31.0840876480106,-18.8169490689289,-29.5113863465313));
#31091=CARTESIAN_POINT('Ctrl Pts',(31.0262914639723,-18.8179790482416,-29.5107292749179));
#31092=CARTESIAN_POINT('Ctrl Pts',(30.9238422544137,-18.8198047841132,-29.5095645532577));
#31093=CARTESIAN_POINT('Ctrl Pts',(30.8210652532058,-18.8213763539421,-29.5085625948816));
#31094=CARTESIAN_POINT('Ctrl Pts',(30.718765507456,-18.8225556950176,-29.507810834769));
#31095=CARTESIAN_POINT('Ctrl Pts',(30.6466529343875,-18.82338702963,-29.5072809081729));
#31096=CARTESIAN_POINT('Ctrl Pts',(30.5747782907563,-18.8240238717387,-29.5068750504575));
#31097=CARTESIAN_POINT('Ctrl Pts',(30.503432395139,-18.8244289981692,-29.5066169468345));
#31098=CARTESIAN_POINT('Ctrl Pts',(30.5006731185507,-18.8244446662867,-29.5066069647707));
#31099=CARTESIAN_POINT('Ctrl Pts',(30.497914633606,-18.8244599892394,-29.5065972028237));
#31100=CARTESIAN_POINT('Ctrl Pts',(30.4951569527683,-18.8244749650172,-29.5065876622664));
#31101=CARTESIAN_POINT('',(30.5,-16.229443021655,-31.0097594187194));
#31102=CARTESIAN_POINT('Origin',(30.5,0.,0.));
#31103=CARTESIAN_POINT('Ctrl Pts',(30.5049076308141,-16.2304573503026,-31.0091238687319));
#31104=CARTESIAN_POINT('Ctrl Pts',(30.5973062294345,-16.2298682766552,-31.0094328533548));
#31105=CARTESIAN_POINT('Ctrl Pts',(30.689059158586,-16.2288427503286,-31.0099692677028));
#31106=CARTESIAN_POINT('Ctrl Pts',(30.7806364364919,-16.2274919709621,-31.0106763092384));
#31107=CARTESIAN_POINT('Ctrl Pts',(30.8441456090292,-16.2265552005994,-31.0111666450936));
#31108=CARTESIAN_POINT('Ctrl Pts',(30.9075713010184,-16.2254611740684,-31.0117394593184));
#31109=CARTESIAN_POINT('Ctrl Pts',(30.9710816356704,-16.2242390174924,-31.0123798375508));
#31110=CARTESIAN_POINT('Ctrl Pts',(31.0734991469995,-16.2222681534488,-31.0134125190071));
#31111=CARTESIAN_POINT('Ctrl Pts',(31.1761345288068,-16.2199648111636,-31.0146205155167));
#31112=CARTESIAN_POINT('Ctrl Pts',(31.279810056847,-16.2174702047238,-31.0159286966544));
#31113=CARTESIAN_POINT('Ctrl Pts',(31.3828326297126,-16.2149913094766,-31.0172286387828));
#31114=CARTESIAN_POINT('Ctrl Pts',(31.4868822244325,-16.2123218973815,-31.0186283615542));
#31115=CARTESIAN_POINT('Ctrl Pts',(31.5928140565585,-16.2095937955791,-31.020057669606));
#31116=CARTESIAN_POINT('Ctrl Pts',(31.6516194621098,-16.208079358137,-31.0208511142011));
#31117=CARTESIAN_POINT('Ctrl Pts',(31.7110057676085,-16.2065468518028,-31.0216536678951));
#31118=CARTESIAN_POINT('Ctrl Pts',(31.7711259776529,-16.2050208141949,-31.0224523036437));
#31119=CARTESIAN_POINT('Ctrl Pts',(31.8409078613427,-16.2032495333099,-31.0233792848848));
#31120=CARTESIAN_POINT('Ctrl Pts',(31.9056298453964,-16.2016434584277,-31.0242198767433));
#31121=CARTESIAN_POINT('Ctrl Pts',(31.9658749467865,-16.2002018139142,-31.0249744961546));
#31122=CARTESIAN_POINT('Ctrl Pts',(32.0341046687228,-16.1985691001829,-31.0258291295008));
#31123=CARTESIAN_POINT('Ctrl Pts',(32.0965918298941,-16.1971462744691,-31.026574015819));
#31124=CARTESIAN_POINT('Ctrl Pts',(32.1542461945013,-16.1959042389539,-31.0272242625029));
#31125=CARTESIAN_POINT('Ctrl Pts',(32.215166595352,-16.1945918439258,-31.0279113447196));
#31126=CARTESIAN_POINT('Ctrl Pts',(32.2706916712563,-16.1934801514051,-31.0284933558527));
#31127=CARTESIAN_POINT('Ctrl Pts',(32.3219582775162,-16.1925241206212,-31.0289937114781));
#31128=CARTESIAN_POINT('Ctrl Pts',(32.3761916324778,-16.1915127652646,-31.0295230221975));
#31129=CARTESIAN_POINT('Ctrl Pts',(32.425659986223,-16.1906748064835,-31.0299613681536));
#31130=CARTESIAN_POINT('Ctrl Pts',(32.4717693483789,-16.1899610544418,-31.0303343957023));
#31131=CARTESIAN_POINT('Ctrl Pts',(32.521533200307,-16.1891907325537,-31.0307369882959));
#31132=CARTESIAN_POINT('Ctrl Pts',(32.5673849287952,-16.1885644631731,-31.0310638203075));
#31133=CARTESIAN_POINT('Ctrl Pts',(32.6111519417719,-16.1880367365758,-31.0313387615313));
#31134=CARTESIAN_POINT('Ctrl Pts',(32.6551741210746,-16.1875059332764,-31.0316153056916));
#31135=CARTESIAN_POINT('Ctrl Pts',(32.697087871783,-16.1870745377529,-31.0318395012595));
#31136=CARTESIAN_POINT('Ctrl Pts',(32.7388013470514,-16.1867185738399,-31.0320241553172));
#31137=CARTESIAN_POINT('Ctrl Pts',(32.7801521457873,-16.1863657048443,-31.0322072039058));
#31138=CARTESIAN_POINT('Ctrl Pts',(32.8213062770012,-16.1860865454659,-31.0323516104906));
#31139=CARTESIAN_POINT('Ctrl Pts',(32.8641640035292,-16.1858844594634,-31.0324560971769));
#31140=CARTESIAN_POINT('Ctrl Pts',(32.9038200784524,-16.1856974701314,-31.0325527782703));
#31141=CARTESIAN_POINT('Ctrl Pts',(32.944934777289,-16.1855761117061,-31.0326154655019));
#31142=CARTESIAN_POINT('Ctrl Pts',(32.9890474705801,-16.1855509840873,-31.0326287580452));
#31143=CARTESIAN_POINT('Ctrl Pts',(32.9926089293361,-16.1855489553974,-31.0326298312248));
#31144=CARTESIAN_POINT('Ctrl Pts',(32.9961899495402,-16.1855475722577,-31.0326305730127));
#31145=CARTESIAN_POINT('Ctrl Pts',(32.9997913521114,-16.1855468609619,-31.0326309700537));
#31146=CARTESIAN_POINT('Ctrl Pts',(33.0362292496771,-16.1855396642873,-31.0326349871946));
#31147=CARTESIAN_POINT('Ctrl Pts',(33.0740922921119,-16.1855331333215,-31.0326386992184));
#31148=CARTESIAN_POINT('Ctrl Pts',(33.114143918563,-16.1855273500631,-31.0326422490868));
#31149=CARTESIAN_POINT('Ctrl Pts',(33.2461674547434,-16.1855082865122,-31.0326539506383));
#31150=CARTESIAN_POINT('Ctrl Pts',(33.3721931286568,-16.1855003220479,-31.0326588963952));
#31151=CARTESIAN_POINT('Ctrl Pts',(33.4993879207448,-16.1854928138549,-31.0326635427516));
#31152=CARTESIAN_POINT('Ctrl Pts',(33.6627849160625,-16.1854831686789,-31.0326695115547));
#31153=CARTESIAN_POINT('Ctrl Pts',(33.8281112474539,-16.1854742764644,-31.0326749862722));
#31154=CARTESIAN_POINT('Ctrl Pts',(33.9929845306743,-16.1854606405093,-31.0326833946004));
#31155=CARTESIAN_POINT('Ctrl Pts',(34.3227310971151,-16.1854333685992,-31.0327002112569));
#31156=CARTESIAN_POINT('Ctrl Pts',(34.6506654708718,-16.1853871217269,-31.032728762356));
#31157=CARTESIAN_POINT('Ctrl Pts',(34.979269363621,-16.1853559472169,-31.032748004237));
#31158=CARTESIAN_POINT('Ctrl Pts',(35.3078732563701,-16.1853247727068,-31.032767246118));
#31159=CARTESIAN_POINT('Ctrl Pts',(35.6371466681116,-16.185308670559,-31.032777178781));
#31160=CARTESIAN_POINT('Ctrl Pts',(35.9662682695208,-16.1852951338216,-31.0327855310262));
#31161=CARTESIAN_POINT('Ctrl Pts',(36.29538987093,-16.1852815970843,-31.0327938832713));
#31162=CARTESIAN_POINT('Ctrl Pts',(36.6243596620069,-16.1852706257574,-31.0328006550988));
#31163=CARTESIAN_POINT('Ctrl Pts',(36.9532592751492,-16.185248102247,-31.0328145551759));
#31164=CARTESIAN_POINT('Ctrl Pts',(38.102326278026,-16.1851694125146,-31.0328631174705));
#31165=CARTESIAN_POINT('Ctrl Pts',(39.2505367075414,-16.184949719878,-31.0329986853002));
#31166=CARTESIAN_POINT('Ctrl Pts',(40.4000986012038,-16.1848953623403,-31.0330322281526));
#31167=CARTESIAN_POINT('Ctrl Pts',(6.89999999997365,0.168526548676475,-11.0276873985587));
#31168=CARTESIAN_POINT('Ctrl Pts',(6.99168932310453,0.107121039164007,-11.0290491215116));
#31169=CARTESIAN_POINT('Ctrl Pts',(7.08383940291242,0.0458098125994604,
-11.0299018391088));
#31170=CARTESIAN_POINT('Ctrl Pts',(8.15761824498006,-0.664186592400577,
-11.0337651740187));
#31171=CARTESIAN_POINT('Ctrl Pts',(9.16607857437499,-1.30870352701556,-10.9699676285446));
#31172=CARTESIAN_POINT('Ctrl Pts',(11.2535171643192,-2.47376106241928,-10.77603305676));
#31173=CARTESIAN_POINT('Ctrl Pts',(12.2576790632369,-3.00237606292525,-10.6330057282434));
#31174=CARTESIAN_POINT('Ctrl Pts',(14.3563663857894,-3.944470058834,-10.3307260661656));
#31175=CARTESIAN_POINT('Ctrl Pts',(15.3658129161116,-4.36032593857961,-10.1540434041659));
#31176=CARTESIAN_POINT('Ctrl Pts',(17.4727193021212,-5.08193366885832,-9.82334300624283));
#31177=CARTESIAN_POINT('Ctrl Pts',(18.4888802671462,-5.39169279079136,-9.6488422591121));
#31178=CARTESIAN_POINT('Ctrl Pts',(19.8473882183426,-5.72385817850078,-9.45778984314827));
#31179=CARTESIAN_POINT('Ctrl Pts',(20.3451395577184,-5.84063156394592,-9.38741838105894));
#31180=CARTESIAN_POINT('Ctrl Pts',(21.119864121141,-6.00690103675049,-9.28201599203951));
#31181=CARTESIAN_POINT('Ctrl Pts',(21.9116430735678,-6.15921075032182,-9.18172875488037));
#31182=CARTESIAN_POINT('Ctrl Pts',(22.4533884343746,-6.25063668203688,-9.12054551137776));
#31183=CARTESIAN_POINT('Ctrl Pts',(22.8546099577479,-6.31320896750581,-9.07881438233611));
#31184=CARTESIAN_POINT('Ctrl Pts',(23.1058218650381,-6.35118260107244,-9.05298395410355));
#31185=CARTESIAN_POINT('Ctrl Pts',(23.6175153199788,-6.42382403760963,-9.00245668094437));
#31186=CARTESIAN_POINT('Ctrl Pts',(24.1364702886545,-6.49007583237977,-8.95485371029554));
#31187=CARTESIAN_POINT('Ctrl Pts',(24.6629181373246,-6.54944423929279,-8.91145225308144));
#31188=CARTESIAN_POINT('Ctrl Pts',(25.0606678571037,-6.59024788291775,-8.88140293076164));
#31189=CARTESIAN_POINT('Ctrl Pts',(25.3945416155882,-6.62099228309709,-8.85873533710263));
#31190=CARTESIAN_POINT('Ctrl Pts',(25.6627586119464,-6.64352323130153,-8.84221409068032));
#31191=CARTESIAN_POINT('Ctrl Pts',(25.7972076165425,-6.65408072739386,-8.83452216013014));
#31192=CARTESIAN_POINT('Ctrl Pts',(26.3824137782946,-6.69837697633853,-8.80240169886323));
#31193=CARTESIAN_POINT('Ctrl Pts',(27.4369717967155,-6.74704662082202,-8.76563881905853));
#31194=CARTESIAN_POINT('Ctrl Pts',(28.4593635146677,-6.76713562537254,-8.74917816753949));
#31195=CARTESIAN_POINT('Ctrl Pts',(29.0427481469891,-6.77974505298722,-8.73952198264543));
#31196=CARTESIAN_POINT('Ctrl Pts',(29.2174939164952,-6.78306424239322,-8.73701514175017));
#31197=CARTESIAN_POINT('Ctrl Pts',(29.5607048332279,-6.78786835107261,-8.73336568489192));
#31198=CARTESIAN_POINT('Ctrl Pts',(29.9899637006214,-6.79106253935676,-8.73093988338427));
#31199=CARTESIAN_POINT('Ctrl Pts',(30.5003627545718,-6.79139754852948,-8.73068255391871));
#31200=CARTESIAN_POINT('Ctrl Pts',(31.5152290141054,-6.78728755019409,-8.73381293113858));
#31201=CARTESIAN_POINT('Ctrl Pts',(32.346385618228,-6.77838967797265,-8.74063107149334));
#31202=CARTESIAN_POINT('Ctrl Pts',(33.1616392309915,-6.77840182636605,-8.74062146997073));
#31203=CARTESIAN_POINT('Ctrl Pts',(33.4928689770884,-6.77840284181041,-8.74062052628883));
#31204=CARTESIAN_POINT('Ctrl Pts',(33.9856875201801,-6.77840526161275,-8.74061852020512));
#31205=CARTESIAN_POINT('Ctrl Pts',(34.4799569296089,-6.7784068708528,-8.74061713883255));
#31206=CARTESIAN_POINT('Ctrl Pts',(35.1382080085716,-6.778409075901,-8.74061527897128));
#31207=CARTESIAN_POINT('Ctrl Pts',(35.9613703496106,-6.7784121544085,-8.74061266742264));
#31208=CARTESIAN_POINT('Ctrl Pts',(37.9364530322258,-6.77841531264166,-8.74060999527037));
#31209=CARTESIAN_POINT('Ctrl Pts',(39.5833333333333,-6.7784348060232,-8.74059347982545));
#31210=CARTESIAN_POINT('Ctrl Pts',(40.9,-6.7784348060232,-8.74059347982545));
#31211=CARTESIAN_POINT('Ctrl Pts',(6.71972576838711,0.727849695365748,-14.4135489955738));
#31212=CARTESIAN_POINT('Ctrl Pts',(6.81144220747046,0.647520064289719,-14.4181051875223));
#31213=CARTESIAN_POINT('Ctrl Pts',(6.90362846895807,0.56728056977469,-14.4219897194692));
#31214=CARTESIAN_POINT('Ctrl Pts',(7.97787094717212,-0.361837668282348,
-14.4591555519285));
#31215=CARTESIAN_POINT('Ctrl Pts',(8.98682261267022,-1.20743712855003,-14.4048184698324));
#31216=CARTESIAN_POINT('Ctrl Pts',(11.0806424583842,-2.74422300498291,-14.2022941804566));
#31217=CARTESIAN_POINT('Ctrl Pts',(12.0862214600973,-3.44223257454471,-14.038891127913));
#31218=CARTESIAN_POINT('Ctrl Pts',(14.1975721203649,-4.69396502652543,-13.6830024292515));
#31219=CARTESIAN_POINT('Ctrl Pts',(15.2099789251839,-5.24642829788655,-13.4699449244818));
#31220=CARTESIAN_POINT('Ctrl Pts',(17.3362999248755,-6.21145869787377,-13.0656161985035));
#31221=CARTESIAN_POINT('Ctrl Pts',(18.357013455463,-6.62511541331198,-12.850252612086));
#31222=CARTESIAN_POINT('Ctrl Pts',(19.7328409259837,-7.07198752003369,-12.6121436508471));
#31223=CARTESIAN_POINT('Ctrl Pts',(20.2337632876373,-7.22841114520151,-12.5247332071257));
#31224=CARTESIAN_POINT('Ctrl Pts',(21.0166345413949,-7.45203181169807,-12.3929576501156));
#31225=CARTESIAN_POINT('Ctrl Pts',(21.8175391230323,-7.65714338227215,-12.2672157657621));
#31226=CARTESIAN_POINT('Ctrl Pts',(22.3668263920487,-7.78054947414231,-12.190248920123));
#31227=CARTESIAN_POINT('Ctrl Pts',(22.7739396967848,-7.86506298164211,-12.1377120270328));
#31228=CARTESIAN_POINT('Ctrl Pts',(23.0274297041713,-7.916156632735,-12.1053188608807));
#31229=CARTESIAN_POINT('Ctrl Pts',(23.5449351393661,-8.01409846114017,-12.0417665186343));
#31230=CARTESIAN_POINT('Ctrl Pts',(24.0699575659665,-8.1034816713378,-11.9817953425795));
#31231=CARTESIAN_POINT('Ctrl Pts',(24.6032835407751,-8.18369268569514,-11.9270075754273));
#31232=CARTESIAN_POINT('Ctrl Pts',(25.0064847905103,-8.23885952183869,-11.8890391550575));
#31233=CARTESIAN_POINT('Ctrl Pts',(25.3452465270805,-8.28045801654025,-11.8603696837558));
#31234=CARTESIAN_POINT('Ctrl Pts',(25.6175460563752,-8.31095886138244,-11.8394640015962));
#31235=CARTESIAN_POINT('Ctrl Pts',(25.75409426488,-8.32525512288968,-11.8297282412419));
#31236=CARTESIAN_POINT('Ctrl Pts',(26.34877806292,-8.38525559473467,-11.7890598714193));
#31237=CARTESIAN_POINT('Ctrl Pts',(27.420647343066,-8.4511591136706,-11.7424863739248));
#31238=CARTESIAN_POINT('Ctrl Pts',(28.4470245212717,-8.47809267828295,-11.7218144944205));
#31239=CARTESIAN_POINT('Ctrl Pts',(29.0301431861018,-8.49498332574136,-11.7097207064843));
#31240=CARTESIAN_POINT('Ctrl Pts',(29.2075511609936,-8.49948124637056,-11.7065424548688));
#31241=CARTESIAN_POINT('Ctrl Pts',(29.5540559241346,-8.50596054299459,-11.7019389390664));
#31242=CARTESIAN_POINT('Ctrl Pts',(29.9873899374288,-8.51027178683721,-11.6988759349841));
#31243=CARTESIAN_POINT('Ctrl Pts',(30.501058587611,-8.51072031244606,-11.6985535595641));
#31244=CARTESIAN_POINT('Ctrl Pts',(31.520398261889,-8.50519297418975,-11.7024891534661));
#31245=CARTESIAN_POINT('Ctrl Pts',(32.3504760849347,-8.49329404471495,-11.7110091605269));
#31246=CARTESIAN_POINT('Ctrl Pts',(33.1607219786944,-8.49331406281709,-11.7109930603161));
#31247=CARTESIAN_POINT('Ctrl Pts',(33.4925972550183,-8.49331574772297,-11.7109914601493));
#31248=CARTESIAN_POINT('Ctrl Pts',(33.9851239882619,-8.49331974280042,-11.7109880844892));
#31249=CARTESIAN_POINT('Ctrl Pts',(34.4795557496198,-8.49332240354984,-11.7109857543654));
#31250=CARTESIAN_POINT('Ctrl Pts',(35.1377808103951,-8.49332604669792,-11.7109826209376));
#31251=CARTESIAN_POINT('Ctrl Pts',(35.9610196518539,-8.49333113419868,-11.7109782193289));
#31252=CARTESIAN_POINT('Ctrl Pts',(37.9361278153251,-8.49333635287233,-11.7109737164007));
#31253=CARTESIAN_POINT('Ctrl Pts',(39.5833333333333,-8.49336856563262,-11.7109458830841));
#31254=CARTESIAN_POINT('Ctrl Pts',(40.9,-8.49336856563262,-11.7109458830841));
#31255=CARTESIAN_POINT('Ctrl Pts',(6.48175880232276,2.0223358101383,-22.3152648782349));
#31256=CARTESIAN_POINT('Ctrl Pts',(6.5727030402579,1.89877066361228,-22.3270401223923));
#31257=CARTESIAN_POINT('Ctrl Pts',(6.66410021308729,1.77531589258794,-22.3377778183098));
#31258=CARTESIAN_POINT('Ctrl Pts',(7.73046719612232,0.343647388924397,-22.4505948584363));
#31259=CARTESIAN_POINT('Ctrl Pts',(8.73293490974102,-0.965853752252137,
-22.4183684385317));
#31260=CARTESIAN_POINT('Ctrl Pts',(10.8102891123217,-3.35126151217317,-22.1981640385547));
#31261=CARTESIAN_POINT('Ctrl Pts',(11.8125652928685,-4.44249581664877,-21.9890905805956));
#31262=CARTESIAN_POINT('Ctrl Pts',(13.9177091187558,-6.40690464277105,-21.5128074248294));
#31263=CARTESIAN_POINT('Ctrl Pts',(14.9295907318602,-7.27826244175744,-21.2167997396941));
#31264=CARTESIAN_POINT('Ctrl Pts',(17.0679705254901,-8.81262608188777,-20.6429560449296));
#31265=CARTESIAN_POINT('Ctrl Pts',(18.0930327325161,-9.47115000177604,-20.3328482957165));
#31266=CARTESIAN_POINT('Ctrl Pts',(19.4931651654931,-10.1918150595348,-19.9834260609175));
#31267=CARTESIAN_POINT('Ctrl Pts',(19.9989304172552,-10.4420751188792,-19.8560672526628));
#31268=CARTESIAN_POINT('Ctrl Pts',(20.794811594708,-10.8025573386247,-19.6618467626018));
#31269=CARTESIAN_POINT('Ctrl Pts',(21.6117660259797,-11.1342859263411,-19.4754657432766));
#31270=CARTESIAN_POINT('Ctrl Pts',(22.1753497026275,-11.3349591405942,-19.3605546952356));
#31271=CARTESIAN_POINT('Ctrl Pts',(22.5940479063322,-11.47260657239,-19.2819382297017));
#31272=CARTESIAN_POINT('Ctrl Pts',(22.8520812047022,-11.5550617085391,-19.2339198113556));
#31273=CARTESIAN_POINT('Ctrl Pts',(23.3813360719091,-11.7138435277865,-19.1391573021403));
#31274=CARTESIAN_POINT('Ctrl Pts',(23.9190563543678,-11.8589452906513,-19.0494991042743));
#31275=CARTESIAN_POINT('Ctrl Pts',(24.4671051082233,-11.989559546254,-18.9672572385016));
#31276=CARTESIAN_POINT('Ctrl Pts',(24.8821466483761,-12.0795190000423,-18.9101500634532));
#31277=CARTESIAN_POINT('Ctrl Pts',(25.2317043848841,-12.1474851335067,-18.8669280179621));
#31278=CARTESIAN_POINT('Ctrl Pts',(25.5130950900239,-12.1973721681455,-18.8353673631031));
#31279=CARTESIAN_POINT('Ctrl Pts',(25.6543465475614,-12.2207724172661,-18.8206563371687));
#31280=CARTESIAN_POINT('Ctrl Pts',(26.2703768283174,-12.3190725812828,-18.7591443923488));
#31281=CARTESIAN_POINT('Ctrl Pts',(27.3823409200252,-12.4269409232394,-18.6887004197342));
#31282=CARTESIAN_POINT('Ctrl Pts',(28.4180912195453,-12.4698946357076,-18.6581821178487));
#31283=CARTESIAN_POINT('Ctrl Pts',(29.0006188348746,-12.4967855079752,-18.6404003655932));
#31284=CARTESIAN_POINT('Ctrl Pts',(29.1842244806991,-12.5041566301777,-18.6355848623939));
#31285=CARTESIAN_POINT('Ctrl Pts',(29.5384110471465,-12.5146498740616,-18.6286952117012));
#31286=CARTESIAN_POINT('Ctrl Pts',(29.9812601150293,-12.5216494975055,-18.6240999155071));
#31287=CARTESIAN_POINT('Ctrl Pts',(30.5025631839301,-12.5223645690813,-18.6236255844566));
#31288=CARTESIAN_POINT('Ctrl Pts',(31.5323495650756,-12.5134871029148,-18.6294670720537));
#31289=CARTESIAN_POINT('Ctrl Pts',(32.3599484134842,-12.4946603930139,-18.6419219593216));
#31290=CARTESIAN_POINT('Ctrl Pts',(33.1585258504257,-12.4947174829697,-18.6418830267369));
#31291=CARTESIAN_POINT('Ctrl Pts',(33.4919095878066,-12.4947228565319,-18.6418790995137));
#31292=CARTESIAN_POINT('Ctrl Pts',(33.9837592380106,-12.4947346270607,-18.6418708983646));
#31293=CARTESIAN_POINT('Ctrl Pts',(34.4785726427749,-12.4947426563109,-18.6418652189506));
#31294=CARTESIAN_POINT('Ctrl Pts',(35.1367406589071,-12.4947535178469,-18.6418575939256));
#31295=CARTESIAN_POINT('Ctrl Pts',(35.9601632093981,-12.4947687456191,-18.641846877137));
#31296=CARTESIAN_POINT('Ctrl Pts',(37.9353361278946,-12.4947843377882,-18.6418359163297));
#31297=CARTESIAN_POINT('Ctrl Pts',(39.5833333333333,-12.4948806713879,-18.6417681573542));
#31298=CARTESIAN_POINT('Ctrl Pts',(40.9,-12.4948806713879,-18.6417681573542));
#31299=CARTESIAN_POINT('Ctrl Pts',(6.40644620858991,3.20016516784475,-30.2320800787095));
#31300=CARTESIAN_POINT('Ctrl Pts',(6.49686818484384,3.03404698664167,-30.2503623618083));
#31301=CARTESIAN_POINT('Ctrl Pts',(6.58771890650216,2.86810360702043,-30.2672526113879));
#31302=CARTESIAN_POINT('Ctrl Pts',(7.64885862899863,0.940991822615538,-30.4476905739236));
#31303=CARTESIAN_POINT('Ctrl Pts',(8.64788707329236,-0.826287776604476,
-30.430792173042));
#31304=CARTESIAN_POINT('Ctrl Pts',(10.707154859542,-4.031357203037,-30.1856445659011));
#31305=CARTESIAN_POINT('Ctrl Pts',(11.7059935225822,-5.50908116677459,-29.9282222211751));
#31306=CARTESIAN_POINT('Ctrl Pts',(13.7894394913649,-8.15261547988191,-29.3339211293757));
#31307=CARTESIAN_POINT('Ctrl Pts',(14.7965025532944,-9.33507154947816,-28.9559671306032));
#31308=CARTESIAN_POINT('Ctrl Pts',(16.9150296648082,-11.4103698853377,-28.2210428396417));
#31309=CARTESIAN_POINT('Ctrl Pts',(17.9356459667173,-12.3080290796725,-27.8189128366825));
#31310=CARTESIAN_POINT('Ctrl Pts',(19.3316976380886,-13.2937048286054,-27.3625462801585));
#31311=CARTESIAN_POINT('Ctrl Pts',(19.8372125803626,-13.6366910969767,-27.1960046691455));
#31312=CARTESIAN_POINT('Ctrl Pts',(20.6335801906183,-14.1320040365234,-26.9406914971977));
#31313=CARTESIAN_POINT('Ctrl Pts',(21.4537597225929,-14.5899345529251,-26.6943052661747));
#31314=CARTESIAN_POINT('Ctrl Pts',(22.0223258890083,-14.8686659459061,-26.5413031957662));
#31315=CARTESIAN_POINT('Ctrl Pts',(22.4461030502075,-15.0605640384028,-26.436200781156));
#31316=CARTESIAN_POINT('Ctrl Pts',(22.7062608359972,-15.1748824403433,-26.3723989822776));
#31317=CARTESIAN_POINT('Ctrl Pts',(23.2414929286472,-15.3959532265256,-26.2458547955408));
#31318=CARTESIAN_POINT('Ctrl Pts',(23.7867279834486,-15.5986167246948,-26.1256827576297));
#31319=CARTESIAN_POINT('Ctrl Pts',(24.3445890668936,-15.7819085569279,-26.0148742888258));
#31320=CARTESIAN_POINT('Ctrl Pts',(24.7681394700222,-15.9085256074861,-25.9376795444545));
#31321=CARTESIAN_POINT('Ctrl Pts',(25.1260106169383,-16.0045350828092,-25.8790242908718));
#31322=CARTESIAN_POINT('Ctrl Pts',(25.4147345926424,-16.0751760807979,-25.8360764159907));
#31323=CARTESIAN_POINT('Ctrl Pts',(25.5598889289846,-16.1083660281041,-25.816019030982));
#31324=CARTESIAN_POINT('Ctrl Pts',(26.193933911503,-16.2480157393789,-25.7320023110876));
#31325=CARTESIAN_POINT('Ctrl Pts',(27.3441597812047,-16.4017510524694,-25.6354753903564));
#31326=CARTESIAN_POINT('Ctrl Pts',(28.3894038584673,-16.4608066876634,-25.5950614103761));
#31327=CARTESIAN_POINT('Ctrl Pts',(28.9713246547182,-16.4977059168027,-25.5715886293348));
#31328=CARTESIAN_POINT('Ctrl Pts',(29.1610585442185,-16.5082319208974,-25.5649734110425));
#31329=CARTESIAN_POINT('Ctrl Pts',(29.5228882487203,-16.5229807852931,-25.5556580156131));
#31330=CARTESIAN_POINT('Ctrl Pts',(29.9752283100297,-16.5328527231063,-25.5494240137562));
#31331=CARTESIAN_POINT('Ctrl Pts',(30.5041683224499,-16.5338357099673,-25.5487969550272));
#31332=CARTESIAN_POINT('Ctrl Pts',(31.5443819697417,-16.5215002939531,-25.5566068476798));
#31333=CARTESIAN_POINT('Ctrl Pts',(32.3694794643941,-16.4958953935747,-25.5729102090687));
#31334=CARTESIAN_POINT('Ctrl Pts',(33.1563754893963,-16.4960222658506,-25.5728296448089));
#31335=CARTESIAN_POINT('Ctrl Pts',(33.4912658278754,-16.4960347835491,-25.572821407314));
#31336=CARTESIAN_POINT('Ctrl Pts',(33.9824352992262,-16.4960613233721,-25.5728043629855));
#31337=CARTESIAN_POINT('Ctrl Pts',(34.4776280283123,-16.4960796138348,-25.5727925244551));
#31338=CARTESIAN_POINT('Ctrl Pts',(35.1357360035507,-16.4961042295225,-25.5727766538608));
#31339=CARTESIAN_POINT('Ctrl Pts',(35.9593379975622,-16.4961387987434,-25.5727543372373));
#31340=CARTESIAN_POINT('Ctrl Pts',(37.9345713338105,-16.4961741679457,-25.5727315175493));
#31341=CARTESIAN_POINT('Ctrl Pts',(39.5833333333333,-16.4963927771432,-25.5725904316243));
#31342=CARTESIAN_POINT('Ctrl Pts',(40.9,-16.4963927771432,-25.5725904316243));
#31343=CARTESIAN_POINT('Ctrl Pts',(6.37427268165564,3.85496595036637,-34.7583359408307));
#31344=CARTESIAN_POINT('Ctrl Pts',(6.46448755772838,3.66446375246399,-34.7802475524424));
#31345=CARTESIAN_POINT('Ctrl Pts',(6.55512331969025,3.47417181608893,-34.8005635888992));
#31346=CARTESIAN_POINT('Ctrl Pts',(7.61410548625795,1.26339052014804,-35.0185788676572));
#31347=CARTESIAN_POINT('Ctrl Pts',(8.61145388480624,-0.76560245720769,-35.0093532870147));
#31348=CARTESIAN_POINT('Ctrl Pts',(10.6635149436019,-4.43910992978125,-34.747974440135));
#31349=CARTESIAN_POINT('Ctrl Pts',(11.6608017032625,-6.13747453196185,-34.4619345886989));
#31350=CARTESIAN_POINT('Ctrl Pts',(13.7353542747945,-9.16685810272324,-33.7990269238398));
#31351=CARTESIAN_POINT('Ctrl Pts',(14.7402715202386,-10.526297955279,-33.3736740493576));
#31352=CARTESIAN_POINT('Ctrl Pts',(16.8491677832147,-12.9054531131771,-32.5473921410153));
#31353=CARTESIAN_POINT('Ctrl Pts',(17.8672809631136,-13.9382203331611,-32.092886041556));
#31354=CARTESIAN_POINT('Ctrl Pts',(19.2587625104673,-15.0707179501981,-31.577179869867));
#31355=CARTESIAN_POINT('Ctrl Pts',(19.7635899403542,-15.4658689812884,-31.3885503410944));
#31356=CARTESIAN_POINT('Ctrl Pts',(20.5586991602297,-16.0362969262867,-31.0991569516509));
#31357=CARTESIAN_POINT('Ctrl Pts',(21.3785272493018,-16.564533786793,-30.819343278526));
#31358=CARTESIAN_POINT('Ctrl Pts',(21.9479176287994,-16.8867906552356,-30.6451300260617));
#31359=CARTESIAN_POINT('Ctrl Pts',(22.3729695502115,-17.1090467735268,-30.525234440013));
#31360=CARTESIAN_POINT('Ctrl Pts',(22.6337096028248,-17.2413581349254,-30.45253373981));
#31361=CARTESIAN_POINT('Ctrl Pts',(23.1707519864209,-17.4975676797996,-30.3080867629256));
#31362=CARTESIAN_POINT('Ctrl Pts',(23.7186485394885,-17.7328951431605,-30.170626807131));
#31363=CARTESIAN_POINT('Ctrl Pts',(24.2804077704385,-17.946249160495,-30.0435395405948));
#31364=CARTESIAN_POINT('Ctrl Pts',(24.7075732751058,-18.0938968083019,-29.9548357769835));
#31365=CARTESIAN_POINT('Ctrl Pts',(25.0692008252975,-18.2061112471098,-29.8872739715487));
#31366=CARTESIAN_POINT('Ctrl Pts',(25.3613771492325,-18.28880476277,-29.8377189043884));
#31367=CARTESIAN_POINT('Ctrl Pts',(25.5084154817281,-18.3277015544066,-29.8145466170753));
#31368=CARTESIAN_POINT('Ctrl Pts',(26.1512870025444,-18.4915385207408,-29.7173716879777));
#31369=CARTESIAN_POINT('Ctrl Pts',(27.3223884400173,-18.6726738474942,-29.6052740416531));
#31370=CARTESIAN_POINT('Ctrl Pts',(28.3731396048321,-18.7409825767551,-29.559177524821));
#31371=CARTESIAN_POINT('Ctrl Pts',(28.9547046473315,-18.7836137746098,-29.5324480977279));
#31372=CARTESIAN_POINT('Ctrl Pts',(29.1479037067738,-18.7960320303041,-29.5247529606444));
#31373=CARTESIAN_POINT('Ctrl Pts',(29.5140802367921,-18.8132921881813,-29.51400582112));
#31374=CARTESIAN_POINT('Ctrl Pts',(29.9718311305158,-18.8248686377542,-29.5067996680497));
#31375=CARTESIAN_POINT('Ctrl Pts',(30.5051365276119,-18.8260067178222,-29.5060845192011));
#31376=CARTESIAN_POINT('Ctrl Pts',(31.551298475448,-18.8116639693829,-29.5150383037988));
#31377=CARTESIAN_POINT('Ctrl Pts',(32.3749555043413,-18.7822473977007,-29.5335081969199));
#31378=CARTESIAN_POINT('Ctrl Pts',(33.1551698865007,-18.7824304492383,-29.5333957726549));
#31379=CARTESIAN_POINT('Ctrl Pts',(33.4909201969602,-18.782448957068,-29.5333841560219));
#31380=CARTESIAN_POINT('Ctrl Pts',(33.981699427726,-18.7824875453788,-29.5333602907362));
#31381=CARTESIAN_POINT('Ctrl Pts',(34.4771077390558,-18.7825142819534,-29.533343676228));
#31382=CARTESIAN_POINT('Ctrl Pts',(35.1351798881798,-18.7825501686284,-29.5333214285967));
#31383=CARTESIAN_POINT('Ctrl Pts',(35.958882261465,-18.7826006107083,-29.5332901329543));
#31384=CARTESIAN_POINT('Ctrl Pts',(37.9341479260215,-18.7826521993715,-29.5332581373787));
#31385=CARTESIAN_POINT('Ctrl Pts',(39.5833333333333,-18.7829711232891,-29.5330603026358));
#31386=CARTESIAN_POINT('Ctrl Pts',(40.9,-18.7829711232891,-29.5330603026358));
#31387=CARTESIAN_POINT('',(40.9,-17.7819838375536,-27.7992994660114));
#31388=CARTESIAN_POINT('Ctrl Pts',(40.9,-17.7819838375536,-27.7992994660114));
#31389=CARTESIAN_POINT('Ctrl Pts',(40.9,-18.0322312401327,-28.2327406817405));
#31390=CARTESIAN_POINT('Ctrl Pts',(40.9,-18.2824786427117,-28.6661818974695));
#31391=CARTESIAN_POINT('Ctrl Pts',(40.9,-18.5327260452908,-29.0996231131986));
#31392=CARTESIAN_POINT('',(38.,-17.7819838375536,-27.7992994660114));
#31393=CARTESIAN_POINT('Ctrl Pts',(38.,-17.7819838375536,-27.7992994660114));
#31394=CARTESIAN_POINT('Ctrl Pts',(38.9666666666667,-17.7819838375536,-27.7992994660114));
#31395=CARTESIAN_POINT('Ctrl Pts',(39.9333333333333,-17.7819838375536,-27.7992994660114));
#31396=CARTESIAN_POINT('Ctrl Pts',(40.9,-17.7819838375536,-27.7992994660114));
#31397=CARTESIAN_POINT('Ctrl Pts',(37.4972421947179,-17.4814252073799,-27.2792895089189));
#31398=CARTESIAN_POINT('Ctrl Pts',(37.6643036200225,-17.5817077438358,-27.4529624980705));
#31399=CARTESIAN_POINT('Ctrl Pts',(37.8311445342373,-17.6818443698597,-27.6263779214721));
#31400=CARTESIAN_POINT('Ctrl Pts',(37.9976555467136,-17.7817739539416,-27.7994312893194));
#31401=CARTESIAN_POINT('',(6.9,2.26556458774883,-29.9143312995417));
#31402=CARTESIAN_POINT('Ctrl Pts',(6.9,2.26556458774883,-29.9143312995417));
#31403=CARTESIAN_POINT('Ctrl Pts',(6.9,2.00382962437802,-27.3056186709172));
#31404=CARTESIAN_POINT('Ctrl Pts',(6.90000000000115,1.73285728374608,-24.6693701926632));
#31405=CARTESIAN_POINT('Ctrl Pts',(6.90000000000115,1.09593289590079,-18.7182130985667));
#31406=CARTESIAN_POINT('Ctrl Pts',(6.9,0.654794893503688,-14.7845781982083));
#31407=CARTESIAN_POINT('Ctrl Pts',(6.9,0.168526548660244,-11.02768739857));
#31408=CARTESIAN_POINT('',(22.9245129145126,-15.8853026165582,-27.5141512254856));
#31409=CARTESIAN_POINT('Ctrl Pts',(22.9245129145126,-15.8853026165582,-27.5141512254856));
#31410=CARTESIAN_POINT('Ctrl Pts',(22.7202811020963,-15.7659233420327,-27.5032269692373));
#31411=CARTESIAN_POINT('Ctrl Pts',(22.5089075447093,-15.6398559109135,-27.4959054260063));
#31412=CARTESIAN_POINT('Ctrl Pts',(22.2913349439917,-15.5073965833875,-27.4928730439354));
#31413=CARTESIAN_POINT('Ctrl Pts',(21.445177058529,-14.9922512750188,-27.4810798586143));
#31414=CARTESIAN_POINT('Ctrl Pts',(20.5220951556664,-14.3509960808543,-27.5650257717265));
#31415=CARTESIAN_POINT('Ctrl Pts',(19.7671428819534,-13.785930418101,-27.676239960775));
#31416=CARTESIAN_POINT('Ctrl Pts',(19.5194773058388,-13.600558020691,-27.7127242885423));
#31417=CARTESIAN_POINT('Ctrl Pts',(19.2865716386089,-13.421872324025,-27.7514615171005));
#31418=CARTESIAN_POINT('Ctrl Pts',(19.0728538401323,-13.2552441975238,-27.7894004949774));
#31419=CARTESIAN_POINT('Ctrl Pts',(18.7028555998035,-12.9667697979459,-27.8550822264681));
#31420=CARTESIAN_POINT('Ctrl Pts',(18.4144703596236,-12.7292901983115,-27.9152561335183));
#31421=CARTESIAN_POINT('Ctrl Pts',(18.0642874871538,-12.4284122845047,-27.9946062155751));
#31422=CARTESIAN_POINT('Ctrl Pts',(17.4420927116721,-11.8938211301513,-28.1355931408966));
#31423=CARTESIAN_POINT('Ctrl Pts',(16.7224564418218,-11.2282910364348,-28.3254287038798));
#31424=CARTESIAN_POINT('Ctrl Pts',(15.9202806616111,-10.4246142212493,-28.5439924969395));
#31425=CARTESIAN_POINT('Ctrl Pts',(15.4090529834518,-9.91242993152957,-28.6832834892781));
#31426=CARTESIAN_POINT('Ctrl Pts',(14.8739602945714,-9.33532862360331,-28.8377564730262));
#31427=CARTESIAN_POINT('Ctrl Pts',(14.3169794331154,-8.6917184299937,-28.9944199787763));
#31428=CARTESIAN_POINT('Ctrl Pts',(13.8864206762836,-8.19419324731423,-29.1155243989539));
#31429=CARTESIAN_POINT('Ctrl Pts',(13.3867890027804,-7.59173852185132,-29.2546860278644));
#31430=CARTESIAN_POINT('Ctrl Pts',(12.8146824059514,-6.86770373383358,-29.3960736315876));
#31431=CARTESIAN_POINT('Ctrl Pts',(12.2526665517595,-6.15643937836578,-29.5349674589251));
#31432=CARTESIAN_POINT('Ctrl Pts',(11.6379478462803,-5.32066918438559,-29.678401911158));
#31433=CARTESIAN_POINT('Ctrl Pts',(10.9739250490308,-4.35448584003993,-29.7956367796097));
#31434=CARTESIAN_POINT('Ctrl Pts',(10.5683455447963,-3.76434923114268,-29.8672428449776));
#31435=CARTESIAN_POINT('Ctrl Pts',(10.1437415406956,-3.12422765605932,-29.9275397584159));
#31436=CARTESIAN_POINT('Ctrl Pts',(9.74137929176525,-2.50486371218385,-29.9670595377668));
#31437=CARTESIAN_POINT('Ctrl Pts',(8.72285779294234,-0.93703399130421,-30.0670981099855));
#31438=CARTESIAN_POINT('Ctrl Pts',(7.81323138778195,0.638451825302681,-30.0560666286387));
#31439=CARTESIAN_POINT('Ctrl Pts',(6.9,2.26556458774884,-29.9143312995417));
#31440=CARTESIAN_POINT('Ctrl Pts',(30.5,-18.8254200738635,-29.5059919176187));
#31441=CARTESIAN_POINT('Ctrl Pts',(29.9560179420816,-18.7064245513841,-29.293615660989));
#31442=CARTESIAN_POINT('Ctrl Pts',(29.4152668325132,-18.5734800115823,-29.0895919906434));
#31443=CARTESIAN_POINT('Ctrl Pts',(28.8740459957565,-18.4125151878636,-28.9020067835811));
#31444=CARTESIAN_POINT('Ctrl Pts',(28.353527792344,-18.2577075471291,-28.7215970352204));
#31445=CARTESIAN_POINT('Ctrl Pts',(27.8179515912466,-18.1008601332298,-28.533139934629));
#31446=CARTESIAN_POINT('Ctrl Pts',(27.2695051149491,-17.9186544331585,-28.3565719042575));
#31447=CARTESIAN_POINT('Ctrl Pts',(26.9554553615883,-17.8143203592948,-28.2554660556724));
#31448=CARTESIAN_POINT('Ctrl Pts',(26.6378099296971,-17.7019284120276,-28.1585101274348));
#31449=CARTESIAN_POINT('Ctrl Pts',(26.3179304017917,-17.5778023417279,-28.0701057587103));
#31450=CARTESIAN_POINT('Ctrl Pts',(26.1078196745982,-17.4962709631331,-28.012037940737));
#31451=CARTESIAN_POINT('Ctrl Pts',(25.8967402232745,-17.409683568055,-27.9576659729224));
#31452=CARTESIAN_POINT('Ctrl Pts',(25.6850706236774,-17.3169960819306,-27.9082593406129));
#31453=CARTESIAN_POINT('Ctrl Pts',(25.6562210027417,-17.3043631915899,-27.9015254373195));
#31454=CARTESIAN_POINT('Ctrl Pts',(25.6277737638215,-17.2918013331136,-27.8949772388532));
#31455=CARTESIAN_POINT('Ctrl Pts',(25.5983858063598,-17.2787081509674,-27.8883138877393));
#31456=CARTESIAN_POINT('Ctrl Pts',(25.1249357452756,-17.067772501732,-27.7809650188704));
#31457=CARTESIAN_POINT('Ctrl Pts',(24.1510084067019,-16.6022239440147,-27.5797558484168));
#31458=CARTESIAN_POINT('Ctrl Pts',(22.9245129145126,-15.8853026165582,-27.5141512254856));
#31459=CARTESIAN_POINT('Origin',(40.65,0.,0.));
#31460=CARTESIAN_POINT('',(40.4,1.49999999999999,-34.9678423698117));
#31461=CARTESIAN_POINT('',(40.9,1.49999999999999,-34.4673758792282));
#31462=CARTESIAN_POINT('Ctrl Pts',(40.4,1.49999999999999,-34.9678423698117));
#31463=CARTESIAN_POINT('Ctrl Pts',(40.5666590142087,1.49999999999999,-34.8010300902431));
#31464=CARTESIAN_POINT('Ctrl Pts',(40.733343045307,1.49999999999999,-34.6341905783528));
#31465=CARTESIAN_POINT('Ctrl Pts',(40.9,1.49999999999999,-34.4673758792282));
#31466=CARTESIAN_POINT('',(40.9,-1.50000000000002,-34.4673758792282));
#31467=CARTESIAN_POINT('Origin',(40.9,0.,0.));
#31468=CARTESIAN_POINT('',(40.4,-1.50000000000001,-34.9678423698117));
#31469=CARTESIAN_POINT('Ctrl Pts',(40.9,-1.50000000000001,-34.4673758792282));
#31470=CARTESIAN_POINT('Ctrl Pts',(40.7333430449637,-1.50000000000001,-34.6341905786964));
#31471=CARTESIAN_POINT('Ctrl Pts',(40.5666590137783,-1.50000000000001,-34.8010300906738));
#31472=CARTESIAN_POINT('Ctrl Pts',(40.4,-1.50000000000001,-34.9678423698117));
#31473=CARTESIAN_POINT('Origin',(40.4,0.,0.));
#31474=CARTESIAN_POINT('Origin',(35.7,0.,0.));
#31475=CARTESIAN_POINT('',(30.5,-1.55029606206997,-34.9656486014478));
#31476=CARTESIAN_POINT('Ctrl Pts',(40.3999915729117,-1.49999518538963,-34.9678423422331));
#31477=CARTESIAN_POINT('Ctrl Pts',(39.2499539542075,-1.49997392326491,-34.9678422204405));
#31478=CARTESIAN_POINT('Ctrl Pts',(38.0997984110589,-1.49988846741895,-34.9678417309291));
#31479=CARTESIAN_POINT('Ctrl Pts',(36.9496886126402,-1.49986523425637,-34.9678415977222));
#31480=CARTESIAN_POINT('Ctrl Pts',(36.7850895654027,-1.49986190922042,-34.9678415786582));
#31481=CARTESIAN_POINT('Ctrl Pts',(36.6204914551167,-1.49985985864023,-34.967841566892));
#31482=CARTESIAN_POINT('Ctrl Pts',(36.4559074066593,-1.49985712176039,-34.9678415512222));
#31483=CARTESIAN_POINT('Ctrl Pts',(36.4193481336993,-1.49985651381364,-34.9678415477415));
#31484=CARTESIAN_POINT('Ctrl Pts',(36.3827895545826,-1.49985587200327,-34.9678415440681));
#31485=CARTESIAN_POINT('Ctrl Pts',(36.3462314281453,-1.49985520449066,-34.9678415402484));
#31486=CARTESIAN_POINT('Ctrl Pts',(36.0893715793236,-1.49985051450228,-34.967841513411));
#31487=CARTESIAN_POINT('Ctrl Pts',(35.8498573424242,-1.49984503951475,-34.9678415998896));
#31488=CARTESIAN_POINT('Ctrl Pts',(35.6261955219287,-1.49984104357288,-34.967841744545));
#31489=CARTESIAN_POINT('Ctrl Pts',(35.5726950208743,-1.49984008773299,-34.9678417791469));
#31490=CARTESIAN_POINT('Ctrl Pts',(35.5201018010634,-1.49983920821971,-34.9678418170305));
#31491=CARTESIAN_POINT('Ctrl Pts',(35.4683958334514,-1.49983842183596,-34.9678418573607));
#31492=CARTESIAN_POINT('Ctrl Pts',(35.3126687160222,-1.4998360534193,-34.9678419788262));
#31493=CARTESIAN_POINT('Ctrl Pts',(35.1649944183664,-1.49983427390521,-34.9678421210274));
#31494=CARTESIAN_POINT('Ctrl Pts',(35.0249177028203,-1.49982884904642,-34.9678422344455));
#31495=CARTESIAN_POINT('Ctrl Pts',(35.0080273577823,-1.49982819492103,-34.9678422481214));
#31496=CARTESIAN_POINT('Ctrl Pts',(34.9912474154116,-1.49982749115044,-34.9678422613979));
#31497=CARTESIAN_POINT('Ctrl Pts',(34.9745770299108,-1.49982673292213,-34.967842274203));
#31498=CARTESIAN_POINT('Ctrl Pts',(34.8398252803349,-1.49982060393425,-34.9678423777109));
#31499=CARTESIAN_POINT('Ctrl Pts',(34.7122270228894,-1.49981110422879,-34.9678424514863));
#31500=CARTESIAN_POINT('Ctrl Pts',(34.5911971286586,-1.49980195022803,-34.9678424931048));
#31501=CARTESIAN_POINT('Ctrl Pts',(34.4536573923533,-1.49979154751836,-34.9678425404006));
#31502=CARTESIAN_POINT('Ctrl Pts',(34.324600768997,-1.49978157387808,-34.9678425460693));
#31503=CARTESIAN_POINT('Ctrl Pts',(34.2032402166286,-1.49977474411704,-34.9678424909992));
#31504=CARTESIAN_POINT('Ctrl Pts',(34.1282158883669,-1.49977052200182,-34.9678424569553));
#31505=CARTESIAN_POINT('Ctrl Pts',(34.0561340587984,-1.49976744984812,-34.9678423994066));
#31506=CARTESIAN_POINT('Ctrl Pts',(33.9868183126576,-1.49976579826338,-34.9678423117327));
#31507=CARTESIAN_POINT('Ctrl Pts',(33.9445485903809,-1.49976479110364,-34.967842258268));
#31508=CARTESIAN_POINT('Ctrl Pts',(33.9033113298609,-1.49976427568321,-34.9678421933981));
#31509=CARTESIAN_POINT('Ctrl Pts',(33.8632060391111,-1.49976308937533,-34.9678421088662));
#31510=CARTESIAN_POINT('Ctrl Pts',(33.8167294892623,-1.49976171460666,-34.9678420109052));
#31511=CARTESIAN_POINT('Ctrl Pts',(33.7717637484314,-1.49975949629186,-34.9678418868506));
#31512=CARTESIAN_POINT('Ctrl Pts',(33.7280832525525,-1.49975712824878,-34.9678417374965));
#31513=CARTESIAN_POINT('Ctrl Pts',(33.6812412750936,-1.49975458881285,-34.9678415773325));
#31514=CARTESIAN_POINT('Ctrl Pts',(33.6358775556469,-1.49975187629478,-34.9678413880696));
#31515=CARTESIAN_POINT('Ctrl Pts',(33.5917762634972,-1.49974959276977,-34.967841169348));
#31516=CARTESIAN_POINT('Ctrl Pts',(33.5583149104291,-1.49974786017117,-34.9678410033954));
#31517=CARTESIAN_POINT('Ctrl Pts',(33.5255817104614,-1.49974636887339,-34.967840820454));
#31518=CARTESIAN_POINT('Ctrl Pts',(33.4935021420768,-1.49974530120961,-34.9678406199406));
#31519=CARTESIAN_POINT('Ctrl Pts',(33.4573943589309,-1.49974409947985,-34.9678403942487));
#31520=CARTESIAN_POINT('Ctrl Pts',(33.4221208193067,-1.49974341134213,-34.9678401461735));
#31521=CARTESIAN_POINT('Ctrl Pts',(33.3878054439024,-1.49974262313064,-34.9678398702965));
#31522=CARTESIAN_POINT('Ctrl Pts',(33.3506623489709,-1.49974176996748,-34.9678395716863));
#31523=CARTESIAN_POINT('Ctrl Pts',(33.3146417056247,-1.49974080006053,-34.9678392405062));
#31524=CARTESIAN_POINT('Ctrl Pts',(33.2798370373775,-1.49973916665773,-34.9678388710955));
#31525=CARTESIAN_POINT('Ctrl Pts',(33.2432420311725,-1.49973744923335,-34.9678384826825));
#31526=CARTESIAN_POINT('Ctrl Pts',(33.2079907612227,-1.4997350003436,-34.9678380520153));
#31527=CARTESIAN_POINT('Ctrl Pts',(33.1741302661583,-1.49973140839958,-34.9678375736847));
#31528=CARTESIAN_POINT('Ctrl Pts',(33.1370268066149,-1.49972747243971,-34.9678370495424));
#31529=CARTESIAN_POINT('Ctrl Pts',(33.1015929393419,-1.49972216527192,-34.9678364681763));
#31530=CARTESIAN_POINT('Ctrl Pts',(33.067825091431,-1.49971518245857,-34.9678358237089));
#31531=CARTESIAN_POINT('Ctrl Pts',(33.0456190541537,-1.49971059049838,-34.9678353999014));
#31532=CARTESIAN_POINT('Ctrl Pts',(33.0241321462894,-1.49970527875611,-34.9678349488311));
#31533=CARTESIAN_POINT('Ctrl Pts',(33.00335138524,-1.49969920384722,-34.9678344690522));
#31534=CARTESIAN_POINT('Ctrl Pts',(32.9442304423539,-1.49968192082565,-34.9678331040887));
#31535=CARTESIAN_POINT('Ctrl Pts',(32.8886870683166,-1.49990565391071,-34.9678225550375));
#31536=CARTESIAN_POINT('Ctrl Pts',(32.8362378081004,-1.50026775301229,-34.9678066545694));
#31537=CARTESIAN_POINT('Ctrl Pts',(32.7772899725208,-1.50067471696594,-34.9677887839993));
#31538=CARTESIAN_POINT('Ctrl Pts',(32.722250704254,-1.50125685144361,-34.9677641385155));
#31539=CARTESIAN_POINT('Ctrl Pts',(32.6703984222899,-1.50192703269666,-34.9677359437545));
#31540=CARTESIAN_POINT('Ctrl Pts',(32.6144142271636,-1.50265061817099,-34.9677055022591));
#31541=CARTESIAN_POINT('Ctrl Pts',(32.5621451030132,-1.50347772465866,-34.9676708895142));
#31542=CARTESIAN_POINT('Ctrl Pts',(32.512643139679,-1.50435187710663,-34.9676341616883));
#31543=CARTESIAN_POINT('Ctrl Pts',(32.4592340800666,-1.5052950247529,-34.9675945350046));
#31544=CARTESIAN_POINT('Ctrl Pts',(32.4090461376418,-1.50629382208342,-34.9675524123823));
#31545=CARTESIAN_POINT('Ctrl Pts',(32.3608457191396,-1.50732223503495,-34.9675086930052));
#31546=CARTESIAN_POINT('Ctrl Pts',(32.3080489575157,-1.50844871640463,-34.9674608045926));
#31547=CARTESIAN_POINT('Ctrl Pts',(32.2576369811114,-1.50961152287641,-34.9674109699093));
#31548=CARTESIAN_POINT('Ctrl Pts',(32.2079387024057,-1.510814387538,-34.9673589596438));
#31549=CARTESIAN_POINT('Ctrl Pts',(32.1569651256412,-1.51204811868044,-34.9673056147528));
#31550=CARTESIAN_POINT('Ctrl Pts',(32.1067423359644,-1.51332494201266,-34.9672499447226));
#31551=CARTESIAN_POINT('Ctrl Pts',(32.0554173210335,-1.51467266340921,-34.9671908342291));
#31552=CARTESIAN_POINT('Ctrl Pts',(32.0053517019588,-1.515987314874,-34.9671331741689));
#31553=CARTESIAN_POINT('Ctrl Pts',(31.9542374237157,-1.51737028688898,-34.9670722073686));
#31554=CARTESIAN_POINT('Ctrl Pts',(31.9003072570603,-1.51885640484753,-34.9670065941482));
#31555=CARTESIAN_POINT('Ctrl Pts',(31.8778006425156,-1.51947660474927,-34.9669792118583));
#31556=CARTESIAN_POINT('Ctrl Pts',(31.8548030119451,-1.52011480778718,-34.9669510193556));
#31557=CARTESIAN_POINT('Ctrl Pts',(31.8311831714798,-1.52077345952528,-34.966921924937));
#31558=CARTESIAN_POINT('Ctrl Pts',(31.7273359798822,-1.52366929336221,-34.9667940081687));
#31559=CARTESIAN_POINT('Ctrl Pts',(31.6209566880911,-1.52669736830073,-34.9666588995974));
#31560=CARTESIAN_POINT('Ctrl Pts',(31.5128850686401,-1.52967035112202,-34.966525984972));
#31561=CARTESIAN_POINT('Ctrl Pts',(31.4048094944667,-1.53264344273527,-34.9663930654827));
#31562=CARTESIAN_POINT('Ctrl Pts',(31.2950411944129,-1.5355595885407,-34.9662624112288));
#31563=CARTESIAN_POINT('Ctrl Pts',(31.1844688435936,-1.53821966510477,-34.9661438178107));
#31564=CARTESIAN_POINT('Ctrl Pts',(31.1320862054071,-1.53947985200658,-34.9660876352654));
#31565=CARTESIAN_POINT('Ctrl Pts',(31.0795238479782,-1.54068257273422,-34.9660341587666));
#31566=CARTESIAN_POINT('Ctrl Pts',(31.0268803009881,-1.5418076100978,-34.9659843897334));
#31567=CARTESIAN_POINT('Ctrl Pts',(30.9324572739831,-1.54382551047565,-34.9658951225195));
#31568=CARTESIAN_POINT('Ctrl Pts',(30.837770831616,-1.54559180591447,-34.9658178374821));
#31569=CARTESIAN_POINT('Ctrl Pts',(30.7433264837577,-1.54696313276377,-34.9657578054117));
#31570=CARTESIAN_POINT('Ctrl Pts',(30.6607858411442,-1.5481616184534,-34.9657053397451));
#31571=CARTESIAN_POINT('Ctrl Pts',(30.5784303320586,-1.54905826480272,-34.965666053989));
#31572=CARTESIAN_POINT('Ctrl Pts',(30.4966228217932,-1.54957830485528,-34.965642796755));
#31573=CARTESIAN_POINT('',(30.5,1.44976976333441,-34.9699609326822));
#31574=CARTESIAN_POINT('Origin',(30.5,0.,0.));
#31575=CARTESIAN_POINT('Ctrl Pts',(30.5051992612603,1.44903843638966,-34.9699071381489));
#31576=CARTESIAN_POINT('Ctrl Pts',(30.6030952980657,1.44976082626916,-34.9698787568566));
#31577=CARTESIAN_POINT('Ctrl Pts',(30.7001121880333,1.45104998650339,-34.9698264221104));
#31578=CARTESIAN_POINT('Ctrl Pts',(30.7969947619801,1.45274237549662,-34.9697577270266));
#31579=CARTESIAN_POINT('Ctrl Pts',(30.8545454823775,1.45374769773142,-34.9697169203944));
#31580=CARTESIAN_POINT('Ctrl Pts',(30.9120492097055,1.45489634227782,-34.9696702850816));
#31581=CARTESIAN_POINT('Ctrl Pts',(30.9696671110348,1.45616096255286,-34.9696190483589));
#31582=CARTESIAN_POINT('Ctrl Pts',(31.0687356284601,1.45833535719175,-34.969530951673));
#31583=CARTESIAN_POINT('Ctrl Pts',(31.1681385828748,1.46085179879274,-34.9694292858245));
#31584=CARTESIAN_POINT('Ctrl Pts',(31.2685908593294,1.46356721252908,-34.9693191238307));
#31585=CARTESIAN_POINT('Ctrl Pts',(31.3711796386319,1.46634037995092,-34.9692066188196));
#31586=CARTESIAN_POINT('Ctrl Pts',(31.4748629185106,1.46932276608705,-34.9690851710714));
#31587=CARTESIAN_POINT('Ctrl Pts',(31.5804543970555,1.4723695155306,-34.9689598486836));
#31588=CARTESIAN_POINT('Ctrl Pts',(31.6427002532174,1.47416556508155,-34.9688859715162));
#31589=CARTESIAN_POINT('Ctrl Pts',(31.7056101943812,1.47598400420447,-34.9688107472906));
#31590=CARTESIAN_POINT('Ctrl Pts',(31.7693590594471,1.4777925610394,-34.9687353433411));
#31591=CARTESIAN_POINT('Ctrl Pts',(31.8369567664635,1.47971030961302,-34.968655386873));
#31592=CARTESIAN_POINT('Ctrl Pts',(31.8998289473023,1.48145356148269,-34.9685826953725));
#31593=CARTESIAN_POINT('Ctrl Pts',(31.9584912820088,1.48302365833457,-34.9685172658125));
#31594=CARTESIAN_POINT('Ctrl Pts',(32.0219681801223,1.484722616932,-34.9684464662861));
#31595=CARTESIAN_POINT('Ctrl Pts',(32.0805160965733,1.48621979971339,-34.9683841232145));
#31596=CARTESIAN_POINT('Ctrl Pts',(32.1348442130202,1.48754049944246,-34.9683291276834));
#31597=CARTESIAN_POINT('Ctrl Pts',(32.1955320114797,1.48901580107678,-34.9682676943422));
#31598=CARTESIAN_POINT('Ctrl Pts',(32.2509543450015,1.49027186778442,-34.9682153821449));
#31599=CARTESIAN_POINT('Ctrl Pts',(32.3021641802418,1.49135570584798,-34.968170114115));
#31600=CARTESIAN_POINT('Ctrl Pts',(32.3568725417847,1.49251358898424,-34.9681217534879));
#31601=CARTESIAN_POINT('Ctrl Pts',(32.4067738547306,1.49347579219526,-34.9680813901956));
#31602=CARTESIAN_POINT('Ctrl Pts',(32.453214342574,1.4942964704374,-34.9680466762592));
#31603=CARTESIAN_POINT('Ctrl Pts',(32.5024778890101,1.49516703667321,-34.9680098521065));
#31604=CARTESIAN_POINT('Ctrl Pts',(32.5478477692433,1.49587895592537,-34.9679793561973));
#31605=CARTESIAN_POINT('Ctrl Pts',(32.5909873019015,1.49648137333635,-34.9679531603256));
#31606=CARTESIAN_POINT('Ctrl Pts',(32.6362425762323,1.49711333579668,-34.9679256796997));
#31607=CARTESIAN_POINT('Ctrl Pts',(32.6790438910161,1.49762527612468,-34.9679029082457));
#31608=CARTESIAN_POINT('Ctrl Pts',(32.7213614276283,1.49804900699202,-34.9678837287556));
#31609=CARTESIAN_POINT('Ctrl Pts',(32.7633326545664,1.49846927021662,-34.9678647062226));
#31610=CARTESIAN_POINT('Ctrl Pts',(32.8048283340736,1.49880319667879,-34.9678491963778));
#31611=CARTESIAN_POINT('Ctrl Pts',(32.8478112859666,1.49905168880696,-34.9678375791942));
#31612=CARTESIAN_POINT('Ctrl Pts',(32.8880595868492,1.49928437142881,-34.9678267011162));
#31613=CARTESIAN_POINT('Ctrl Pts',(32.9296120625659,1.49944259954574,-34.9678192143482));
#31614=CARTESIAN_POINT('Ctrl Pts',(32.9741124736877,1.49949475964765,-34.9678170031323));
#31615=CARTESIAN_POINT('Ctrl Pts',(32.9824658917628,1.49950455090861,-34.9678165880527));
#31616=CARTESIAN_POINT('Ctrl Pts',(32.9909232824633,1.49951049395371,-34.9678163642396));
#31617=CARTESIAN_POINT('Ctrl Pts',(32.9994956564547,1.4995122138931,-34.9678163521983));
#31618=CARTESIAN_POINT('Ctrl Pts',(33.035916707601,1.49951952132052,-34.9678163010392));
#31619=CARTESIAN_POINT('Ctrl Pts',(33.0737648470631,1.49952600456097,-34.9678163144541));
#31620=CARTESIAN_POINT('Ctrl Pts',(33.1138039348094,1.49953164904712,-34.9678165569182));
#31621=CARTESIAN_POINT('Ctrl Pts',(33.2457861392315,1.49955025515845,-34.9678173561608));
#31622=CARTESIAN_POINT('Ctrl Pts',(33.3718058092168,1.49955552940342,-34.9678177616075));
#31623=CARTESIAN_POINT('Ctrl Pts',(33.4990121011459,1.49956083536767,-34.9678181023247));
#31624=CARTESIAN_POINT('Ctrl Pts',(33.6624238693915,1.49956765151637,-34.9678185400169));
#31625=CARTESIAN_POINT('Ctrl Pts',(33.8277938592881,1.49957452000976,-34.9678188708891));
#31626=CARTESIAN_POINT('Ctrl Pts',(33.9926457806311,1.49958605843696,-34.9678194856962));
#31627=CARTESIAN_POINT('Ctrl Pts',(34.322349623317,1.49960913529134,-34.9678207153104));
#31628=CARTESIAN_POINT('Ctrl Pts',(34.649981191788,1.49965089188093,-34.9678230806641));
#31629=CARTESIAN_POINT('Ctrl Pts',(34.978743760729,1.499668413021,-34.9678240597269));
#31630=CARTESIAN_POINT('Ctrl Pts',(35.1431250451995,1.49967717359104,-34.9678245492582));
#31631=CARTESIAN_POINT('Ctrl Pts',(35.3077890797876,1.49967987529869,-34.9678246922169));
#31632=CARTESIAN_POINT('Ctrl Pts',(35.4723919953983,1.49968390458378,-34.9678249110675));
#31633=CARTESIAN_POINT('Ctrl Pts',(35.9662007422305,1.49969599243904,-34.9678255676192));
#31634=CARTESIAN_POINT('Ctrl Pts',(36.4594594182669,1.49972002849122,-34.9678269071982));
#31635=CARTESIAN_POINT('Ctrl Pts',(36.9527108273738,1.49975356610212,-34.9678287658476));
#31636=CARTESIAN_POINT('Ctrl Pts',(38.1015495523822,1.49983167901863,-34.9678330948538));
#31637=CARTESIAN_POINT('Ctrl Pts',(39.2503488559568,1.49996133572171,-34.9678402396984));
#31638=CARTESIAN_POINT('Ctrl Pts',(40.4000634893725,1.49999290859452,-34.9678419791559));
#31639=CARTESIAN_POINT('Ctrl Pts',(6.89999999997365,5.65979197164529,-9.46599415780712));
#31640=CARTESIAN_POINT('Ctrl Pts',(6.99168932310453,5.60729410195164,-9.49787619923353));
#31641=CARTESIAN_POINT('Ctrl Pts',(7.08406757664724,5.55450348934908,-9.52934743218563));
#31642=CARTESIAN_POINT('Ctrl Pts',(8.15335547176687,4.94393526084759,-9.88612718871467));
#31643=CARTESIAN_POINT('Ctrl Pts',(9.17064157978095,4.34950511965197,-10.155373368134));
#31644=CARTESIAN_POINT('Ctrl Pts',(11.2497073679685,3.24768323904103,-10.5680733268196));
#31645=CARTESIAN_POINT('Ctrl Pts',(12.2613257965134,2.71507134816794,-10.7096965195797));
#31646=CARTESIAN_POINT('Ctrl Pts',(14.3530385707896,1.75090834575261,-10.9182697262449));
#31647=CARTESIAN_POINT('Ctrl Pts',(15.3683954027039,1.30024059461546,-10.9736607960856));
#31648=CARTESIAN_POINT('Ctrl Pts',(17.4699663744738,0.511601148556842,-11.0479352514981));
#31649=CARTESIAN_POINT('Ctrl Pts',(18.4899687408706,0.154958649018866,-11.051850654124));
#31650=CARTESIAN_POINT('Ctrl Pts',(19.8459543561021,-0.227742125737042,
-11.0525070343707));
#31651=CARTESIAN_POINT('Ctrl Pts',(20.3436217075759,-0.364015941931448,
-11.0499451453311));
#31652=CARTESIAN_POINT('Ctrl Pts',(21.3765896493641,-0.626368709758944,
-11.0391193472025));
#31653=CARTESIAN_POINT('Ctrl Pts',(22.1786672894955,-0.801485129181549,
-11.0271785661492));
#31654=CARTESIAN_POINT('Ctrl Pts',(22.8524865110786,-0.927592368920619,
-11.0190187727781));
#31655=CARTESIAN_POINT('Ctrl Pts',(23.1034925219802,-0.973363366151912,
-11.0156366139706));
#31656=CARTESIAN_POINT('Ctrl Pts',(23.6153640104269,-1.06158199416384,-11.0082049867405));
#31657=CARTESIAN_POINT('Ctrl Pts',(24.2641052830132,-1.16309769090629,-10.9980910304789));
#31658=CARTESIAN_POINT('Ctrl Pts',(24.925223802488,-1.25113068226714,-10.9882977299783));
#31659=CARTESIAN_POINT('Ctrl Pts',(25.39243267008,-1.30426326836546,-10.9823394091471));
#31660=CARTESIAN_POINT('Ctrl Pts',(25.6607214646257,-1.33204812136028,-10.9792978116211));
#31661=CARTESIAN_POINT('Ctrl Pts',(25.7950851290472,-1.3450283872937,-10.9779152492989));
#31662=CARTESIAN_POINT('Ctrl Pts',(26.2512983640655,-1.38748632823361,-10.973504884093));
#31663=CARTESIAN_POINT('Ctrl Pts',(27.3073255991507,-1.45732001035815,-10.9653766251364));
#31664=CARTESIAN_POINT('Ctrl Pts',(28.3319095891359,-1.48237652410472,-10.9609947927216));
#31665=CARTESIAN_POINT('Ctrl Pts',(29.1279971548665,-1.50394615286608,-10.9582093263721));
#31666=CARTESIAN_POINT('Ctrl Pts',(29.4779663121082,-1.51103862156505,-10.9573325432847));
#31667=CARTESIAN_POINT('Ctrl Pts',(29.9466432965585,-1.51533372194798,-10.9567800734979));
#31668=CARTESIAN_POINT('Ctrl Pts',(30.4585813758454,-1.5163264007104,-10.9566567573898));
#31669=CARTESIAN_POINT('Ctrl Pts',(31.4732365826137,-1.51158267548692,-10.9572595410787));
#31670=CARTESIAN_POINT('Ctrl Pts',(32.3455737970013,-1.49995034482797,-10.9587933809202));
#31671=CARTESIAN_POINT('Ctrl Pts',(33.1628435364506,-1.49997381799307,-10.9587933913798));
#31672=CARTESIAN_POINT('Ctrl Pts',(33.4532364756742,-1.49997294893161,-10.9587933907408));
#31673=CARTESIAN_POINT('Ctrl Pts',(33.7813770806023,-1.49997567748037,-10.9587933918753));
#31674=CARTESIAN_POINT('Ctrl Pts',(34.275530783599,-1.49997630771875,-10.9587933920503));
#31675=CARTESIAN_POINT('Ctrl Pts',(34.810224248481,-1.49998265426638,-10.9587933943926));
#31676=CARTESIAN_POINT('Ctrl Pts',(35.6332393788981,-1.49998352671605,-10.9587933946975));
#31677=CARTESIAN_POINT('Ctrl Pts',(36.2915395642402,-1.49998521165682,-10.9587933953165));
#31678=CARTESIAN_POINT('Ctrl Pts',(38.1020088507064,-1.4999875244666,-10.9587933961529));
#31679=CARTESIAN_POINT('Ctrl Pts',(39.5833333333333,-1.5,-10.9587934006931));
#31680=CARTESIAN_POINT('Ctrl Pts',(40.9,-1.5,-10.9587934006931));
#31681=CARTESIAN_POINT('Ctrl Pts',(6.71972576838711,7.83711082411041,-12.1185747411757));
#31682=CARTESIAN_POINT('Ctrl Pts',(6.81144220747046,7.76982141889617,-12.1626853346856));
#31683=CARTESIAN_POINT('Ctrl Pts',(6.90386756592035,7.70211146561914,-12.206272355858));
#31684=CARTESIAN_POINT('Ctrl Pts',(7.97356860844392,6.9193341478531,-12.7007961961294));
#31685=CARTESIAN_POINT('Ctrl Pts',(8.99209675135677,6.15357612800253,-13.0797453577275));
#31686=CARTESIAN_POINT('Ctrl Pts',(11.0768095250715,4.72738288403858,-13.6699841865111));
#31687=CARTESIAN_POINT('Ctrl Pts',(12.0908998487774,4.03629416338865,-13.8792353432569));
#31688=CARTESIAN_POINT('Ctrl Pts',(14.1940249697802,2.77872196480346,-14.1957933847446));
#31689=CARTESIAN_POINT('Ctrl Pts',(15.2135111428103,2.19039552953479,-14.2882641966348));
#31690=CARTESIAN_POINT('Ctrl Pts',(17.3331413243803,1.15511424931918,-14.4203884130587));
#31691=CARTESIAN_POINT('Ctrl Pts',(18.3586247182578,0.687383264604317,-14.4409834784055));
#31692=CARTESIAN_POINT('Ctrl Pts',(19.7310977064191,0.182163287151178,-14.4582431367918));
#31693=CARTESIAN_POINT('Ctrl Pts',(20.2319281700692,0.00304050314957347,
-14.4607525000525));
#31694=CARTESIAN_POINT('Ctrl Pts',(21.2757193631683,-0.34316184167988,-14.4577287725711));
#31695=CARTESIAN_POINT('Ctrl Pts',(22.0878459668371,-0.574768167050975,
-14.4494235361695));
#31696=CARTESIAN_POINT('Ctrl Pts',(22.7712255558999,-0.741838037544796,
-14.4439791152719));
#31697=CARTESIAN_POINT('Ctrl Pts',(23.0244518575534,-0.802235623376846,
-14.4414745946824));
#31698=CARTESIAN_POINT('Ctrl Pts',(23.5421782294103,-0.918904682189656,
-14.4354166159132));
#31699=CARTESIAN_POINT('Ctrl Pts',(24.1985076923264,-1.05321891221311,-14.4263782772875));
#31700=CARTESIAN_POINT('Ctrl Pts',(24.8685349201902,-1.16990126309174,-14.4171649757332));
#31701=CARTESIAN_POINT('Ctrl Pts',(25.3425219397605,-1.24038895116693,-14.4115304423973));
#31702=CARTESIAN_POINT('Ctrl Pts',(25.6149132395532,-1.2772755062893,-14.4086772259669));
#31703=CARTESIAN_POINT('Ctrl Pts',(25.751350411375,-1.29451009974022,-14.4073941370215));
#31704=CARTESIAN_POINT('Ctrl Pts',(26.2150797233484,-1.35093461898509,-14.4033369558708));
#31705=CARTESIAN_POINT('Ctrl Pts',(27.290210767141,-1.44377946037276,-14.3955032503722));
#31706=CARTESIAN_POINT('Ctrl Pts',(28.3189127523345,-1.47663174833176,-14.3908275896983));
#31707=CARTESIAN_POINT('Ctrl Pts',(29.1160761436634,-1.50501177720119,-14.3880866255979));
#31708=CARTESIAN_POINT('Ctrl Pts',(29.4714822396865,-1.51444018285273,-14.3872233428149));
#31709=CARTESIAN_POINT('Ctrl Pts',(29.9435445757052,-1.5200984593836,-14.3866793881694));
#31710=CARTESIAN_POINT('Ctrl Pts',(30.4592512763238,-1.52141685888082,-14.3865579372846));
#31711=CARTESIAN_POINT('Ctrl Pts',(31.4783289771153,-1.51514975878901,-14.3871513993674));
#31712=CARTESIAN_POINT('Ctrl Pts',(32.3494109418822,-1.49991854815768,-14.3886610620144));
#31713=CARTESIAN_POINT('Ctrl Pts',(33.1623024290964,-1.49995704732011,-14.3886610002152));
#31714=CARTESIAN_POINT('Ctrl Pts',(33.4534378485101,-1.49995562308142,-14.3886610012865));
#31715=CARTESIAN_POINT('Ctrl Pts',(33.7812569880683,-1.49996009863815,-14.3886609937099));
#31716=CARTESIAN_POINT('Ctrl Pts',(34.2755369516761,-1.49996113279295,-14.3886609915395));
#31717=CARTESIAN_POINT('Ctrl Pts',(34.8101662657421,-1.49997154418691,-14.3886609724833));
#31718=CARTESIAN_POINT('Ctrl Pts',(35.6332120986579,-1.49997297550203,-14.3886609697809));
#31719=CARTESIAN_POINT('Ctrl Pts',(36.2915016928915,-1.49997573962884,-14.3886609647081));
#31720=CARTESIAN_POINT('Ctrl Pts',(38.1019871489809,-1.49997953382812,-14.3886609576808));
#31721=CARTESIAN_POINT('Ctrl Pts',(39.5833333333333,-1.5,-14.3886609199119));
#31722=CARTESIAN_POINT('Ctrl Pts',(40.9,-1.5,-14.3886609199119));
#31723=CARTESIAN_POINT('Ctrl Pts',(6.48179127333656,12.909089854674,-18.3143700731402));
#31724=CARTESIAN_POINT('Ctrl Pts',(6.5727355112717,12.8079669208388,-18.3863503069792));
#31725=CARTESIAN_POINT('Ctrl Pts',(6.66430583051619,12.7062136474361,-18.4575107126117));
#31726=CARTESIAN_POINT('Ctrl Pts',(7.72728755127275,11.526813643454,-19.2683717061286));
#31727=CARTESIAN_POINT('Ctrl Pts',(8.73767093241514,10.3681062987579,-19.8994793964433));
#31728=CARTESIAN_POINT('Ctrl Pts',(10.8072764746652,8.20052377414071,-20.8976754072823));
#31729=CARTESIAN_POINT('Ctrl Pts',(11.8176293289991,7.14335535654034,-21.2648595585571));
#31730=CARTESIAN_POINT('Ctrl Pts',(13.9143877357634,5.21126000157089,-21.8327192432693));
#31731=CARTESIAN_POINT('Ctrl Pts',(14.9340995606326,4.30265046255494,-22.0133279182349));
#31732=CARTESIAN_POINT('Ctrl Pts',(17.0643846051769,2.69212316987972,-22.28293018524));
#31733=CARTESIAN_POINT('Ctrl Pts',(18.0954552433595,1.9632331485467,-22.3440950085561));
#31734=CARTESIAN_POINT('Ctrl Pts',(19.4909197138958,1.16629947063494,-22.4018170797765));
#31735=CARTESIAN_POINT('Ctrl Pts',(19.9966086695085,0.886002865969556,-22.4166274395865));
#31736=CARTESIAN_POINT('Ctrl Pts',(21.057536308733,0.34008676046798,-22.4327717472399));
#31737=CARTESIAN_POINT('Ctrl Pts',(21.8881436826395,-0.0273249680472169,
-22.4335301553629));
#31738=CARTESIAN_POINT('Ctrl Pts',(22.5903109281612,-0.293403230880334,
-22.4347813300338));
#31739=CARTESIAN_POINT('Ctrl Pts',(22.8479490471753,-0.388703666414858,
-22.4344227430831));
#31740=CARTESIAN_POINT('Ctrl Pts',(23.3775020106794,-0.573741554000536,
-22.4317625870076));
#31741=CARTESIAN_POINT('Ctrl Pts',(24.0496637775493,-0.786975429601204,
-22.4254188817567));
#31742=CARTESIAN_POINT('Ctrl Pts',(24.7388948303246,-0.97298069201505,-22.4176871558595));
#31743=CARTESIAN_POINT('Ctrl Pts',(25.2278255076836,-1.08558489693713,-22.4128668811674));
#31744=CARTESIAN_POINT('Ctrl Pts',(25.5093513414538,-1.14461019857633,-22.4104803100082));
#31745=CARTESIAN_POINT('Ctrl Pts',(25.65043215624,-1.17219731393412,-22.4094403330887));
#31746=CARTESIAN_POINT('Ctrl Pts',(26.1310661693221,-1.26270961274929,-22.4062434753127));
#31747=CARTESIAN_POINT('Ctrl Pts',(27.2501415560404,-1.41179466704418,-22.3991278521003));
#31748=CARTESIAN_POINT('Ctrl Pts',(28.2886032423041,-1.46273606147739,-22.3937640305132));
#31749=CARTESIAN_POINT('Ctrl Pts',(29.0882604747173,-1.50713395382423,-22.3911301380753));
#31750=CARTESIAN_POINT('Ctrl Pts',(29.4563322715989,-1.52226638583168,-22.3902983022162));
#31751=CARTESIAN_POINT('Ctrl Pts',(29.9362980190428,-1.53114557872188,-22.3897746111047));
#31752=CARTESIAN_POINT('Ctrl Pts',(30.4607981263299,-1.53325643249715,-22.3896576468515));
#31753=CARTESIAN_POINT('Ctrl Pts',(31.4901962393228,-1.52335038033792,-22.3902297218138));
#31754=CARTESIAN_POINT('Ctrl Pts',(32.3583565740134,-1.49981123516845,-22.3916842973338));
#31755=CARTESIAN_POINT('Ctrl Pts',(33.1610357599842,-1.49990048269241,-22.3916846791414));
#31756=CARTESIAN_POINT('Ctrl Pts',(33.4539035041348,-1.49989717526718,-22.3916846678314));
#31757=CARTESIAN_POINT('Ctrl Pts',(33.7809729803152,-1.49990754848558,-22.3916847131259));
#31758=CARTESIAN_POINT('Ctrl Pts',(34.2755476513316,-1.49990994339324,-22.3916847245643));
#31759=CARTESIAN_POINT('Ctrl Pts',(34.8100282687525,-1.49993406756257,-22.3916848332468));
#31760=CARTESIAN_POINT('Ctrl Pts',(35.6331458770731,-1.49993738365807,-22.3916848483796));
#31761=CARTESIAN_POINT('Ctrl Pts',(36.2914110212366,-1.49994378833294,-22.391684877265));
#31762=CARTESIAN_POINT('Ctrl Pts',(38.1019345670508,-1.49995257945083,-22.3916849170636));
#31763=CARTESIAN_POINT('Ctrl Pts',(39.5833333333333,-1.5,-22.3916851314225));
#31764=CARTESIAN_POINT('Ctrl Pts',(40.9,-1.5,-22.3916851314225));
#31765=CARTESIAN_POINT('Ctrl Pts',(6.40644620858992,17.8874643710144,-24.5816667734855));
#31766=CARTESIAN_POINT('Ctrl Pts',(6.49686818484384,17.7527429476115,-24.6805587856898));
#31767=CARTESIAN_POINT('Ctrl Pts',(6.58784510136317,17.6172881830822,-24.7782796712625));
#31768=CARTESIAN_POINT('Ctrl Pts',(7.64659115698292,16.0421679652612,-25.8957117993605));
#31769=CARTESIAN_POINT('Ctrl Pts',(8.6514045236879,14.4950741541975,-26.7687295114656));
#31770=CARTESIAN_POINT('Ctrl Pts',(10.7050090174743,11.6047165303877,-28.1553288871656));
#31771=CARTESIAN_POINT('Ctrl Pts',(11.7100667319376,10.1884238311836,-28.6739187260774));
#31772=CARTESIAN_POINT('Ctrl Pts',(13.7869442940535,7.60965076371051,-29.4789383477456));
#31773=CARTESIAN_POINT('Ctrl Pts',(14.800547377598,6.38969931376494,-29.7443143884371));
#31774=CARTESIAN_POINT('Ctrl Pts',(16.9119018452747,4.23153286849663,-30.1445946231782));
#31775=CARTESIAN_POINT('Ctrl Pts',(17.9381035625226,3.24834169632011,-30.2457831733189));
#31776=CARTESIAN_POINT('Ctrl Pts',(19.3293046497141,2.1696711131215,-30.3432573890378));
#31777=CARTESIAN_POINT('Ctrl Pts',(19.834780983011,1.78946315727512,-30.3704921110681));
#31778=CARTESIAN_POINT('Ctrl Pts',(20.8961305093701,1.0472327615649,-30.4059869321106));
#31779=CARTESIAN_POINT('Ctrl Pts',(21.7315172578668,0.543887046860907,-30.4162256374442));
#31780=CARTESIAN_POINT('Ctrl Pts',(22.4417821405951,0.177022257580511,-30.4244987232164));
#31781=CARTESIAN_POINT('Ctrl Pts',(22.7014733500986,0.0463161543317088,
-30.4263999272521));
#31782=CARTESIAN_POINT('Ctrl Pts',(23.2370081907225,-0.208619908910742,
-30.4273647052435));
#31783=CARTESIAN_POINT('Ctrl Pts',(23.9184639528738,-0.503259137524155,
-30.4239702414859));
#31784=CARTESIAN_POINT('Ctrl Pts',(24.6208764942963,-0.761940486000404,
-30.4179198546273));
#31785=CARTESIAN_POINT('Ctrl Pts',(25.1213019205202,-0.91928494098934,-30.4140183351927));
#31786=CARTESIAN_POINT('Ctrl Pts',(25.4101854930952,-1.00200491165304,-30.4121479536513));
#31787=CARTESIAN_POINT('Ctrl Pts',(25.5551212201431,-1.04071255367786,-30.4113724623503));
#31788=CARTESIAN_POINT('Ctrl Pts',(26.0499700309764,-1.16807884822144,-30.4091032350971));
#31789=CARTESIAN_POINT('Ctrl Pts',(27.2099838300809,-1.37887073252529,-30.4027650251877));
#31790=CARTESIAN_POINT('Ctrl Pts',(28.2587071867247,-1.44776855241709,-30.3967001628547));
#31791=CARTESIAN_POINT('Ctrl Pts',(29.0606747532772,-1.50844446424265,-30.3941758184157));
#31792=CARTESIAN_POINT('Ctrl Pts',(29.4413133039643,-1.52986784607282,-30.3933750220959));
#31793=CARTESIAN_POINT('Ctrl Pts',(29.9291749316176,-1.54205805667022,-30.3928713041225));
#31794=CARTESIAN_POINT('Ctrl Pts',(30.4624577144424,-1.54503525729536,-30.3927586652121));
#31795=CARTESIAN_POINT('Ctrl Pts',(31.5021663454747,-1.53129124555949,-30.3933094956308));
#31796=CARTESIAN_POINT('Ctrl Pts',(32.3673500494201,-1.4996392507279,-30.3947081079589));
#31797=CARTESIAN_POINT('Ctrl Pts',(33.1597959712394,-1.49981015578451,-30.394708675703));
#31798=CARTESIAN_POINT('Ctrl Pts',(33.4543964419649,-1.49980374442732,-30.3947086583173));
#31799=CARTESIAN_POINT('Ctrl Pts',(33.780713697117,-1.49982358355628,-30.3947087254864));
#31800=CARTESIAN_POINT('Ctrl Pts',(34.2755823554681,-1.49982813702183,-30.3947087422566));
#31801=CARTESIAN_POINT('Ctrl Pts',(34.809907886371,-1.49987418368373,-30.3947089027709));
#31802=CARTESIAN_POINT('Ctrl Pts',(35.6330963662039,-1.49988050793533,-30.3947089250841));
#31803=CARTESIAN_POINT('Ctrl Pts',(36.2913353597009,-1.49989273190318,-30.3947089677392));
#31804=CARTESIAN_POINT('Ctrl Pts',(38.1018946411375,-1.49990950652165,-30.3947090264815));
#31805=CARTESIAN_POINT('Ctrl Pts',(39.5833333333333,-1.50000000000001,-30.3947093429332));
#31806=CARTESIAN_POINT('Ctrl Pts',(40.9,-1.50000000000001,-30.3947093429332));
#31807=CARTESIAN_POINT('Ctrl Pts',(6.37427268165564,20.7176664141567,-28.1741189428499));
#31808=CARTESIAN_POINT('Ctrl Pts',(6.46448755772839,20.5636424771022,-28.2883460540946));
#31809=CARTESIAN_POINT('Ctrl Pts',(6.55522920065044,20.4088241438424,-28.4012016037216));
#31810=CARTESIAN_POINT('Ctrl Pts',(7.61218358683609,18.6066930771539,-29.6930901664144));
#31811=CARTESIAN_POINT('Ctrl Pts',(8.61458966533695,16.8369834746305,-30.7034878418583));
#31812=CARTESIAN_POINT('Ctrl Pts',(10.6617286949536,13.5326707735154,-32.3103185106199));
#31813=CARTESIAN_POINT('Ctrl Pts',(11.6645299641072,11.9110262048008,-32.9144286242224));
#31814=CARTESIAN_POINT('Ctrl Pts',(13.7331354874437,8.96388086964109,-33.8529305432337));
#31815=CARTESIAN_POINT('Ctrl Pts',(14.7439974349565,7.56674273992029,-34.1658034093158));
#31816=CARTESIAN_POINT('Ctrl Pts',(16.8461293839489,5.10010790554499,-34.6388295936079));
#31817=CARTESIAN_POINT('Ctrl Pts',(17.869539668257,3.97330758910436,-34.7622699672013));
#31818=CARTESIAN_POINT('Ctrl Pts',(19.2561499197764,2.73819527916447,-34.8817370116275));
#31819=CARTESIAN_POINT('Ctrl Pts',(19.7609682985244,2.30174976258002,-34.9159236099686));
#31820=CARTESIAN_POINT('Ctrl Pts',(20.8205490930365,1.45014125059819,-34.962142837607));
#31821=CARTESIAN_POINT('Ctrl Pts',(21.6560398772552,0.871063560332534,-34.9776921520547));
#31822=CARTESIAN_POINT('Ctrl Pts',(22.3683071131494,0.447764459080894,-34.9899406319134));
#31823=CARTESIAN_POINT('Ctrl Pts',(22.628558263498,0.297072507988388,-34.9931292198003));
#31824=CARTESIAN_POINT('Ctrl Pts',(23.1658987323054,0.00272021601686333,
-34.9961615195562));
#31825=CARTESIAN_POINT('Ctrl Pts',(23.8506336743687,-0.338080815637156,
-34.9944685164155));
#31826=CARTESIAN_POINT('Ctrl Pts',(24.5584297298735,-0.638330240963619,
-34.9894063813143));
#31827=CARTESIAN_POINT('Ctrl Pts',(25.0640452406954,-0.821508451465936,
-34.9860482895808));
#31828=CARTESIAN_POINT('Ctrl Pts',(25.3563918473524,-0.917987033927376,
-34.9844827679614));
#31829=CARTESIAN_POINT('Ctrl Pts',(25.5031889952515,-0.963173610848517,
-34.9838627756015));
#31830=CARTESIAN_POINT('Ctrl Pts',(26.004987441878,-1.11209942724697,-34.9821396575606));
#31831=CARTESIAN_POINT('Ctrl Pts',(27.1869158502136,-1.35964566982755,-34.9762669195668));
#31832=CARTESIAN_POINT('Ctrl Pts',(28.241775526507,-1.43886068581106,-34.9698005674756));
#31833=CARTESIAN_POINT('Ctrl Pts',(29.0449901822568,-1.50891651433762,-34.967341499596));
#31834=CARTESIAN_POINT('Ctrl Pts',(29.4327578078034,-1.53412418433924,-34.9665584285133));
#31835=CARTESIAN_POINT('Ctrl Pts',(29.9251326248081,-1.54823778132882,-34.9660664877723));
#31836=CARTESIAN_POINT('Ctrl Pts',(30.4634303371364,-1.55173467727118,-34.9659564517225));
#31837=CARTESIAN_POINT('Ctrl Pts',(31.5090284502475,-1.53573375297651,-34.9664954568879));
#31838=CARTESIAN_POINT('Ctrl Pts',(32.3724987732541,-1.49951478355662,-34.9678633280106));
#31839=CARTESIAN_POINT('Ctrl Pts',(33.1590931275331,-1.49974473197886,-34.9678645639232));
#31840=CARTESIAN_POINT('Ctrl Pts',(33.4546837514055,-1.49973608826798,-34.96786452809));
#31841=CARTESIAN_POINT('Ctrl Pts',(33.780570662352,-1.49976277569534,-34.9678646749597));
#31842=CARTESIAN_POINT('Ctrl Pts',(34.275607154309,-1.49976889496147,-34.9678647123124));
#31843=CARTESIAN_POINT('Ctrl Pts',(34.8098427469218,-1.4998308160265,-34.9678650656176));
#31844=CARTESIAN_POINT('Ctrl Pts',(35.6330715352155,-1.49983931935013,-34.9678651148618));
#31845=CARTESIAN_POINT('Ctrl Pts',(36.291295234337,-1.49985575728851,-34.9678652087707));
#31846=CARTESIAN_POINT('Ctrl Pts',(38.1018744475862,-1.49987831370054,-34.9678653381985));
#31847=CARTESIAN_POINT('Ctrl Pts',(39.5833333333333,-1.50000000000001,-34.9678660352249));
#31848=CARTESIAN_POINT('Ctrl Pts',(40.9,-1.50000000000001,-34.9678660352249));
#31849=CARTESIAN_POINT('',(40.9,-1.50000000000002,-32.9658914637539));
#31850=CARTESIAN_POINT('Ctrl Pts',(40.9,-1.50000000000002,-32.9658914637539));
#31851=CARTESIAN_POINT('Ctrl Pts',(40.9,-1.50000000000002,-33.466386268912));
#31852=CARTESIAN_POINT('Ctrl Pts',(40.9,-1.50000000000002,-33.9668810740701));
#31853=CARTESIAN_POINT('Ctrl Pts',(40.9,-1.50000000000002,-34.4673758792282));
#31854=CARTESIAN_POINT('',(38.,-1.5,-32.9658914637539));
#31855=CARTESIAN_POINT('Ctrl Pts',(38.,-1.50000000000001,-32.9658914637539));
#31856=CARTESIAN_POINT('Ctrl Pts',(38.9666666666667,-1.50000000000001,-32.9658914637539));
#31857=CARTESIAN_POINT('Ctrl Pts',(39.9333333333333,-1.50000000000001,-32.9658914637539));
#31858=CARTESIAN_POINT('Ctrl Pts',(40.9,-1.50000000000001,-32.9658914637539));
#31859=CARTESIAN_POINT('Ctrl Pts',(37.499759314198,-1.49989731090857,-32.3652586491488));
#31860=CARTESIAN_POINT('Ctrl Pts',(37.6667177862607,-1.49990104941725,-32.5658057373987));
#31861=CARTESIAN_POINT('Ctrl Pts',(37.8334339226403,-1.49990571638763,-32.7660568899056));
#31862=CARTESIAN_POINT('Ctrl Pts',(37.9998061672102,-1.49991103444899,-32.9658910126336));
#31863=CARTESIAN_POINT('',(6.9,16.9192021366758,-24.7737885487526));
#31864=CARTESIAN_POINT('Ctrl Pts',(6.9,16.9192021366758,-24.7737885487526));
#31865=CARTESIAN_POINT('Ctrl Pts',(6.9,15.3881766950258,-22.645444622876));
#31866=CARTESIAN_POINT('Ctrl Pts',(6.90000000000115,13.8353835251886,-20.4978726403359));
#31867=CARTESIAN_POINT('Ctrl Pts',(6.90000000000115,10.3082122779765,-15.662481608859));
#31868=CARTESIAN_POINT('Ctrl Pts',(6.9,7.95935811114668,-12.4764228571341));
#31869=CARTESIAN_POINT('Ctrl Pts',(6.9,5.6597919716369,-9.46599415782505));
#31870=CARTESIAN_POINT('',(22.9245129145126,-5.83616550085653E-15,-31.7706052331164));
#31871=CARTESIAN_POINT('Ctrl Pts',(22.9245129145126,-9.86197306871846E-15,
-31.7706052331164));
#31872=CARTESIAN_POINT('Ctrl Pts',(22.7202811020963,0.0979233563002592,
-31.7014549124251));
#31873=CARTESIAN_POINT('Ctrl Pts',(22.5089075447093,0.203440182623867,-31.6320805544326));
#31874=CARTESIAN_POINT('Ctrl Pts',(22.2913349439917,0.316637134194161,-31.5632247707622));
#31875=CARTESIAN_POINT('Ctrl Pts',(21.4451770585292,0.756869465221163,-31.2954389184984));
#31876=CARTESIAN_POINT('Ctrl Pts',(20.5220951556668,1.35418571023225,-31.0475106147151));
#31877=CARTESIAN_POINT('Ctrl Pts',(19.7671428819538,1.89915402350704,-30.8612920963158));
#31878=CARTESIAN_POINT('Ctrl Pts',(19.5194773058391,2.07793339270832,-30.8002022522972));
#31879=CARTESIAN_POINT('Ctrl Pts',(19.2865716386091,2.25204835959322,-30.7444068279678));
#31880=CARTESIAN_POINT('Ctrl Pts',(19.0728538401323,2.41532203906683,-30.6939488833522));
#31881=CARTESIAN_POINT('Ctrl Pts',(18.7028555998036,2.69798906318807,-30.6065937315988));
#31882=CARTESIAN_POINT('Ctrl Pts',(18.4144703596236,2.93373938287709,-30.539966063932));
#31883=CARTESIAN_POINT('Ctrl Pts',(18.0642874871539,3.23398234069978,-30.4582462938821));
#31884=CARTESIAN_POINT('Ctrl Pts',(17.4420927116722,3.76744532366909,-30.3130489756353));
#31885=CARTESIAN_POINT('Ctrl Pts',(16.7224564418219,4.43872907330225,-30.1446863488622));
#31886=CARTESIAN_POINT('Ctrl Pts',(15.9202806616111,5.24401550821528,-29.9321297384067));
#31887=CARTESIAN_POINT('Ctrl Pts',(15.4090529834523,5.75722561070076,-29.7966671314305));
#31888=CARTESIAN_POINT('Ctrl Pts',(14.8739602945724,6.33424649579561,-29.6418940055918));
#31889=CARTESIAN_POINT('Ctrl Pts',(14.3169794331169,6.96996102647052,-29.4557634846127));
#31890=CARTESIAN_POINT('Ctrl Pts',(13.8864206762846,7.46138268378274,-29.3118803976572));
#31891=CARTESIAN_POINT('Ctrl Pts',(13.386789002781,8.05270459511923,-29.1311705407941));
#31892=CARTESIAN_POINT('Ctrl Pts',(12.8146824059514,8.75043091662867,-28.8915984033895));
#31893=CARTESIAN_POINT('Ctrl Pts',(12.2526665517594,9.43585083093896,-28.6562518085588));
#31894=CARTESIAN_POINT('Ctrl Pts',(11.6379478462803,10.2313662767681,-28.3625845909802));
#31895=CARTESIAN_POINT('Ctrl Pts',(10.9739250490307,11.1267230319108,-27.9810212930959));
#31896=CARTESIAN_POINT('Ctrl Pts',(10.5683455447962,11.6735993596029,-27.7479656603209));
#31897=CARTESIAN_POINT('Ctrl Pts',(10.1437415406955,12.2581093618547,-27.4801235315866));
#31898=CARTESIAN_POINT('Ctrl Pts',(9.74137929176524,12.8142541611144,-27.2046666925187));
#31899=CARTESIAN_POINT('Ctrl Pts',(8.72285779294233,14.2220538143138,-26.5073877769786));
#31900=CARTESIAN_POINT('Ctrl Pts',(7.81323138778195,15.580948814124,-25.7100913255874));
#31901=CARTESIAN_POINT('Ctrl Pts',(6.9,16.9192021366758,-24.7737885487526));
#31902=CARTESIAN_POINT('Ctrl Pts',(30.5,-1.55029606206997,-34.9656486014478));
#31903=CARTESIAN_POINT('Ctrl Pts',(29.9560179420817,-1.55343104498103,-34.7222276068062));
#31904=CARTESIAN_POINT('Ctrl Pts',(29.4152668325132,-1.54030953139106,-34.4790656554127));
#31905=CARTESIAN_POINT('Ctrl Pts',(28.8740459957565,-1.49470250846617,-34.2361296888632));
#31906=CARTESIAN_POINT('Ctrl Pts',(28.3535277923439,-1.45084003307051,-34.0024864433252));
#31907=CARTESIAN_POINT('Ctrl Pts',(27.8179515912466,-1.40923473841146,-33.7608540997398));
#31908=CARTESIAN_POINT('Ctrl Pts',(27.2695051149491,-1.33972398862117,-33.5168388499063));
#31909=CARTESIAN_POINT('Ctrl Pts',(26.9554553615883,-1.29992095446743,-33.3771115796287));
#31910=CARTESIAN_POINT('Ctrl Pts',(26.6378099296971,-1.25106463707209,-33.2369493090937));
#31911=CARTESIAN_POINT('Ctrl Pts',(26.3179304017917,-1.18777049128279,-33.0983258448229));
#31912=CARTESIAN_POINT('Ctrl Pts',(26.1078196745982,-1.14619615520082,-33.0072719500184));
#31913=CARTESIAN_POINT('Ctrl Pts',(25.8967402232745,-1.09839525532295,-32.9168907470981));
#31914=CARTESIAN_POINT('Ctrl Pts',(25.6850706236774,-1.04282885388103,-32.8277596053404));
#31915=CARTESIAN_POINT('Ctrl Pts',(25.6562210027417,-1.03525540156945,-32.8156114288513));
#31916=CARTESIAN_POINT('Ctrl Pts',(25.6277737638215,-1.0276506122434,-32.8036595933923));
#31917=CARTESIAN_POINT('Ctrl Pts',(25.5983858063598,-1.01964325944537,-32.7913423709803));
#31918=CARTESIAN_POINT('Ctrl Pts',(25.1249357452756,-0.890642063078177,
-32.5929076988546));
#31919=CARTESIAN_POINT('Ctrl Pts',(24.1510084067019,-0.588069770626608,
-32.1858811669087));
#31920=CARTESIAN_POINT('Ctrl Pts',(22.9245129145126,-9.86197306871846E-15,
-31.7706052331164));
#31921=CARTESIAN_POINT('Origin',(40.65,0.,0.));
#31922=CARTESIAN_POINT('',(40.4,18.7829592905825,-29.5330398077868));
#31923=CARTESIAN_POINT('',(40.9,18.5327260452907,-29.0996231131986));
#31924=CARTESIAN_POINT('Ctrl Pts',(40.4,18.7829592905825,-29.5330398077868));
#31925=CARTESIAN_POINT('Ctrl Pts',(40.5666590140292,18.699553150888,-29.3885761361728));
#31926=CARTESIAN_POINT('Ctrl Pts',(40.7333430452231,18.616133394895,-29.2440888804379));
#31927=CARTESIAN_POINT('Ctrl Pts',(40.9,18.5327260452907,-29.0996231131986));
#31928=CARTESIAN_POINT('',(40.9,15.9346498339374,-30.5996231131986));
#31929=CARTESIAN_POINT('Origin',(40.9,0.,0.));
#31930=CARTESIAN_POINT('',(40.4,16.1848830792292,-31.0330398077868));
#31931=CARTESIAN_POINT('Ctrl Pts',(40.9,15.9346498339374,-30.5996231131986));
#31932=CARTESIAN_POINT('Ctrl Pts',(40.7333430442937,16.0180571840068,-30.7440888812435));
#31933=CARTESIAN_POINT('Ctrl Pts',(40.5666590123859,16.1014769403571,-30.8885761375972));
#31934=CARTESIAN_POINT('Ctrl Pts',(40.4,16.1848830792292,-31.0330398077868));
#31935=CARTESIAN_POINT('Origin',(40.4,0.,0.));
#31936=CARTESIAN_POINT('Origin',(35.7,0.,0.));
#31937=CARTESIAN_POINT('',(30.5,16.1402285275843,-31.0562879796886));
#31938=CARTESIAN_POINT('Ctrl Pts',(40.3999012894849,16.1848928782182,-31.0330346270951));
#31939=CARTESIAN_POINT('Ctrl Pts',(39.2494626810401,16.1849362443212,-31.0330116996609));
#31940=CARTESIAN_POINT('Ctrl Pts',(38.0976708836828,16.1851115327779,-31.0329190263647));
#31941=CARTESIAN_POINT('Ctrl Pts',(36.9467340384723,16.1851746119074,-31.0328856894588));
#31942=CARTESIAN_POINT('Ctrl Pts',(36.745427730736,16.1851856448556,-31.032879858618));
#31943=CARTESIAN_POINT('Ctrl Pts',(36.5441475779313,16.1851932450653,-31.0328758430125));
#31944=CARTESIAN_POINT('Ctrl Pts',(36.3429119519248,16.1852000001162,-31.0328722727086));
#31945=CARTESIAN_POINT('Ctrl Pts',(36.2102758775794,16.1852044524265,-31.0328699194916));
#31946=CARTESIAN_POINT('Ctrl Pts',(36.0822774296293,16.1852084224022,-31.0328678560427));
#31947=CARTESIAN_POINT('Ctrl Pts',(35.9587202262686,16.1852125810273,-31.0328657167445));
#31948=CARTESIAN_POINT('Ctrl Pts',(35.7925662245335,16.1852181733537,-31.0328628399153));
#31949=CARTESIAN_POINT('Ctrl Pts',(35.6344388155487,16.1852241162452,-31.0328598211429));
#31950=CARTESIAN_POINT('Ctrl Pts',(35.483771446345,16.1852312078525,-31.032856216152));
#31951=CARTESIAN_POINT('Ctrl Pts',(35.3175474553568,16.1852390316786,-31.0328522389407));
#31952=CARTESIAN_POINT('Ctrl Pts',(35.1604041224798,16.1852482463284,-31.0328475520712));
#31953=CARTESIAN_POINT('Ctrl Pts',(35.0116427948666,16.1852592402396,-31.0328419178902));
#31954=CARTESIAN_POINT('Ctrl Pts',(34.9979272091136,16.1852602538628,-31.0328413984267));
#31955=CARTESIAN_POINT('Ctrl Pts',(34.9842829110367,16.1852612822246,-31.0328408711132));
#31956=CARTESIAN_POINT('Ctrl Pts',(34.9707093736272,16.1852623254083,-31.0328403358797));
#31957=CARTESIAN_POINT('Ctrl Pts',(34.8522491799023,16.1852714295753,-31.0328356647415));
#31958=CARTESIAN_POINT('Ctrl Pts',(34.7391835006529,16.1852816068676,-31.0328304196803));
#31959=CARTESIAN_POINT('Ctrl Pts',(34.6312849042887,16.1852915612822,-31.0328252639047));
#31960=CARTESIAN_POINT('Ctrl Pts',(34.5096795260851,16.1853027802452,-31.0328194531708));
#31961=CARTESIAN_POINT('Ctrl Pts',(34.3946370581326,16.1853137193614,-31.0328137541413));
#31962=CARTESIAN_POINT('Ctrl Pts',(34.2857585821188,16.1853233495613,-31.0328086821746));
#31963=CARTESIAN_POINT('Ctrl Pts',(34.1786801908151,16.1853328205454,-31.0328036940625));
#31964=CARTESIAN_POINT('Ctrl Pts',(34.0775620514827,16.185341043166,-31.0327993031901));
#31965=CARTESIAN_POINT('Ctrl Pts',(33.9819758246427,16.1853475980775,-31.0327957057953));
#31966=CARTESIAN_POINT('Ctrl Pts',(33.9184449689727,16.1853519547631,-31.0327933148067));
#31967=CARTESIAN_POINT('Ctrl Pts',(33.8573517602305,16.1853555977386,-31.0327912624254));
#31968=CARTESIAN_POINT('Ctrl Pts',(33.7984399511826,16.1853587887284,-31.0327894081824));
#31969=CARTESIAN_POINT('Ctrl Pts',(33.7337970612213,16.1853622901452,-31.0327873735543));
#31970=CARTESIAN_POINT('Ctrl Pts',(33.6717809742681,16.1853652470741,-31.0327855776265));
#31971=CARTESIAN_POINT('Ctrl Pts',(33.6121191806454,16.1853678991827,-31.0327838881567));
#31972=CARTESIAN_POINT('Ctrl Pts',(33.5695978710648,16.1853697893561,-31.0327826840617));
#31973=CARTESIAN_POINT('Ctrl Pts',(33.5282738752657,16.1853715223629,-31.0327815352149));
#31974=CARTESIAN_POINT('Ctrl Pts',(33.4880643388298,16.1853731585247,-31.032780407062));
#31975=CARTESIAN_POINT('Ctrl Pts',(33.4508270573206,16.1853746737428,-31.0327793623013));
#31976=CARTESIAN_POINT('Ctrl Pts',(33.4145509216558,16.1853761126591,-31.0327783314862));
#31977=CARTESIAN_POINT('Ctrl Pts',(33.3793439789548,16.1853777420672,-31.0327771639657));
#31978=CARTESIAN_POINT('Ctrl Pts',(33.3411337035362,16.1853795104722,-31.0327758968498));
#31979=CARTESIAN_POINT('Ctrl Pts',(33.3041826660689,16.1853815029502,-31.0327744688781));
#31980=CARTESIAN_POINT('Ctrl Pts',(33.2685652776782,16.1853839484229,-31.0327727495066));
#31981=CARTESIAN_POINT('Ctrl Pts',(33.231009447455,16.1853865269881,-31.0327709365599));
#31982=CARTESIAN_POINT('Ctrl Pts',(33.1949357943681,16.185389608116,-31.0327688002292));
#31983=CARTESIAN_POINT('Ctrl Pts',(33.1603699172393,16.1853933524012,-31.0327662471215));
#31984=CARTESIAN_POINT('Ctrl Pts',(33.1223715679419,16.1853974685027,-31.0327634404841));
#31985=CARTESIAN_POINT('Ctrl Pts',(33.0861949166477,16.1854023852333,-31.0327601306123));
#31986=CARTESIAN_POINT('Ctrl Pts',(33.0518089354075,16.1854082033113,-31.0327562557942));
#31987=CARTESIAN_POINT('Ctrl Pts',(33.034103081306,16.1854111991264,-31.0327542605926));
#31988=CARTESIAN_POINT('Ctrl Pts',(33.0168710360022,16.1854144322605,-31.032752116523));
#31989=CARTESIAN_POINT('Ctrl Pts',(33.0001033802535,16.1854179076007,-31.0327498200704));
#31990=CARTESIAN_POINT('Ctrl Pts',(32.9420348133412,16.1854299431543,-31.0327418671573));
#31991=CARTESIAN_POINT('Ctrl Pts',(32.8874145324497,16.1852296143113,-31.0328461364757));
#31992=CARTESIAN_POINT('Ctrl Pts',(32.8357863520582,16.1849068811705,-31.0330149777623));
#31993=CARTESIAN_POINT('Ctrl Pts',(32.7779739682632,16.1845454899291,-31.0332040434467));
#31994=CARTESIAN_POINT('Ctrl Pts',(32.7239136589684,16.1840302574575,-31.0334742654593));
#31995=CARTESIAN_POINT('Ctrl Pts',(32.6729278684753,16.1834371021678,-31.033785409572));
#31996=CARTESIAN_POINT('Ctrl Pts',(32.6180801336262,16.1827990180322,-31.0341201214522));
#31997=CARTESIAN_POINT('Ctrl Pts',(32.5667902508433,16.1820699950121,-31.0345025939175));
#31998=CARTESIAN_POINT('Ctrl Pts',(32.5181731636799,16.1812992842338,-31.034906696383));
#31999=CARTESIAN_POINT('Ctrl Pts',(32.4659536029866,16.1804714646211,-31.0353407424038));
#32000=CARTESIAN_POINT('Ctrl Pts',(32.4168175136243,16.1795947944396,-31.0358001425894));
#32001=CARTESIAN_POINT('Ctrl Pts',(32.3696233879005,16.1786925325961,-31.0362725138779));
#32002=CARTESIAN_POINT('Ctrl Pts',(32.3182581618423,16.1777105272545,-31.0367866341767));
#32003=CARTESIAN_POINT('Ctrl Pts',(32.2691934412637,16.1766975364928,-31.0373164741889));
#32004=CARTESIAN_POINT('Ctrl Pts',(32.2209064724814,16.1756521425246,-31.0378627004434));
#32005=CARTESIAN_POINT('Ctrl Pts',(32.1715370438637,16.1745833137247,-31.0384211715746));
#32006=CARTESIAN_POINT('Ctrl Pts',(32.1229805798595,16.173479840102,-31.0389971805319));
#32007=CARTESIAN_POINT('Ctrl Pts',(32.0735591134775,16.1723205501866,-31.039601856364));
#32008=CARTESIAN_POINT('Ctrl Pts',(32.0254239419637,16.1711914331653,-31.0401907942693));
#32009=CARTESIAN_POINT('Ctrl Pts',(31.9764682879407,16.1700086968176,-31.0408072809901));
#32010=CARTESIAN_POINT('Ctrl Pts',(31.9250947921519,16.1687449477338,-31.041465759884));
#32011=CARTESIAN_POINT('Ctrl Pts',(31.895291910488,16.168011819419,-31.0418477578044));
#32012=CARTESIAN_POINT('Ctrl Pts',(31.8646744620479,16.1672513233695,-31.0422439429542));
#32013=CARTESIAN_POINT('Ctrl Pts',(31.8329224323944,16.1664582369103,-31.0426570718779));
#32014=CARTESIAN_POINT('Ctrl Pts',(31.7319354368357,16.163935833788,-31.0439710240642));
#32015=CARTESIAN_POINT('Ctrl Pts',(31.6284526822058,16.1613063818565,-31.0453389332579));
#32016=CARTESIAN_POINT('Ctrl Pts',(31.523233635432,16.1587277943726,-31.0466795487252));
#32017=CARTESIAN_POINT('Ctrl Pts',(31.4188807866252,16.156170434673,-31.0480091278028));
#32018=CARTESIAN_POINT('Ctrl Pts',(31.3128198672025,16.1536645426213,-31.0493111005243));
#32019=CARTESIAN_POINT('Ctrl Pts',(31.2058402970409,16.1513736799426,-31.0505011542277));
#32020=CARTESIAN_POINT('Ctrl Pts',(31.1464339374053,16.1501015509562,-31.0511619977718));
#32021=CARTESIAN_POINT('Ctrl Pts',(31.0867451889515,16.1488957763821,-31.051788304276));
#32022=CARTESIAN_POINT('Ctrl Pts',(31.0269161235859,16.1477831210733,-31.052366291213));
#32023=CARTESIAN_POINT('Ctrl Pts',(30.9223727403119,16.1458389029967,-31.0533762469848));
#32024=CARTESIAN_POINT('Ctrl Pts',(30.8173993541569,16.1441811147896,-31.0542375463396));
#32025=CARTESIAN_POINT('Ctrl Pts',(30.7129204018003,16.1429541726495,-31.0548748925162));
#32026=CARTESIAN_POINT('Ctrl Pts',(30.6397146645873,16.1420944855847,-31.0553214647269));
#32027=CARTESIAN_POINT('Ctrl Pts',(30.5667525557982,16.1414458510594,-31.0556583368409));
#32028=CARTESIAN_POINT('Ctrl Pts',(30.4943593393942,16.1410459118957,-31.0558660149161));
#32029=CARTESIAN_POINT('',(30.5,18.7405179110272,-29.559989655385));
#32030=CARTESIAN_POINT('Origin',(30.5,0.,0.));
#32031=CARTESIAN_POINT('Ctrl Pts',(30.5049791804999,18.7395177484755,-29.5605178050969));
#32032=CARTESIAN_POINT('Ctrl Pts',(30.597367682774,18.74007970098,-29.5601622646425));
#32033=CARTESIAN_POINT('Ctrl Pts',(30.6891105694842,18.741056756011,-29.5595425101545));
#32034=CARTESIAN_POINT('Ctrl Pts',(30.7806774793076,18.7423441244045,-29.5587264396731));
#32035=CARTESIAN_POINT('Ctrl Pts',(30.8441888930625,18.7432370516295,-29.5581604077944));
#32036=CARTESIAN_POINT('Ctrl Pts',(30.9076166453413,18.7442800408073,-29.5574994222388));
#32037=CARTESIAN_POINT('Ctrl Pts',(30.9711288096736,18.7454455999908,-29.5567612578197));
#32038=CARTESIAN_POINT('Ctrl Pts',(31.0735567068107,18.7473253308645,-29.5555707987951));
#32039=CARTESIAN_POINT('Ctrl Pts',(31.176201908291,18.7495231556638,-29.5541800414695));
#32040=CARTESIAN_POINT('Ctrl Pts',(31.2798872709465,18.7519033574719,-29.5526737444511));
#32041=CARTESIAN_POINT('Ctrl Pts',(31.3828989348227,18.7542680938468,-29.5511772346432));
#32042=CARTESIAN_POINT('Ctrl Pts',(31.4869372222045,18.7568144117906,-29.5495656759356));
#32043=CARTESIAN_POINT('Ctrl Pts',(31.5928574097326,18.7594156373079,-29.5479181178242));
#32044=CARTESIAN_POINT('Ctrl Pts',(31.6516459294224,18.7608593866168,-29.5470036792764));
#32045=CARTESIAN_POINT('Ctrl Pts',(31.7110150391174,18.7623200347848,-29.5460781618904));
#32046=CARTESIAN_POINT('Ctrl Pts',(31.771117672524,18.7637740491308,-29.5451562912552));
#32047=CARTESIAN_POINT('Ctrl Pts',(31.8409082760362,18.7654624366934,-29.5440858238838));
#32048=CARTESIAN_POINT('Ctrl Pts',(31.9056373311744,18.7669933631238,-29.5431152615712));
#32049=CARTESIAN_POINT('Ctrl Pts',(31.9658882086279,18.7683675834938,-29.5422441375116));
#32050=CARTESIAN_POINT('Ctrl Pts',(32.0341093482752,18.7699235920322,-29.5412577771691));
#32051=CARTESIAN_POINT('Ctrl Pts',(32.0965888127919,18.7712796560441,-29.5403982847663));
#32052=CARTESIAN_POINT('Ctrl Pts',(32.1542362617658,18.772463407492,-29.5396480149482));
#32053=CARTESIAN_POINT('Ctrl Pts',(32.2151538519833,18.7737143090828,-29.5388551849072));
#32054=CARTESIAN_POINT('Ctrl Pts',(32.2706761902197,18.7747738843963,-29.5381836213571));
#32055=CARTESIAN_POINT('Ctrl Pts',(32.3219402247771,18.7756849339007,-29.5376060245815));
#32056=CARTESIAN_POINT('Ctrl Pts',(32.3761674213252,18.7766486438578,-29.5369950415767));
#32057=CARTESIAN_POINT('Ctrl Pts',(32.4256304058838,18.7774469218489,-29.5364887148645));
#32058=CARTESIAN_POINT('Ctrl Pts',(32.471735031406,18.7781265619111,-29.5360572749795));
#32059=CARTESIAN_POINT('Ctrl Pts',(32.5214923281247,18.7788600469324,-29.5355916539678));
#32060=CARTESIAN_POINT('Ctrl Pts',(32.5673384642519,18.7794559410664,-29.535212877449));
#32061=CARTESIAN_POINT('Ctrl Pts',(32.6111004962922,18.7799576530149,-29.5348934788925));
#32062=CARTESIAN_POINT('Ctrl Pts',(32.6551147163173,18.7804622561848,-29.5345722397342));
#32063=CARTESIAN_POINT('Ctrl Pts',(32.6970214084867,18.7808718608787,-29.5343108907555));
#32064=CARTESIAN_POINT('Ctrl Pts',(32.7387279964578,18.7812095285093,-29.5340950825229));
#32065=CARTESIAN_POINT('Ctrl Pts',(32.7800761354878,18.7815442940419,-29.5338811290628));
#32066=CARTESIAN_POINT('Ctrl Pts',(32.821227734235,18.7818087481601,-29.5337116838821));
#32067=CARTESIAN_POINT('Ctrl Pts',(32.8640829337526,18.7820000955038,-29.5335890251801));
#32068=CARTESIAN_POINT('Ctrl Pts',(32.9037320332525,18.782177127695,-29.5334755428692));
#32069=CARTESIAN_POINT('Ctrl Pts',(32.9448394203908,18.7822919200909,-29.5334018918634));
#32070=CARTESIAN_POINT('Ctrl Pts',(32.9889438598235,18.7823158450365,-29.5333868654403));
#32071=CARTESIAN_POINT('Ctrl Pts',(32.9925102269245,18.7823177796522,-29.5333856503758));
#32072=CARTESIAN_POINT('Ctrl Pts',(32.9960962106233,18.7823191027631,-29.5333848297965));
#32073=CARTESIAN_POINT('Ctrl Pts',(32.9997026353886,18.7823197895504,-29.5333844198651));
#32074=CARTESIAN_POINT('Ctrl Pts',(33.0361388185044,18.7823267282527,-29.5333802782741));
#32075=CARTESIAN_POINT('Ctrl Pts',(33.0740002606602,18.7823330770043,-29.5333765562526));
#32076=CARTESIAN_POINT('Ctrl Pts',(33.1140504028665,18.7823389179973,-29.5333733966323));
#32077=CARTESIAN_POINT('Ctrl Pts',(33.2460690464805,18.7823581718609,-29.5333629814687));
#32078=CARTESIAN_POINT('Ctrl Pts',(33.3720922029404,18.7823661897827,-29.5333587011921));
#32079=CARTESIAN_POINT('Ctrl Pts',(33.4992849360723,18.7823737360728,-29.5333546566754));
#32080=CARTESIAN_POINT('Ctrl Pts',(33.6626792864135,18.7823834301892,-29.5333494610076));
#32081=CARTESIAN_POINT('Ctrl Pts',(33.8280037294634,18.7823923459957,-29.5333446544024));
#32082=CARTESIAN_POINT('Ctrl Pts',(33.9928746198632,18.7824059536075,-29.533337331307));
#32083=CARTESIAN_POINT('Ctrl Pts',(34.3226164006628,18.7824331688311,-29.5333226851163));
#32084=CARTESIAN_POINT('Ctrl Pts',(34.6505439708619,18.7824791512757,-29.533297972965));
#32085=CARTESIAN_POINT('Ctrl Pts',(34.9791449252859,18.7825099763788,-29.5332814027047));
#32086=CARTESIAN_POINT('Ctrl Pts',(35.3077458797098,18.7825408014818,-29.5332648324443));
#32087=CARTESIAN_POINT('Ctrl Pts',(35.6370202183587,18.7825564692434,-29.533256404075));
#32088=CARTESIAN_POINT('Ctrl Pts',(35.9661418060972,18.7825697306316,-29.5332492722833));
#32089=CARTESIAN_POINT('Ctrl Pts',(36.2952633938356,18.7825829920198,-29.5332421404916));
#32090=CARTESIAN_POINT('Ctrl Pts',(36.6242322306636,18.7825938470346,-29.5332363052775));
#32091=CARTESIAN_POINT('Ctrl Pts',(36.9531363303402,18.7826154119859,-29.5332247108409));
#32092=CARTESIAN_POINT('Ctrl Pts',(38.1022190076917,18.7826907528288,-29.5331842036953));
#32093=CARTESIAN_POINT('Ctrl Pts',(39.2505115204485,18.782896816333,-29.5330734009978));
#32094=CARTESIAN_POINT('Ctrl Pts',(40.400093943525,18.7829477771169,-29.533045998731));
#32095=CARTESIAN_POINT('Ctrl Pts',(6.89999999997365,9.63452070648359,-5.36789542691341));
#32096=CARTESIAN_POINT('Ctrl Pts',(6.99168932310453,9.60499723839753,-5.42175501956001));
#32097=CARTESIAN_POINT('Ctrl Pts',(7.08383915760478,9.57508016834563,-5.47527828673705));
#32098=CARTESIAN_POINT('Ctrl Pts',(8.15762752947026,9.22342495405909,-6.09209251732963));
#32099=CARTESIAN_POINT('Ctrl Pts',(9.16608342448599,8.84591675027098,-6.61836595106259));
#32100=CARTESIAN_POINT('Ctrl Pts',(11.2535425311854,8.09542754093136,-7.53037930120419));
#32101=CARTESIAN_POINT('Ctrl Pts',(12.2577133097064,7.7072500137176,-7.91666449612082));
#32102=CARTESIAN_POINT('Ctrl Pts',(14.356433377742,6.97440810645326,-8.58141250110814));
#32103=CARTESIAN_POINT('Ctrl Pts',(15.3659105035251,6.61345583116596,-8.85322312286061));
#32104=CARTESIAN_POINT('Ctrl Pts',(17.4728641219044,5.96623757129007,-9.31281879192962));
#32105=CARTESIAN_POINT('Ctrl Pts',(18.4890996814195,5.66020885204394,-9.49384943617778));
#32106=CARTESIAN_POINT('Ctrl Pts',(19.8476172011441,5.32865724601648,-9.68599953593308));
#32107=CARTESIAN_POINT('Ctrl Pts',(20.3454889307686,5.20930542916259,-9.75195458239819));
#32108=CARTESIAN_POINT('Ctrl Pts',(21.3782040612024,4.97678151322346,-9.87366876552719));
#32109=CARTESIAN_POINT('Ctrl Pts',(22.1792648896895,4.81935607344486,-9.95072592994715));
#32110=CARTESIAN_POINT('Ctrl Pts',(22.8542621828909,4.70591921690554,-10.0067883222624));
#32111=CARTESIAN_POINT('Ctrl Pts',(23.1054579010967,4.66456206383028,-10.0267605301623));
#32112=CARTESIAN_POINT('Ctrl Pts',(23.6171513959785,4.58448144656259,-10.0644076466806));
#32113=CARTESIAN_POINT('Ctrl Pts',(24.1360713221937,4.51012725444834,-10.0979855598765));
#32114=CARTESIAN_POINT('Ctrl Pts',(24.6624927871864,4.44285620865165,-10.1277002159266));
#32115=CARTESIAN_POINT('Ctrl Pts',(25.1928168818088,4.3809527171812,-10.154786256444));
#32116=CARTESIAN_POINT('Ctrl Pts',(25.5948982287615,4.34117176259643,-10.1721457030179));
#32117=CARTESIAN_POINT('Ctrl Pts',(26.1232031889651,4.29604941535506,-10.1922876384417));
#32118=CARTESIAN_POINT('Ctrl Pts',(27.1768897027567,4.2232612911204,-10.2241871753182));
#32119=CARTESIAN_POINT('Ctrl Pts',(28.2111297865347,4.19969555688313,-10.2325109692973));
#32120=CARTESIAN_POINT('Ctrl Pts',(29.1277555719713,4.17661492679514,-10.2421056253618));
#32121=CARTESIAN_POINT('Ctrl Pts',(29.4767605677587,4.1700561490002,-10.2448788784735));
#32122=CARTESIAN_POINT('Ctrl Pts',(30.1601418995912,4.16421367130871,-10.2473221772452));
#32123=CARTESIAN_POINT('Ctrl Pts',(31.3500242312262,4.16794387579264,-10.2457563290907));
#32124=CARTESIAN_POINT('Ctrl Pts',(32.3461596131128,4.18040640609126,-10.2405791191157));
#32125=CARTESIAN_POINT('Ctrl Pts',(33.1614718826738,4.18039330945984,-10.2405840900447));
#32126=CARTESIAN_POINT('Ctrl Pts',(33.4925794155279,4.18039253080268,-10.2405841444578));
#32127=CARTESIAN_POINT('Ctrl Pts',(34.1499904318886,4.18039030822714,-10.2405848392549));
#32128=CARTESIAN_POINT('Ctrl Pts',(34.9738731541179,4.18038393925505,-10.2405865289644));
#32129=CARTESIAN_POINT('Ctrl Pts',(35.9612754428242,4.18038119412748,-10.2405873001735));
#32130=CARTESIAN_POINT('Ctrl Pts',(37.936646788162,4.18037753677864,-10.2405882857915));
#32131=CARTESIAN_POINT('Ctrl Pts',(39.5833333333333,4.18035859466987,-10.2405934798255));
#32132=CARTESIAN_POINT('Ctrl Pts',(40.9,4.18035859466987,-10.2405934798255));
#32133=CARTESIAN_POINT('Ctrl Pts',(6.71972576838711,12.8464244365415,-6.57643817146341));
#32134=CARTESIAN_POINT('Ctrl Pts',(6.81144220747046,12.8102053989753,-6.64828376862611));
#32135=CARTESIAN_POINT('Ctrl Pts',(6.90362823998598,12.7734498343709,-6.7197152492286));
#32136=CARTESIAN_POINT('Ctrl Pts',(7.9778781148633,12.3410744046091,-7.54294881554196));
#32137=CARTESIAN_POINT('Ctrl Pts',(8.98681832185142,11.871220138602,-8.24809748747638));
#32138=CARTESIAN_POINT('Ctrl Pts',(11.0806583453373,10.9274240314556,-9.47774891389535));
#32139=CARTESIAN_POINT('Ctrl Pts',(12.0862475175457,10.4368998098017,-10.0005505115845));
#32140=CARTESIAN_POINT('Ctrl Pts',(14.197639322261,9.50280276487817,-10.906656993414));
#32141=CARTESIAN_POINT('Ctrl Pts',(15.2100862637122,9.04203633254719,-11.2785931828498));
#32142=CARTESIAN_POINT('Ctrl Pts',(17.3364698493954,8.20932952666152,-11.9121957711898));
#32143=CARTESIAN_POINT('Ctrl Pts',(18.357279581038,7.81594677169138,-12.1627870018009));
#32144=CARTESIAN_POINT('Ctrl Pts',(19.7331217809845,7.38628119283515,-12.4307568384137));
#32145=CARTESIAN_POINT('Ctrl Pts',(20.2341927100358,7.23233618870704,-12.5225360922774));
#32146=CARTESIAN_POINT('Ctrl Pts',(21.2777139275316,6.93114017240204,-12.6928916013278));
#32147=CARTESIAN_POINT('Ctrl Pts',(22.0885637816418,6.72673758680646,-12.8012350092453));
#32148=CARTESIAN_POINT('Ctrl Pts',(22.7734874647764,6.57909772915771,-12.8801738355232));
#32149=CARTESIAN_POINT('Ctrl Pts',(23.0269571312139,6.52549682636868,-12.9082278965574));
#32150=CARTESIAN_POINT('Ctrl Pts',(23.5444618566097,6.42148511325402,-12.9612738268023));
#32151=CARTESIAN_POINT('Ctrl Pts',(24.0694383156461,6.32485290039693,-13.0087020921734));
#32152=CARTESIAN_POINT('Ctrl Pts',(24.6027295908464,6.2373000813771,-13.0507741241225));
#32153=CARTESIAN_POINT('Ctrl Pts',(25.1403192523141,6.15667530541498,-13.0891677302172));
#32154=CARTESIAN_POINT('Ctrl Pts',(25.5484689870706,6.10479659087691,-13.1137995888261));
#32155=CARTESIAN_POINT('Ctrl Pts',(26.0852808149067,6.04589855121054,-13.1423647911197));
#32156=CARTESIAN_POINT('Ctrl Pts',(27.1586857291269,5.95074158602807,-13.1877077660314));
#32157=CARTESIAN_POINT('Ctrl Pts',(28.1995312980844,5.92039197700573,-13.1995114624862));
#32158=CARTESIAN_POINT('Ctrl Pts',(29.1157533315888,5.89061060808305,-13.2130297822556));
#32159=CARTESIAN_POINT('Ctrl Pts',(29.4698938670486,5.88204921070822,-13.2169740538762));
#32160=CARTESIAN_POINT('Ctrl Pts',(30.1587234046998,5.87447683559579,-13.220429005539));
#32161=CARTESIAN_POINT('Ctrl Pts',(31.355731195606,5.87931523414859,-13.2182120926509));
#32162=CARTESIAN_POINT('Ctrl Pts',(32.350180243561,5.89537176970751,-13.2109234983782));
#32163=CARTESIAN_POINT('Ctrl Pts',(33.1605031382466,5.89535013085608,-13.2109314016452));
#32164=CARTESIAN_POINT('Ctrl Pts',(33.4922179295252,5.89534881762644,-13.2109314596682));
#32165=CARTESIAN_POINT('Ctrl Pts',(34.1493400019899,5.89534512891167,-13.2109325467447));
#32166=CARTESIAN_POINT('Ctrl Pts',(34.9735241318652,5.89533452524069,-13.2109351472382));
#32167=CARTESIAN_POINT('Ctrl Pts',(35.9608954520827,5.89532995964261,-13.2109363413972));
#32168=CARTESIAN_POINT('Ctrl Pts',(37.9363824842976,5.89532387223529,-13.2109378608691));
#32169=CARTESIAN_POINT('Ctrl Pts',(39.5833333333333,5.89529235427928,-13.2109458830841));
#32170=CARTESIAN_POINT('Ctrl Pts',(40.9,5.89529235427928,-13.2109458830841));
#32171=CARTESIAN_POINT('Ctrl Pts',(6.48177011792014,20.336764848396,-9.40621265917916));
#32172=CARTESIAN_POINT('Ctrl Pts',(6.57271435585528,20.2851799357091,-9.51911083717173));
#32173=CARTESIAN_POINT('Ctrl Pts',(6.66411141569866,20.2327517601296,-9.63139437446866));
#32174=CARTESIAN_POINT('Ctrl Pts',(7.73048017258431,19.614616528956,-10.9276768808967));
#32175=CARTESIAN_POINT('Ctrl Pts',(8.73292722985418,18.9319609573801,-12.0456324995184));
#32176=CARTESIAN_POINT('Ctrl Pts',(10.8102906905198,17.5485371602851,-14.0013807284478));
#32177=CARTESIAN_POINT('Ctrl Pts',(11.8125687231201,16.8218444562665,-14.8418955382559));
#32178=CARTESIAN_POINT('Ctrl Pts',(13.9177445864075,15.4271303717406,-16.3050153868123));
#32179=CARTESIAN_POINT('Ctrl Pts',(14.9296562678442,14.7350649820735,-16.9116612373854));
#32180=CARTESIAN_POINT('Ctrl Pts',(17.0680844879216,13.4708635112562,-17.9535844659564));
#32181=CARTESIAN_POINT('Ctrl Pts',(18.0932339179161,12.8729609429,-18.3688941094638));
#32182=CARTESIAN_POINT('Ctrl Pts',(19.4933464326809,12.2099892645604,-18.8183285494774));
#32183=CARTESIAN_POINT('Ctrl Pts',(19.9993272808496,11.9744841299437,-18.971430097181));
#32184=CARTESIAN_POINT('Ctrl Pts',(21.0600020168761,11.5100300116438,-19.2581324129064));
#32185=CARTESIAN_POINT('Ctrl Pts',(21.8888875769482,11.1928649299996,-19.4420158954033));
#32186=CARTESIAN_POINT('Ctrl Pts',(22.5933490549503,10.962505511385,-19.5764520117208));
#32187=CARTESIAN_POINT('Ctrl Pts',(22.8513437851799,10.8796937171906,-19.6238525927722));
#32188=CARTESIAN_POINT('Ctrl Pts',(23.3805933886566,10.7182299385361,-19.7139851739534));
#32189=CARTESIAN_POINT('Ctrl Pts',(23.9182257576785,10.5680285062335,-19.7948254980796));
#32190=CARTESIAN_POINT('Ctrl Pts',(24.4662138806868,10.4315004891655,-19.8668205194741));
#32191=CARTESIAN_POINT('Ctrl Pts',(25.0195744741822,10.3055778221167,-19.9326328666884));
#32192=CARTESIAN_POINT('Ctrl Pts',(25.4412458088222,10.2242864909386,-19.9749776253082));
#32193=CARTESIAN_POINT('Ctrl Pts',(25.9971983460992,10.131797107587,-20.0240850656221));
#32194=CARTESIAN_POINT('Ctrl Pts',(27.1157050405652,9.9818233225046,-20.102368552767));
#32195=CARTESIAN_POINT('Ctrl Pts',(28.1723100127449,9.93573708068023,-20.1222437541335));
#32196=CARTESIAN_POINT('Ctrl Pts',(29.0876106506766,9.89029022572783,-20.1449463132817));
#32197=CARTESIAN_POINT('Ctrl Pts',(29.4537207931442,9.87684873205162,-20.1517438988729));
#32198=CARTESIAN_POINT('Ctrl Pts',(30.1552759232946,9.86516345924736,-20.1576060163182));
#32199=CARTESIAN_POINT('Ctrl Pts',(31.368924127636,9.87263514017792,-20.1538463873917));
#32200=CARTESIAN_POINT('Ctrl Pts',(32.3594787154311,9.89702302165623,-20.1416711708076));
#32201=CARTESIAN_POINT('Ctrl Pts',(33.1581760188914,9.89696607979066,-20.1416983285705));
#32202=CARTESIAN_POINT('Ctrl Pts',(33.4913102145729,9.89696201382194,-20.1416998058431));
#32203=CARTESIAN_POINT('Ctrl Pts',(34.1477617736107,9.89695193052412,-20.1417043298969));
#32204=CARTESIAN_POINT('Ctrl Pts',(34.9726616332633,9.89692218573782,-20.1417171222835));
#32205=CARTESIAN_POINT('Ctrl Pts',(35.9599657908142,9.89690948638391,-20.1417226604566));
#32206=CARTESIAN_POINT('Ctrl Pts',(37.9357298104643,9.89689244880615,-20.1417300151411));
#32207=CARTESIAN_POINT('Ctrl Pts',(39.5833333333333,9.89680446003459,-20.1417681573542));
#32208=CARTESIAN_POINT('Ctrl Pts',(40.9,9.89680446003459,-20.1417681573542));
#32209=CARTESIAN_POINT('Ctrl Pts',(6.40644620858992,27.7818319413302,-12.3446157076951));
#32210=CARTESIAN_POINT('Ctrl Pts',(6.49686818484384,27.7146057723314,-12.4976194141968));
#32211=CARTESIAN_POINT('Ctrl Pts',(6.58771883172007,27.6462615383487,-12.6497754970258));
#32212=CARTESIAN_POINT('Ctrl Pts',(7.64885870107048,26.838967465877,-14.4089312086777));
#32213=CARTESIAN_POINT('Ctrl Pts',(8.64786699401838,25.9406999974137,-15.9309901815184));
#32214=CARTESIAN_POINT('Ctrl Pts',(10.7071344443812,24.1258468463739,-18.5841088194585));
#32215=CARTESIAN_POINT('Ctrl Pts',(11.7059636153277,23.1640388241121,-19.7351568023896));
#32216=CARTESIAN_POINT('Ctrl Pts',(13.7894167134297,21.32755345859,-21.7274097031724));
#32217=CARTESIAN_POINT('Ctrl Pts',(14.7964804448639,20.4089660621499,-22.5625068415354));
#32218=CARTESIAN_POINT('Ctrl Pts',(16.9150096963282,18.7347867871849,-23.9923642448819));
#32219=CARTESIAN_POINT('Ctrl Pts',(17.9356563974909,17.9376031564435,-24.568778311437));
#32220=CARTESIAN_POINT('Ctrl Pts',(19.3316378726114,17.0495061236355,-25.1942531765859));
#32221=CARTESIAN_POINT('Ctrl Pts',(19.8373783148988,16.733671277521,-25.4080883980549));
#32222=CARTESIAN_POINT('Ctrl Pts',(20.8986146451321,16.1088561234904,-25.8097110946141));
#32223=CARTESIAN_POINT('Ctrl Pts',(21.7322089233615,15.6790344990822,-26.0695581056351));
#32224=CARTESIAN_POINT('Ctrl Pts',(22.4452152218927,15.3644450466694,-26.2607608176433));
#32225=CARTESIAN_POINT('Ctrl Pts',(22.7053175952387,15.2520352575854,-26.3278633535721));
#32226=CARTESIAN_POINT('Ctrl Pts',(23.2405350109148,15.0319031635371,-26.456049557717));
#32227=CARTESIAN_POINT('Ctrl Pts',(23.7856351879594,14.8265027181049,-26.5714803865859));
#32228=CARTESIAN_POINT('Ctrl Pts',(24.3434088150882,14.6389049166987,-26.6748081507042));
#32229=CARTESIAN_POINT('Ctrl Pts',(24.9080926446007,14.4653482504621,-26.7695587595053));
#32230=CARTESIAN_POINT('Ctrl Pts',(25.3404979553364,14.3526452692475,-26.8308622015488));
#32231=CARTESIAN_POINT('Ctrl Pts',(25.9125607075504,14.2239063651395,-26.9021372597287));
#32232=CARTESIAN_POINT('Ctrl Pts',(27.0720378258712,14.0136986134135,-27.0165941086124));
#32233=CARTESIAN_POINT('Ctrl Pts',(28.1454151442859,13.9518646781024,-27.0445191043407));
#32234=CARTESIAN_POINT('Ctrl Pts',(29.0596751952944,13.890725520751,-27.0764264216485));
#32235=CARTESIAN_POINT('Ctrl Pts',(29.4376599373188,13.8719255145712,-27.0863532011149));
#32236=CARTESIAN_POINT('Ctrl Pts',(30.1519376760718,13.855954576287,-27.0947220176404));
#32237=CARTESIAN_POINT('Ctrl Pts',(31.3821999577689,13.8661782937677,-27.0893514143297));
#32238=CARTESIAN_POINT('Ctrl Pts',(32.3688386893657,13.8987881217581,-27.0723527225427));
#32239=CARTESIAN_POINT('Ctrl Pts',(33.1558986739574,13.8986675947835,-27.0724155351932));
#32240=CARTESIAN_POINT('Ctrl Pts',(33.49045038666,13.8986584195583,-27.072419804706));
#32241=CARTESIAN_POINT('Ctrl Pts',(34.1462287076184,13.8986367255002,-27.0724307945236));
#32242=CARTESIAN_POINT('Ctrl Pts',(34.9718350023128,13.8985720488061,-27.0724629552156));
#32243=CARTESIAN_POINT('Ctrl Pts',(35.9590682028415,13.8985445297567,-27.0724767217601));
#32244=CARTESIAN_POINT('Ctrl Pts',(37.9351039480424,13.8985075170899,-27.072495155898));
#32245=CARTESIAN_POINT('Ctrl Pts',(39.5833333333333,13.8983165657899,-27.0725904316243));
#32246=CARTESIAN_POINT('Ctrl Pts',(40.9,13.8983165657899,-27.0725904316243));
#32247=CARTESIAN_POINT('Ctrl Pts',(6.37427268165564,32.0290848932163,-14.0406695266741));
#32248=CARTESIAN_POINT('Ctrl Pts',(6.46448755772838,31.9528098065586,-14.2166050753401));
#32249=CARTESIAN_POINT('Ctrl Pts',(6.55512327887565,31.8752581000468,-14.3915605358513));
#32250=CARTESIAN_POINT('Ctrl Pts',(7.61410360785656,30.958672886913,-16.4151695040826));
#32251=CARTESIAN_POINT('Ctrl Pts',(8.61142775869687,29.9361952854453,-18.1677152487792));
#32252=CARTESIAN_POINT('Ctrl Pts',(10.6634825022472,27.8730682250752,-21.2183968262284));
#32253=CARTESIAN_POINT('Ctrl Pts',(11.6607542873627,26.7761583709751,-22.5462154536683));
#32254=CARTESIAN_POINT('Ctrl Pts',(13.7353039743977,24.6873364683673,-24.8383185913233));
#32255=CARTESIAN_POINT('Ctrl Pts',(14.7402095633116,23.6392130729629,-25.802985911944));
#32256=CARTESIAN_POINT('Ctrl Pts',(16.8490881066137,21.733995182915,-27.450307490631));
#32257=CARTESIAN_POINT('Ctrl Pts',(17.8672038783315,20.8239061433235,-28.1175362426871));
#32258=CARTESIAN_POINT('Ctrl Pts',(19.2585933984997,19.811022849419,-28.8404836901117));
#32259=CARTESIAN_POINT('Ctrl Pts',(19.7636418533908,19.4499572035579,-29.0884650342026));
#32260=CARTESIAN_POINT('Ctrl Pts',(20.8231816497994,18.7357747989967,-29.5540603372584));
#32261=CARTESIAN_POINT('Ctrl Pts',(21.6568670511735,18.2431916560479,-29.8562628482713));
#32262=CARTESIAN_POINT('Ctrl Pts',(22.3720072062877,17.8815051531587,-30.0792593376712));
#32263=CARTESIAN_POINT('Ctrl Pts',(22.6326824787813,17.7523977438431,-30.1574913312728));
#32264=CARTESIAN_POINT('Ctrl Pts',(23.1697036949937,17.4991937768336,-30.3071564102286));
#32265=CARTESIAN_POINT('Ctrl Pts',(23.7174377716562,17.2625030946595,-30.4422233412819));
#32266=CARTESIAN_POINT('Ctrl Pts',(24.2790946262572,17.0457855087881,-30.5634410393029));
#32267=CARTESIAN_POINT('Ctrl Pts',(24.8485847331463,16.8449230908939,-30.6748008187179));
#32268=CARTESIAN_POINT('Ctrl Pts',(25.2859632686137,16.714000734413,-30.7471152582869));
#32269=CARTESIAN_POINT('Ctrl Pts',(25.8659001690755,16.5640760155963,-30.8313513860032));
#32270=CARTESIAN_POINT('Ctrl Pts',(27.0467877055032,16.3181083484214,-30.9672841404844));
#32271=CARTESIAN_POINT('Ctrl Pts',(28.1301993946288,16.2470842981322,-30.9999203594232));
#32272=CARTESIAN_POINT('Ctrl Pts',(29.0438132065911,16.1769735529556,-31.0370949113971));
#32273=CARTESIAN_POINT('Ctrl Pts',(29.4285323170642,16.1549555741443,-31.0489002942269));
#32274=CARTESIAN_POINT('Ctrl Pts',(30.1500796604944,16.1364761766636,-31.0587367393328));
#32275=CARTESIAN_POINT('Ctrl Pts',(31.3898224001987,16.1483068856791,-31.0524272220083));
#32276=CARTESIAN_POINT('Ctrl Pts',(32.3742147772173,16.1855693458549,-31.0327017051641));
#32277=CARTESIAN_POINT('Ctrl Pts',(33.1546196294426,16.1853991323255,-31.0327939306214));
#32278=CARTESIAN_POINT('Ctrl Pts',(33.4899805045662,16.1853856345319,-31.0328008093452));
#32279=CARTESIAN_POINT('Ctrl Pts',(34.1453728987309,16.1853546639145,-31.0328173216774));
#32280=CARTESIAN_POINT('Ctrl Pts',(34.9713787068036,16.1852616946182,-31.0328663827335));
#32281=CARTESIAN_POINT('Ctrl Pts',(35.9585696612047,16.1852222245757,-31.0328872804502));
#32282=CARTESIAN_POINT('Ctrl Pts',(37.9347583211501,16.1851690519236,-31.0329153648958));
#32283=CARTESIAN_POINT('Ctrl Pts',(39.5833333333333,16.1848949119358,-31.0330603026358));
#32284=CARTESIAN_POINT('Ctrl Pts',(40.9,16.1848949119358,-31.0330603026358));
#32285=CARTESIAN_POINT('',(40.9,15.1839076262002,-29.2992994660114));
#32286=CARTESIAN_POINT('Ctrl Pts',(40.9,15.1839076262002,-29.2992994660114));
#32287=CARTESIAN_POINT('Ctrl Pts',(40.9,15.4341550287793,-29.7327406817405));
#32288=CARTESIAN_POINT('Ctrl Pts',(40.9,15.6844024313583,-30.1661818974696));
#32289=CARTESIAN_POINT('Ctrl Pts',(40.9,15.9346498339374,-30.5996231131986));
#32290=CARTESIAN_POINT('',(38.,15.1839076262003,-29.2992994660114));
#32291=CARTESIAN_POINT('Ctrl Pts',(38.,15.1839076262003,-29.2992994660114));
#32292=CARTESIAN_POINT('Ctrl Pts',(38.9666666666667,15.1839076262003,-29.2992994660114));
#32293=CARTESIAN_POINT('Ctrl Pts',(39.9333333333333,15.1839076262003,-29.2992994660114));
#32294=CARTESIAN_POINT('Ctrl Pts',(40.9,15.1839076262003,-29.2992994660114));
#32295=CARTESIAN_POINT('Ctrl Pts',(37.4974382384971,14.8838038109906,-28.7790269720419));
#32296=CARTESIAN_POINT('Ctrl Pts',(37.6645213547145,14.9840691120819,-28.9527098777878));
#32297=CARTESIAN_POINT('Ctrl Pts',(37.8313739960415,15.0841847150559,-29.1261374112003));
#32298=CARTESIAN_POINT('Ctrl Pts',(37.9978889629903,15.1840905833949,-29.2992044501375));
#32299=CARTESIAN_POINT('',(6.9,27.0393531365015,-12.9951291628659));
#32300=CARTESIAN_POINT('Ctrl Pts',(6.9,27.0393531365015,-12.9951291628659));
#32301=CARTESIAN_POINT('Ctrl Pts',(6.9,24.649274247254,-11.9174419758914));
#32302=CARTESIAN_POINT('Ctrl Pts',(6.90000000000115,22.230729924082,-10.8339866674746));
#32303=CARTESIAN_POINT('Ctrl Pts',(6.90000000000115,16.7584145047598,-8.41000082059025));
#32304=CARTESIAN_POINT('Ctrl Pts',(6.9,13.1312177506378,-6.82522008706164));
#32305=CARTESIAN_POINT('Ctrl Pts',(6.9,9.63452070648529,-5.36789542693313));
#32306=CARTESIAN_POINT('',(22.9245129145126,15.8853026165582,-27.5141512254857));
#32307=CARTESIAN_POINT('Ctrl Pts',(22.9245129145126,15.8853026165582,-27.5141512254857));
#32308=CARTESIAN_POINT('Ctrl Pts',(22.7202811020963,15.9355315703924,-27.405303612937));
#32309=CARTESIAN_POINT('Ctrl Pts',(22.5089075447093,15.9922246435191,-27.2924652433825));
#32310=CARTESIAN_POINT('Ctrl Pts',(22.2913349439917,16.0558281873747,-27.1762359097413));
#32311=CARTESIAN_POINT('Ctrl Pts',(21.4451770585294,16.3031876434794,-26.7242103933933));
#32312=CARTESIAN_POINT('Ctrl Pts',(20.5220951556672,16.6965145338604,-26.2108400614944));
#32313=CARTESIAN_POINT('Ctrl Pts',(19.7671428819544,17.0753616782141,-25.7770859372682));
#32314=CARTESIAN_POINT('Ctrl Pts',(19.5194773058395,17.1996442316058,-25.6347908958341));
#32315=CARTESIAN_POINT('Ctrl Pts',(19.2865716386092,17.3225345039426,-25.4994131575073));
#32316=CARTESIAN_POINT('Ctrl Pts',(19.0728538401323,17.4387046858284,-25.3740784559106));
#32317=CARTESIAN_POINT('Ctrl Pts',(18.7028555998036,17.6398239336528,-25.1570931632801));
#32318=CARTESIAN_POINT('Ctrl Pts',(18.4144703596236,17.8106758656204,-24.9815167506412));
#32319=CARTESIAN_POINT('Ctrl Pts',(18.0642874871539,18.0298340093773,-24.7606238748753));
#32320=CARTESIAN_POINT('Ctrl Pts',(17.4420927116722,18.419227845484,-24.3681478172275));
#32321=CARTESIAN_POINT('Ctrl Pts',(16.7224564418219,18.9163953124274,-23.8866996305776));
#32322=CARTESIAN_POINT('Ctrl Pts',(15.9202806616111,19.5075155171573,-23.2999769887242));
#32323=CARTESIAN_POINT('Ctrl Pts',(15.409052983452,19.8842371999007,-22.926057878577));
#32324=CARTESIAN_POINT('Ctrl Pts',(14.8739602945718,20.3065653819879,-22.5035099772299));
#32325=CARTESIAN_POINT('Ctrl Pts',(14.316979433116,20.764045054618,-22.0244589523046));
#32326=CARTESIAN_POINT('Ctrl Pts',(13.886420676284,21.1176871503423,-21.6541417151704));
#32327=CARTESIAN_POINT('Ctrl Pts',(13.3867890027807,21.5394320189423,-21.2019814327446));
#32328=CARTESIAN_POINT('Ctrl Pts',(12.8146824059514,22.0238946695559,-20.6456427149589));
#32329=CARTESIAN_POINT('Ctrl Pts',(12.2526665517594,22.499812430193,-20.0991166279862));
#32330=CARTESIAN_POINT('Ctrl Pts',(11.6379478462803,23.0419154065947,-19.4470356343899));
#32331=CARTESIAN_POINT('Ctrl Pts',(10.9739250490307,23.6265354530561,-18.668913747699));
#32332=CARTESIAN_POINT('Ctrl Pts',(10.5683455447962,23.9836164291783,-18.1936434853747));
#32333=CARTESIAN_POINT('Ctrl Pts',(10.1437415406955,24.3558958755273,-17.6694303965612));
#32334=CARTESIAN_POINT('Ctrl Pts',(9.74137929176525,24.6998029803349,-17.1528053766524));
#32335=CARTESIAN_POINT('Ctrl Pts',(8.72285779294233,25.5703537856744,-15.8450442956717));
#32336=CARTESIAN_POINT('Ctrl Pts',(7.81323138778195,26.3485431508901,-14.4751178145147));
#32337=CARTESIAN_POINT('Ctrl Pts',(6.9,27.0393531365015,-12.9951291628659));
#32338=CARTESIAN_POINT('Ctrl Pts',(30.5,16.1402285275843,-31.0562879796886));
#32339=CARTESIAN_POINT('Ctrl Pts',(29.9560179420817,16.0158030554221,-30.8470467059701));
#32340=CARTESIAN_POINT('Ctrl Pts',(29.4152668325132,15.9055856438303,-30.6299015220344));
#32341=CARTESIAN_POINT('Ctrl Pts',(28.8740459957565,15.8236145009995,-30.3967092920472));
#32342=CARTESIAN_POINT('Ctrl Pts',(28.353527792344,15.7447788961961,-30.1724370682909));
#32343=CARTESIAN_POINT('Ctrl Pts',(27.8179515912467,15.65999396651,-29.9423746730404));
#32344=CARTESIAN_POINT('Ctrl Pts',(27.2695051149491,15.5981844167478,-29.6962958928787));
#32345=CARTESIAN_POINT('Ctrl Pts',(26.9554553615883,15.5627912203338,-29.5553870101399));
#32346=CARTESIAN_POINT('Ctrl Pts',(26.6378099296971,15.535020897066,-29.4095747645068));
#32347=CARTESIAN_POINT('Ctrl Pts',(26.3179304017917,15.520523503095,-29.2578762499931));
#32348=CARTESIAN_POINT('Ctrl Pts',(26.1078196745982,15.5110009868852,-29.1582340959378));
#32349=CARTESIAN_POINT('Ctrl Pts',(25.8967402232745,15.507207179043,-29.0560612282453));
#32350=CARTESIAN_POINT('Ctrl Pts',(25.6850706236774,15.5107635234098,-28.9510881944939));
#32351=CARTESIAN_POINT('Ctrl Pts',(25.6562210027417,15.5112482372614,-28.9367808388889));
#32352=CARTESIAN_POINT('Ctrl Pts',(25.6277737638215,15.5118582602787,-28.9226278510966));
#32353=CARTESIAN_POINT('Ctrl Pts',(25.5983858063598,15.5126342200129,-28.9079571471847));
#32354=CARTESIAN_POINT('Ctrl Pts',(25.1249357452756,15.5251351971226,-28.6716070819486));
#32355=CARTESIAN_POINT('Ctrl Pts',(24.1510084067019,15.583657222894,-28.1678256190434));
#32356=CARTESIAN_POINT('Ctrl Pts',(22.9245129145126,15.8853026165582,-27.5141512254857));
#32357=CARTESIAN_POINT('Origin',(40.65,0.,0.));
#32358=CARTESIAN_POINT('',(40.4,31.0330398077868,-16.1848830792292));
#32359=CARTESIAN_POINT('',(40.9,30.5996231131986,-15.9346498339374));
#32360=CARTESIAN_POINT('Ctrl Pts',(40.4,31.0330398077868,-16.1848830792292));
#32361=CARTESIAN_POINT('Ctrl Pts',(40.5666590138513,30.888576136327,-16.1014769396238));
#32362=CARTESIAN_POINT('Ctrl Pts',(40.7333430451333,30.7440888805157,-16.0180571835867));
#32363=CARTESIAN_POINT('Ctrl Pts',(40.9,30.5996231131986,-15.9346498339374));
#32364=CARTESIAN_POINT('',(40.9,29.0996231131986,-18.5327260452908));
#32365=CARTESIAN_POINT('Origin',(40.9,0.,0.));
#32366=CARTESIAN_POINT('',(40.4,29.5330398077868,-18.7829592905825));
#32367=CARTESIAN_POINT('Ctrl Pts',(40.9,29.0996231131986,-18.5327260452908));
#32368=CARTESIAN_POINT('Ctrl Pts',(40.7333430447098,29.2440888808829,-18.616133395152));
#32369=CARTESIAN_POINT('Ctrl Pts',(40.566659013253,29.3885761368456,-18.6995531512765));
#32370=CARTESIAN_POINT('Ctrl Pts',(40.4,29.5330398077868,-18.7829592905825));
#32371=CARTESIAN_POINT('Origin',(40.4,0.,0.));
#32372=CARTESIAN_POINT('Origin',(35.7,0.,0.));
#32373=CARTESIAN_POINT('',(30.5,29.5059919176187,-18.8254200738635));
#32374=CARTESIAN_POINT('Ctrl Pts',(40.3998805977094,29.5330468723882,-18.7829479019245));
#32375=CARTESIAN_POINT('Ctrl Pts',(39.2493532038211,29.5330781202017,-18.7828975281219));
#32376=CARTESIAN_POINT('Ctrl Pts',(38.0972325173324,29.5332042421652,-18.7826942098493));
#32377=CARTESIAN_POINT('Ctrl Pts',(36.9466403233752,29.5332467931519,-18.7826256101695));
#32378=CARTESIAN_POINT('Ctrl Pts',(36.7453942973752,29.533254235595,-18.7826136116412));
#32379=CARTESIAN_POINT('Ctrl Pts',(36.5441950314395,29.5332591214118,-18.7826057344612));
#32380=CARTESIAN_POINT('Ctrl Pts',(36.3429831482115,29.5332638326534,-18.7825981392431));
#32381=CARTESIAN_POINT('Ctrl Pts',(36.2103627229287,29.533266937872,-18.7825931331717));
#32382=CARTESIAN_POINT('Ctrl Pts',(36.0823539050873,29.5332699079824,-18.7825884046388));
#32383=CARTESIAN_POINT('Ctrl Pts',(35.9587472612551,29.533273304022,-18.7825830315924));
#32384=CARTESIAN_POINT('Ctrl Pts',(35.7554552092513,29.5332788893841,-18.7825741947079));
#32385=CARTESIAN_POINT('Ctrl Pts',(35.5640774641711,29.5332855100166,-18.78256380265));
#32386=CARTESIAN_POINT('Ctrl Pts',(35.3838244599967,29.5332919882698,-18.7825536727525));
#32387=CARTESIAN_POINT('Ctrl Pts',(35.2391029659044,29.5332971895284,-18.7825455396624));
#32388=CARTESIAN_POINT('Ctrl Pts',(35.1015509582766,29.5333023181163,-18.7825375448068));
#32389=CARTESIAN_POINT('Ctrl Pts',(34.9707359993239,29.5333070397951,-18.7825301856736));
#32390=CARTESIAN_POINT('Ctrl Pts',(34.857898178191,29.533311112601,-18.7825238378632));
#32391=CARTESIAN_POINT('Ctrl Pts',(34.7500670454289,29.5333148977242,-18.7825179389498));
#32392=CARTESIAN_POINT('Ctrl Pts',(34.6468496335934,29.5333184739771,-18.7825123391461));
#32393=CARTESIAN_POINT('Ctrl Pts',(34.5887227637577,29.5333204879433,-18.7825091856174));
#32394=CARTESIAN_POINT('Ctrl Pts',(34.5320601650214,29.5333224349754,-18.7825061280289));
#32395=CARTESIAN_POINT('Ctrl Pts',(34.4767987085013,29.5333243245899,-18.7825031467392));
#32396=CARTESIAN_POINT('Ctrl Pts',(34.3959515550964,29.5333270890838,-18.7824987851317));
#32397=CARTESIAN_POINT('Ctrl Pts',(34.3181086378962,29.533329735084,-18.7824945795527));
#32398=CARTESIAN_POINT('Ctrl Pts',(34.2432236356273,29.5333323757695,-18.7824903288468));
#32399=CARTESIAN_POINT('Ctrl Pts',(34.162267530415,29.5333352305416,-18.7824857335262));
#32400=CARTESIAN_POINT('Ctrl Pts',(34.0847679659788,29.5333380786013,-18.7824810862876));
#32401=CARTESIAN_POINT('Ctrl Pts',(34.0106064145146,29.5333409984257,-18.7824762390846));
#32402=CARTESIAN_POINT('Ctrl Pts',(34.0011740963656,29.5333413697867,-18.7824756225878));
#32403=CARTESIAN_POINT('Ctrl Pts',(33.9917957065319,29.5333417422356,-18.7824750029764));
#32404=CARTESIAN_POINT('Ctrl Pts',(33.982470944213,29.5333421158732,-18.7824743800456));
#32405=CARTESIAN_POINT('Ctrl Pts',(33.9223617768104,29.533344524411,-18.7824703645173));
#32406=CARTESIAN_POINT('Ctrl Pts',(33.8644761963965,29.5333469783619,-18.7824662176402));
#32407=CARTESIAN_POINT('Ctrl Pts',(33.8085662291515,29.5333493560495,-18.7824621300573));
#32408=CARTESIAN_POINT('Ctrl Pts',(33.7474237015737,29.5333519562626,-18.7824576599214));
#32409=CARTESIAN_POINT('Ctrl Pts',(33.6886441629424,29.5333544654644,-18.7824532603738));
#32410=CARTESIAN_POINT('Ctrl Pts',(33.6319696815246,29.5333567795573,-18.7824490897141));
#32411=CARTESIAN_POINT('Ctrl Pts',(33.5826925637263,29.5333587916063,-18.7824454634244));
#32412=CARTESIAN_POINT('Ctrl Pts',(33.5350083428651,29.5333606573844,-18.7824420081377));
#32413=CARTESIAN_POINT('Ctrl Pts',(33.4887791610293,29.5333623350577,-18.7824387839385));
#32414=CARTESIAN_POINT('Ctrl Pts',(33.4518540159975,29.5333636750843,-18.7824362086382));
#32415=CARTESIAN_POINT('Ctrl Pts',(33.415863041895,29.5333649012575,-18.7824337706412));
#32416=CARTESIAN_POINT('Ctrl Pts',(33.3809178973935,29.5333661853238,-18.7824311829815));
#32417=CARTESIAN_POINT('Ctrl Pts',(33.3430135141806,29.533367578128,-18.7824283761925));
#32418=CARTESIAN_POINT('Ctrl Pts',(33.3063394413794,29.533369038868,-18.782425393611));
#32419=CARTESIAN_POINT('Ctrl Pts',(33.2709744549996,29.5333707165148,-18.782421984424));
#32420=CARTESIAN_POINT('Ctrl Pts',(33.2337091833701,29.5333724843074,-18.7824183920493));
#32421=CARTESIAN_POINT('Ctrl Pts',(33.1978968817055,29.5333744922841,-18.7824143270743));
#32422=CARTESIAN_POINT('Ctrl Pts',(33.1635680440121,29.5333768470907,-18.7824096072585));
#32423=CARTESIAN_POINT('Ctrl Pts',(33.1258517952633,29.5333794342587,-18.7824044217132));
#32424=CARTESIAN_POINT('Ctrl Pts',(33.0899258346456,29.5333824396273,-18.7823984464624));
#32425=CARTESIAN_POINT('Ctrl Pts',(33.0557653924634,29.5333859335647,-18.7823915566589));
#32426=CARTESIAN_POINT('Ctrl Pts',(33.0368719876719,29.5333878659862,-18.7823877460571));
#32427=CARTESIAN_POINT('Ctrl Pts',(33.0185175726606,29.5333899466911,-18.7823836576174));
#32428=CARTESIAN_POINT('Ctrl Pts',(33.0006913488414,29.533392180445,-18.7823792819583));
#32429=CARTESIAN_POINT('Ctrl Pts',(32.9433364917301,29.5333993674205,-18.782365203525));
#32430=CARTESIAN_POINT('Ctrl Pts',(32.8893232017973,29.5332829792511,-18.7825476275078));
#32431=CARTESIAN_POINT('Ctrl Pts',(32.8382230275391,29.5330947066423,-18.7828441878577));
#32432=CARTESIAN_POINT('Ctrl Pts',(32.7810653123534,29.5328841157333,-18.7831759032042));
#32433=CARTESIAN_POINT('Ctrl Pts',(32.7275524566167,29.5325833908839,-18.783650731462));
#32434=CARTESIAN_POINT('Ctrl Pts',(32.6770430178925,29.5322363386496,-18.7841988325575));
#32435=CARTESIAN_POINT('Ctrl Pts',(32.6227203150995,29.5318630853359,-18.7847883131311));
#32436=CARTESIAN_POINT('Ctrl Pts',(32.5718714570969,29.5314358212364,-18.7854632228815));
#32437=CARTESIAN_POINT('Ctrl Pts',(32.5236533104246,29.5309832901802,-18.7861776881423));
#32438=CARTESIAN_POINT('Ctrl Pts',(32.4718100170281,29.5304967368401,-18.7869458684789));
#32439=CARTESIAN_POINT('Ctrl Pts',(32.4230076636094,29.5299805545515,-18.787760443828));
#32440=CARTESIAN_POINT('Ctrl Pts',(32.3761512171914,29.5294487411366,-18.7885990065863));
#32441=CARTESIAN_POINT('Ctrl Pts',(32.3248096591116,29.5288660223985,-18.7895178367975));
#32442=CARTESIAN_POINT('Ctrl Pts',(32.2758043950059,29.5282641700435,-18.7904660498706));
#32443=CARTESIAN_POINT('Ctrl Pts',(32.2276418899913,29.5276429422444,-18.7914438965952));
#32444=CARTESIAN_POINT('Ctrl Pts',(32.1780484879523,29.5270032579093,-18.7924507949227));
#32445=CARTESIAN_POINT('Ctrl Pts',(32.1293485207493,29.5263425803878,-18.7934898288216));
#32446=CARTESIAN_POINT('Ctrl Pts',(32.0798596721981,29.5256485080419,-18.7945806299647));
#32447=CARTESIAN_POINT('Ctrl Pts',(32.0310319727761,29.5249637081956,-18.795656858487));
#32448=CARTESIAN_POINT('Ctrl Pts',(31.9814363679965,29.5242459918055,-18.7967841293548));
#32449=CARTESIAN_POINT('Ctrl Pts',(31.9294088356335,29.5234781937103,-18.7979897024647));
#32450=CARTESIAN_POINT('Ctrl Pts',(31.8980169361542,29.5230149266759,-18.7987171102076));
#32451=CARTESIAN_POINT('Ctrl Pts',(31.8657387723059,29.5225333465274,-18.7994731533957));
#32452=CARTESIAN_POINT('Ctrl Pts',(31.832199550689,29.5220297162343,-18.8002637757389));
#32453=CARTESIAN_POINT('Ctrl Pts',(31.7313430769547,29.5205152393625,-18.8026412722264));
#32454=CARTESIAN_POINT('Ctrl Pts',(31.6280303063014,29.5189339810999,-18.8051208616254));
#32455=CARTESIAN_POINT('Ctrl Pts',(31.5230436306591,29.5173797888791,-18.8075570016555));
#32456=CARTESIAN_POINT('Ctrl Pts',(31.4165412834615,29.5158031590972,-18.8100283117502));
#32457=CARTESIAN_POINT('Ctrl Pts',(31.308316179973,29.514255268772,-18.8124534992281));
#32458=CARTESIAN_POINT('Ctrl Pts',(31.1992361907457,29.5128402023346,-18.8146708525442));
#32459=CARTESIAN_POINT('Ctrl Pts',(31.1417800802777,29.5120948391005,-18.815838807345));
#32460=CARTESIAN_POINT('Ctrl Pts',(31.0840876501121,29.5113863470817,-18.8169490671259));
#32461=CARTESIAN_POINT('Ctrl Pts',(31.0262914624598,29.5107292754507,-18.8179790464239));
#32462=CARTESIAN_POINT('Ctrl Pts',(30.9238422517516,29.5095645538192,-18.819804782176));
#32463=CARTESIAN_POINT('Ctrl Pts',(30.8210652493991,29.508562595471,-18.8213763518942));
#32464=CARTESIAN_POINT('Ctrl Pts',(30.7187655025437,29.5078108353848,-18.822555692875));
#32465=CARTESIAN_POINT('Ctrl Pts',(30.6466529304573,29.5072809088202,-18.8233870274004));
#32466=CARTESIAN_POINT('Ctrl Pts',(30.574778287816,29.5068750511295,-18.8240238694395));
#32467=CARTESIAN_POINT('Ctrl Pts',(30.5034323931867,29.5066169475222,-18.8244289958229));
#32468=CARTESIAN_POINT('Ctrl Pts',(30.500673116597,29.5066069654589,-18.8244446639388));
#32469=CARTESIAN_POINT('Ctrl Pts',(30.497914631651,29.5065972035123,-18.8244599868899));
#32470=CARTESIAN_POINT('Ctrl Pts',(30.4951569508121,29.5065876629555,-18.8244749626662));
#32471=CARTESIAN_POINT('',(30.5,31.0097594187194,-16.229443021655));
#32472=CARTESIAN_POINT('Origin',(30.5,0.,0.));
#32473=CARTESIAN_POINT('Ctrl Pts',(30.504907630814,31.0091238687318,-16.2304573503026));
#32474=CARTESIAN_POINT('Ctrl Pts',(30.5973062294344,31.0094328533547,-16.2298682766552));
#32475=CARTESIAN_POINT('Ctrl Pts',(30.689059158586,31.0099692677028,-16.2288427503286));
#32476=CARTESIAN_POINT('Ctrl Pts',(30.7806364364919,31.0106763092383,-16.2274919709621));
#32477=CARTESIAN_POINT('Ctrl Pts',(30.8441456090292,31.0111666450935,-16.2265552005993));
#32478=CARTESIAN_POINT('Ctrl Pts',(30.9075713010183,31.0117394593183,-16.2254611740684));
#32479=CARTESIAN_POINT('Ctrl Pts',(30.9710816356703,31.0123798375508,-16.2242390174924));
#32480=CARTESIAN_POINT('Ctrl Pts',(31.0734991469994,31.013412519007,-16.2222681534487));
#32481=CARTESIAN_POINT('Ctrl Pts',(31.1761345288067,31.0146205155167,-16.2199648111636));
#32482=CARTESIAN_POINT('Ctrl Pts',(31.2798100568469,31.0159286966544,-16.2174702047238));
#32483=CARTESIAN_POINT('Ctrl Pts',(31.3828326297147,31.0172286387828,-16.2149913094765));
#32484=CARTESIAN_POINT('Ctrl Pts',(31.4868822244369,31.0186283615542,-16.2123218973813));
#32485=CARTESIAN_POINT('Ctrl Pts',(31.5928140565652,31.020057669606,-16.2095937955789));
#32486=CARTESIAN_POINT('Ctrl Pts',(31.6516194621143,31.0208511142011,-16.2080793581369));
#32487=CARTESIAN_POINT('Ctrl Pts',(31.7110057676108,31.0216536678951,-16.2065468518027));
#32488=CARTESIAN_POINT('Ctrl Pts',(31.7711259776529,31.0224523036437,-16.2050208141949));
#32489=CARTESIAN_POINT('Ctrl Pts',(31.8409078613426,31.0233792848848,-16.2032495333099));
#32490=CARTESIAN_POINT('Ctrl Pts',(31.9056298453963,31.0242198767433,-16.2016434584277));
#32491=CARTESIAN_POINT('Ctrl Pts',(31.9658749467864,31.0249744961546,-16.2002018139142));
#32492=CARTESIAN_POINT('Ctrl Pts',(32.0341046687228,31.0258291295008,-16.1985691001829));
#32493=CARTESIAN_POINT('Ctrl Pts',(32.096591829894,31.026574015819,-16.1971462744691));
#32494=CARTESIAN_POINT('Ctrl Pts',(32.1542461945013,31.0272242625029,-16.1959042389539));
#32495=CARTESIAN_POINT('Ctrl Pts',(32.215166595352,31.0279113447196,-16.1945918439258));
#32496=CARTESIAN_POINT('Ctrl Pts',(32.2706916712563,31.0284933558527,-16.1934801514051));
#32497=CARTESIAN_POINT('Ctrl Pts',(32.3219582775163,31.0289937114781,-16.1925241206212));
#32498=CARTESIAN_POINT('Ctrl Pts',(32.3761916324787,31.0295230221975,-16.1915127652646));
#32499=CARTESIAN_POINT('Ctrl Pts',(32.4256599862246,31.0299613681536,-16.1906748064835));
#32500=CARTESIAN_POINT('Ctrl Pts',(32.4717693483811,31.0303343957023,-16.1899610544418));
#32501=CARTESIAN_POINT('Ctrl Pts',(32.5215332003089,31.0307369882959,-16.1891907325537));
#32502=CARTESIAN_POINT('Ctrl Pts',(32.5673849287969,31.0310638203075,-16.1885644631731));
#32503=CARTESIAN_POINT('Ctrl Pts',(32.6111519417734,31.0313387615313,-16.1880367365758));
#32504=CARTESIAN_POINT('Ctrl Pts',(32.6551741210766,31.0316153056916,-16.1875059332764));
#32505=CARTESIAN_POINT('Ctrl Pts',(32.6970878717853,31.0318395012596,-16.1870745377529));
#32506=CARTESIAN_POINT('Ctrl Pts',(32.7388013470543,31.0320241553173,-16.1867185738399));
#32507=CARTESIAN_POINT('Ctrl Pts',(32.7801521457897,31.0322072039059,-16.1863657048443));
#32508=CARTESIAN_POINT('Ctrl Pts',(32.8213062770032,31.0323516104907,-16.1860865454659));
#32509=CARTESIAN_POINT('Ctrl Pts',(32.8641640035307,31.0324560971769,-16.1858844594634));
#32510=CARTESIAN_POINT('Ctrl Pts',(32.9038200784545,31.0325527782703,-16.1856974701314));
#32511=CARTESIAN_POINT('Ctrl Pts',(32.9449347772916,31.032615465502,-16.1855761117061));
#32512=CARTESIAN_POINT('Ctrl Pts',(32.9890474705834,31.0326287580452,-16.1855509840874));
#32513=CARTESIAN_POINT('Ctrl Pts',(32.9926089293383,31.0326298312249,-16.1855489553974));
#32514=CARTESIAN_POINT('Ctrl Pts',(32.9961899495414,31.0326305730127,-16.1855475722577));
#32515=CARTESIAN_POINT('Ctrl Pts',(32.9997913521115,31.0326309700538,-16.1855468609619));
#32516=CARTESIAN_POINT('Ctrl Pts',(33.0362292496772,31.0326349871946,-16.1855396642873));
#32517=CARTESIAN_POINT('Ctrl Pts',(33.074092292112,31.0326386992185,-16.1855331333215));
#32518=CARTESIAN_POINT('Ctrl Pts',(33.1141439185631,31.0326422490868,-16.1855273500631));
#32519=CARTESIAN_POINT('Ctrl Pts',(33.2461674547434,31.0326539506383,-16.1855082865123));
#32520=CARTESIAN_POINT('Ctrl Pts',(33.3721931286569,31.0326588963953,-16.1855003220479));
#32521=CARTESIAN_POINT('Ctrl Pts',(33.4993879207449,31.0326635427516,-16.185492813855));
#32522=CARTESIAN_POINT('Ctrl Pts',(33.6627849160625,31.0326695115547,-16.1854831686789));
#32523=CARTESIAN_POINT('Ctrl Pts',(33.828111247454,31.0326749862723,-16.1854742764644));
#32524=CARTESIAN_POINT('Ctrl Pts',(33.9929845306744,31.0326833946005,-16.1854606405094));
#32525=CARTESIAN_POINT('Ctrl Pts',(34.3227310971152,31.0327002112569,-16.1854333685993));
#32526=CARTESIAN_POINT('Ctrl Pts',(34.6506654708719,31.032728762356,-16.185387121727));
#32527=CARTESIAN_POINT('Ctrl Pts',(34.979269363621,31.032748004237,-16.1853559472169));
#32528=CARTESIAN_POINT('Ctrl Pts',(35.3078732563701,31.0327672461181,-16.1853247727068));
#32529=CARTESIAN_POINT('Ctrl Pts',(35.6371466681116,31.032777178781,-16.185308670559));
#32530=CARTESIAN_POINT('Ctrl Pts',(35.9662682695208,31.0327855310262,-16.1852951338217));
#32531=CARTESIAN_POINT('Ctrl Pts',(36.29538987093,31.0327938832714,-16.1852815970843));
#32532=CARTESIAN_POINT('Ctrl Pts',(36.6243596620069,31.0328006550988,-16.1852706257574));
#32533=CARTESIAN_POINT('Ctrl Pts',(36.9532592751492,31.0328145551759,-16.185248102247));
#32534=CARTESIAN_POINT('Ctrl Pts',(38.102326278026,31.0328631174705,-16.1851694125146));
#32535=CARTESIAN_POINT('Ctrl Pts',(39.2505367075415,31.0329986853002,-16.184949719878));
#32536=CARTESIAN_POINT('Ctrl Pts',(40.4000986012038,31.0330322281526,-16.1848953623403));
#32537=CARTESIAN_POINT('Ctrl Pts',(6.89999999997365,11.0276873985587,0.168526548676475));
#32538=CARTESIAN_POINT('Ctrl Pts',(6.99168932310453,11.0290491215116,0.107121039164007));
#32539=CARTESIAN_POINT('Ctrl Pts',(7.08383940291242,11.0299018391088,0.0458098125994608));
#32540=CARTESIAN_POINT('Ctrl Pts',(8.15761824498006,11.0337651740187,-0.664186592400576));
#32541=CARTESIAN_POINT('Ctrl Pts',(9.16607857437499,10.9699676285446,-1.30870352701556));
#32542=CARTESIAN_POINT('Ctrl Pts',(11.2535171643192,10.77603305676,-2.47376106241928));
#32543=CARTESIAN_POINT('Ctrl Pts',(12.2576790632369,10.6330057282435,-3.00237606292525));
#32544=CARTESIAN_POINT('Ctrl Pts',(14.3563663857894,10.3307260661656,-3.944470058834));
#32545=CARTESIAN_POINT('Ctrl Pts',(15.3658129161116,10.1540434041659,-4.36032593857962));
#32546=CARTESIAN_POINT('Ctrl Pts',(17.4727193021212,9.82334300624284,-5.08193366885832));
#32547=CARTESIAN_POINT('Ctrl Pts',(18.4888802671462,9.6488422591121,-5.39169279079136));
#32548=CARTESIAN_POINT('Ctrl Pts',(19.8473882183426,9.45778984314828,-5.72385817850078));
#32549=CARTESIAN_POINT('Ctrl Pts',(20.3451395577184,9.38741838105895,-5.84063156394592));
#32550=CARTESIAN_POINT('Ctrl Pts',(21.119864121141,9.28201599203951,-6.00690103675049));
#32551=CARTESIAN_POINT('Ctrl Pts',(21.9116430735678,9.18172875488038,-6.15921075032183));
#32552=CARTESIAN_POINT('Ctrl Pts',(22.4533884343746,9.12054551137776,-6.25063668203688));
#32553=CARTESIAN_POINT('Ctrl Pts',(22.8546099577479,9.07881438233612,-6.31320896750581));
#32554=CARTESIAN_POINT('Ctrl Pts',(23.1058218650381,9.05298395410356,-6.35118260107245));
#32555=CARTESIAN_POINT('Ctrl Pts',(23.6175153199788,9.00245668094437,-6.42382403760964));
#32556=CARTESIAN_POINT('Ctrl Pts',(24.1364702886545,8.95485371029555,-6.49007583237978));
#32557=CARTESIAN_POINT('Ctrl Pts',(24.6629181373246,8.91145225308144,-6.54944423929279));
#32558=CARTESIAN_POINT('Ctrl Pts',(25.0606678571037,8.88140293076164,-6.59024788291775));
#32559=CARTESIAN_POINT('Ctrl Pts',(25.3945416155882,8.85873533710264,-6.6209922830971));
#32560=CARTESIAN_POINT('Ctrl Pts',(25.6627586119464,8.84221409068033,-6.64352323130153));
#32561=CARTESIAN_POINT('Ctrl Pts',(25.7972076165425,8.83452216013014,-6.65408072739387));
#32562=CARTESIAN_POINT('Ctrl Pts',(26.3824137782946,8.80240169886323,-6.69837697633853));
#32563=CARTESIAN_POINT('Ctrl Pts',(27.4369717967155,8.76563881905854,-6.74704662082203));
#32564=CARTESIAN_POINT('Ctrl Pts',(28.4593635146677,8.74917816753949,-6.76713562537254));
#32565=CARTESIAN_POINT('Ctrl Pts',(29.0427481469891,8.73952198264544,-6.77974505298723));
#32566=CARTESIAN_POINT('Ctrl Pts',(29.2174939164952,8.73701514175018,-6.78306424239323));
#32567=CARTESIAN_POINT('Ctrl Pts',(29.5607048332279,8.73336568489193,-6.78786835107262));
#32568=CARTESIAN_POINT('Ctrl Pts',(29.9899637006214,8.73093988338428,-6.79106253935677));
#32569=CARTESIAN_POINT('Ctrl Pts',(30.5003627545718,8.73068255391872,-6.79139754852948));
#32570=CARTESIAN_POINT('Ctrl Pts',(31.5152290141054,8.73381293113859,-6.7872875501941));
#32571=CARTESIAN_POINT('Ctrl Pts',(32.346385618228,8.74063107149335,-6.77838967797266));
#32572=CARTESIAN_POINT('Ctrl Pts',(33.1616392309915,8.74062146997074,-6.77840182636606));
#32573=CARTESIAN_POINT('Ctrl Pts',(33.4928689770884,8.74062052628883,-6.77840284181041));
#32574=CARTESIAN_POINT('Ctrl Pts',(33.9856875201801,8.74061852020513,-6.77840526161275));
#32575=CARTESIAN_POINT('Ctrl Pts',(34.4799569296089,8.74061713883255,-6.7784068708528));
#32576=CARTESIAN_POINT('Ctrl Pts',(35.1382080085716,8.74061527897129,-6.778409075901));
#32577=CARTESIAN_POINT('Ctrl Pts',(35.9613703496106,8.74061266742265,-6.7784121544085));
#32578=CARTESIAN_POINT('Ctrl Pts',(37.9364530322258,8.74060999527038,-6.77841531264167));
#32579=CARTESIAN_POINT('Ctrl Pts',(39.5833333333333,8.74059347982546,-6.7784348060232));
#32580=CARTESIAN_POINT('Ctrl Pts',(40.9,8.74059347982546,-6.7784348060232));
#32581=CARTESIAN_POINT('Ctrl Pts',(6.65963435785827,15.5421695279122,0.914290744262172));
#32582=CARTESIAN_POINT('Ctrl Pts',(6.7513219377677,15.5478000748543,0.82766409749893));
#32583=CARTESIAN_POINT('Ctrl Pts',(6.84347928233528,15.552705535984,0.741125593738214));
#32584=CARTESIAN_POINT('Ctrl Pts',(7.91768245328712,15.6010379387116,-0.26091214146805));
#32585=CARTESIAN_POINT('Ctrl Pts',(8.92716941433652,15.5498192559038,-1.17337698529147));
#32586=CARTESIAN_POINT('Ctrl Pts',(11.0226592374973,15.3445243615387,-2.83406080960164));
#32587=CARTESIAN_POINT('Ctrl Pts',(12.028922251309,15.174357849642,-3.58841078209879));
#32588=CARTESIAN_POINT('Ctrl Pts',(14.1441326723881,14.8006104561251,-4.94359337154892));
#32589=CARTESIAN_POINT('Ctrl Pts',(15.1576282381579,14.5754503759515,-5.54148857510366));
#32590=CARTESIAN_POINT('Ctrl Pts',(17.2903455772588,14.1464770374584,-6.58799131832697));
#32591=CARTESIAN_POINT('Ctrl Pts',(18.3126565164254,13.9174993841978,-7.03615941125111));
#32592=CARTESIAN_POINT('Ctrl Pts',(19.6943886098338,13.6636269320846,-7.52140607073201));
#32593=CARTESIAN_POINT('Ctrl Pts',(20.1963997689949,13.5705283753709,-7.69105316997363));
#32594=CARTESIAN_POINT('Ctrl Pts',(20.9820476354982,13.4299327266448,-7.93384577456641));
#32595=CARTESIAN_POINT('Ctrl Pts',(21.7860719497258,13.2956844767357,-8.15658902665418));
#32596=CARTESIAN_POINT('Ctrl Pts',(22.337913112583,13.2134517389134,-8.29065006793576));
#32597=CARTESIAN_POINT('Ctrl Pts',(22.7470242103181,13.1573095336481,-8.38247788994951));
#32598=CARTESIAN_POINT('Ctrl Pts',(23.0012838485784,13.1227286630507,-8.43794163853499));
#32599=CARTESIAN_POINT('Ctrl Pts',(23.5207560883432,13.0548326909721,-8.54431696039332));
#32600=CARTESIAN_POINT('Ctrl Pts',(24.0478165510037,12.9907421048666,-8.64139629793569));
#32601=CARTESIAN_POINT('Ctrl Pts',(24.5834508086858,12.9321620155411,-8.72854413973125));
#32602=CARTESIAN_POINT('Ctrl Pts',(24.9884814516724,12.8915554305395,-8.78849484453724));
#32603=CARTESIAN_POINT('Ctrl Pts',(25.328876176695,12.8608881947636,-8.83370307828861));
#32604=CARTESIAN_POINT('Ctrl Pts',(25.6025411192576,12.8385223247211,-8.86685769924429));
#32605=CARTESIAN_POINT('Ctrl Pts',(25.7397909478799,12.8281059147068,-8.88239886754126));
#32606=CARTESIAN_POINT('Ctrl Pts',(26.337634174326,12.7845927902169,-8.94762125696996));
#32607=CARTESIAN_POINT('Ctrl Pts',(27.4152541470276,12.7347557261564,-9.01924678134852));
#32608=CARTESIAN_POINT('Ctrl Pts',(28.4429499146132,12.7126826807293,-9.04845162691344));
#32609=CARTESIAN_POINT('Ctrl Pts',(29.025973512459,12.6997781188675,-9.06676270853365));
#32610=CARTESIAN_POINT('Ctrl Pts',(29.2042686472713,12.6963761571783,-9.07165323227904));
#32611=CARTESIAN_POINT('Ctrl Pts',(29.5518704410185,12.6914548812215,-9.07868995890013));
#32612=CARTESIAN_POINT('Ctrl Pts',(29.9865605489543,12.6881801081656,-9.0833711721763));
#32613=CARTESIAN_POINT('Ctrl Pts',(30.5013181269546,12.687836307306,-9.08385656546478));
#32614=CARTESIAN_POINT('Ctrl Pts',(31.5221463919967,12.692041007367,-9.07785413361794));
#32615=CARTESIAN_POINT('Ctrl Pts',(32.3518561954418,12.7011306199595,-9.06494609970921));
#32616=CARTESIAN_POINT('Ctrl Pts',(33.1604291208177,12.7011133788387,-9.06496486760966));
#32617=CARTESIAN_POINT('Ctrl Pts',(33.492519059067,12.7011117013819,-9.06496624091916));
#32618=CARTESIAN_POINT('Ctrl Pts',(33.9849476449336,12.7011081104537,-9.06496984963707));
#32619=CARTESIAN_POINT('Ctrl Pts',(34.4794328720439,12.7011056432242,-9.06497218408094));
#32620=CARTESIAN_POINT('Ctrl Pts',(35.1376484147356,12.7011023177079,-9.06497542847038));
#32621=CARTESIAN_POINT('Ctrl Pts',(35.9609115545804,12.7010976498373,-9.06497993729913));
#32622=CARTESIAN_POINT('Ctrl Pts',(37.9360269889122,12.7010928728514,-9.06498457262958));
#32623=CARTESIAN_POINT('Ctrl Pts',(39.5833333333333,12.701063350837,-9.06501315216909));
#32624=CARTESIAN_POINT('Ctrl Pts',(40.9,12.701063350837,-9.06501315216909));
#32625=CARTESIAN_POINT('Ctrl Pts',(6.47499700785697,23.4452408248497,2.19830497971403));
#32626=CARTESIAN_POINT('Ctrl Pts',(6.56578730943226,23.4579749263878,2.06870104448402));
#32627=CARTESIAN_POINT('Ctrl Pts',(6.65702462351448,23.4696212195475,1.93921681262018));
#32628=CARTESIAN_POINT('Ctrl Pts',(7.72175305647137,23.5924911125725,0.437116228582368));
#32629=CARTESIAN_POINT('Ctrl Pts',(8.72281885180382,23.562968194923,-0.937680140908612));
#32630=CARTESIAN_POINT('Ctrl Pts',(10.7949492361907,23.3400040819285,-3.44026704375966));
#32631=CARTESIAN_POINT('Ctrl Pts',(11.7960921547002,23.1244337632637,-4.58695803318564));
#32632=CARTESIAN_POINT('Ctrl Pts',(13.8958332645754,22.6316660291752,-6.64967501166335));
#32633=CARTESIAN_POINT('Ctrl Pts',(14.90655296446,22.3241101177864,-7.56603922905965));
#32634=CARTESIAN_POINT('Ctrl Pts',(17.0410718223018,21.7268962408645,-9.17994203101702));
#32635=CARTESIAN_POINT('Ctrl Pts',(18.0654584152639,21.4035033181339,-9.87337110606603));
#32636=CARTESIAN_POINT('Ctrl Pts',(19.4655915747002,21.0382396447148,-10.6334003056859));
#32637=CARTESIAN_POINT('Ctrl Pts',(19.9714665789849,20.9051898734593,-10.8971713557552));
#32638=CARTESIAN_POINT('Ctrl Pts',(20.7678306953019,20.7020007981629,-11.2774874271219));
#32639=CARTESIAN_POINT('Ctrl Pts',(21.5858101282049,20.5068169170513,-11.6277425327431));
#32640=CARTESIAN_POINT('Ctrl Pts',(22.1506096305012,20.3863209191721,-11.8398576536859));
#32641=CARTESIAN_POINT('Ctrl Pts',(22.5704199924792,20.3038374401207,-11.9854171937934));
#32642=CARTESIAN_POINT('Ctrl Pts',(22.8289065956907,20.2535349220293,-12.0724797867542));
#32643=CARTESIAN_POINT('Ctrl Pts',(23.3593853239227,20.1541718428526,-12.2402701514191));
#32644=CARTESIAN_POINT('Ctrl Pts',(23.8985486588058,20.0601195256968,-12.3936552183108));
#32645=CARTESIAN_POINT('Ctrl Pts',(24.4483714419233,19.9737860075934,-12.5318087211867));
#32646=CARTESIAN_POINT('Ctrl Pts',(24.8648919059683,19.9138158121695,-12.6269879069122));
#32647=CARTESIAN_POINT('Ctrl Pts',(25.2158455690755,19.8684065291874,-12.6989260386038));
#32648=CARTESIAN_POINT('Ctrl Pts',(25.4984343217206,19.835239602927,-12.7517388774023));
#32649=CARTESIAN_POINT('Ctrl Pts',(25.6403132052063,19.819776905443,-12.7765150372188));
#32650=CARTESIAN_POINT('Ctrl Pts',(26.259216041408,19.7551088720196,-12.880614699098));
#32651=CARTESIAN_POINT('Ctrl Pts',(27.3768446537004,19.681063586732,-12.994818613011));
#32652=CARTESIAN_POINT('Ctrl Pts',(28.4139434096804,19.6491350216628,-13.040069216748));
#32653=CARTESIAN_POINT('Ctrl Pts',(28.9963902080607,19.6305403234116,-13.068390840642));
#32654=CARTESIAN_POINT('Ctrl Pts',(29.1808784030088,19.62547738919,-13.0761959447011));
#32655=CARTESIAN_POINT('Ctrl Pts',(29.5361613355605,19.6182496508376,-13.0872826938044));
#32656=CARTESIAN_POINT('Ctrl Pts',(29.9803701492973,19.6134266676609,-13.0946820190498));
#32657=CARTESIAN_POINT('Ctrl Pts',(30.502764565205,19.6129305494836,-13.0954354949455));
#32658=CARTESIAN_POINT('Ctrl Pts',(31.5340441540657,19.6190493314859,-13.0860712826797));
#32659=CARTESIAN_POINT('Ctrl Pts',(32.3612933570749,19.6320590316267,-13.0662692307128));
#32660=CARTESIAN_POINT('Ctrl Pts',(33.1582057305722,19.6320151866218,-13.0663352315321));
#32661=CARTESIAN_POINT('Ctrl Pts',(33.4918052160808,19.6320107493385,-13.0663415440457));
#32662=CARTESIAN_POINT('Ctrl Pts',(33.9835585756086,19.6320015037507,-13.0663552182345));
#32663=CARTESIAN_POINT('Ctrl Pts',(34.4784268233885,19.6319950964453,-13.0663645784941));
#32664=CARTESIAN_POINT('Ctrl Pts',(35.1365871092732,19.6319864972548,-13.0663772185058));
#32665=CARTESIAN_POINT('Ctrl Pts',(35.9600364992905,19.631974409872,-13.0663949498221));
#32666=CARTESIAN_POINT('Ctrl Pts',(37.935219274406,19.6319620479287,-13.0664131007023));
#32667=CARTESIAN_POINT('Ctrl Pts',(39.5833333333333,19.6318856251071,-13.0665252579244));
#32668=CARTESIAN_POINT('Ctrl Pts',(40.9,19.6318856251071,-13.0665252579244));
#32669=CARTESIAN_POINT('Ctrl Pts',(6.39840282685635,31.3636440442398,3.36386536347515));
#32670=CARTESIAN_POINT('Ctrl Pts',(6.48879582230594,31.3828291635015,3.19164073503352));
#32671=CARTESIAN_POINT('Ctrl Pts',(6.57961766269115,31.4005708453189,3.01959979440375));
#32672=CARTESIAN_POINT('Ctrl Pts',(7.64032554406628,31.5903744166847,1.0214771742003));
#32673=CARTESIAN_POINT('Ctrl Pts',(8.63867106160223,31.5754173772483,-0.811297807542591));
#32674=CARTESIAN_POINT('Ctrl Pts',(10.6964316380006,31.3261515036618,-4.13353910931636));
#32675=CARTESIAN_POINT('Ctrl Pts',(11.6947290441859,31.0615534966588,-5.66648609020815));
#32676=CARTESIAN_POINT('Ctrl Pts',(13.7762263687762,30.4500782098735,-8.40637303045945));
#32677=CARTESIAN_POINT('Ctrl Pts',(14.7826773906134,30.0602543273649,-9.63313444048393));
#32678=CARTESIAN_POINT('Ctrl Pts',(16.8988982405362,29.3025485110513,-11.7841821047735));
#32679=CARTESIAN_POINT('Ctrl Pts',(17.9188263508252,28.8873179990429,-12.7156877051221));
#32680=CARTESIAN_POINT('Ctrl Pts',(19.3136620513073,28.4161739072999,-13.7379571249216));
#32681=CARTESIAN_POINT('Ctrl Pts',(19.8189838754923,28.2441169214324,-14.0939758439964));
#32682=CARTESIAN_POINT('Ctrl Pts',(20.6150001505384,27.9803060047161,-14.6080226620617));
#32683=CARTESIAN_POINT('Ctrl Pts',(21.4350390683301,27.7255808745093,-15.0835002485374));
#32684=CARTESIAN_POINT('Ctrl Pts',(22.0037815933943,27.5672808319297,-15.3731124530265));
#32685=CARTESIAN_POINT('Ctrl Pts',(22.4278524797961,27.4584837184542,-15.5725968076267));
#32686=CARTESIAN_POINT('Ctrl Pts',(22.688147887321,27.3924576319504,-15.6914147925572));
#32687=CARTESIAN_POINT('Ctrl Pts',(23.223810634427,27.2614400973337,-15.921268075794));
#32688=CARTESIAN_POINT('Ctrl Pts',(23.7696978745004,27.1369441741205,-16.1321064141347));
#32689=CARTESIAN_POINT('Ctrl Pts',(24.3285206801332,27.0220641661339,-16.3229204338608));
#32690=CARTESIAN_POINT('Ctrl Pts',(24.7529653140503,26.9419913350361,-16.4547973514758));
#32691=CARTESIAN_POINT('Ctrl Pts',(25.1117719491783,26.8811074137508,-16.5548637960119));
#32692=CARTESIAN_POINT('Ctrl Pts',(25.4013553254923,26.8365068705618,-16.6285198436921));
#32693=CARTESIAN_POINT('Ctrl Pts',(25.5469791293169,26.8156703264604,-16.6631374284085));
#32694=CARTESIAN_POINT('Ctrl Pts',(26.1832292898986,26.7283606594224,-16.8088431266916));
#32695=CARTESIAN_POINT('Ctrl Pts',(27.3386864567866,26.6279357083784,-16.9694451045117));
#32696=CARTESIAN_POINT('Ctrl Pts',(28.3853135289693,26.586099013527,-17.0308214554547));
#32697=CARTESIAN_POINT('Ctrl Pts',(28.9671494424547,26.5618106446085,-17.0691585340133));
#32698=CARTESIAN_POINT('Ctrl Pts',(29.1577497745604,26.5549253720647,-17.0801578267591));
#32699=CARTESIAN_POINT('Ctrl Pts',(29.5206667656999,26.5452518307314,-17.095535221436));
#32700=CARTESIAN_POINT('Ctrl Pts',(29.9743609805095,26.5387742795116,-17.1058350294712));
#32701=CARTESIAN_POINT('Ctrl Pts',(30.5043929318941,26.5381249904398,-17.1068574997827));
#32702=CARTESIAN_POINT('Ctrl Pts',(31.5460952643804,26.5462202887399,-17.0940221862974));
#32703=CARTESIAN_POINT('Ctrl Pts',(32.3708379684223,26.5630634070366,-17.0674707682792));
#32704=CARTESIAN_POINT('Ctrl Pts',(33.1560659395073,26.5629740474711,-17.0676145179389));
#32705=CARTESIAN_POINT('Ctrl Pts',(33.4911715963805,26.5629648505726,-17.0676289242213));
#32706=CARTESIAN_POINT('Ctrl Pts',(33.9822440621775,26.5629459056337,-17.0676591426917));
#32707=CARTESIAN_POINT('Ctrl Pts',(34.4774910986523,26.5629327280363,-17.0676800396183));
#32708=CARTESIAN_POINT('Ctrl Pts',(35.1355906516825,26.5629150749568,-17.0677081152075));
#32709=CARTESIAN_POINT('Ctrl Pts',(35.9592185001008,26.5628902459987,-17.0677475655254));
#32710=CARTESIAN_POINT('Ctrl Pts',(37.9344606912907,26.5628648600815,-17.067787918432));
#32711=CARTESIAN_POINT('Ctrl Pts',(39.5833333333333,26.5627078993772,-17.0680373636797));
#32712=CARTESIAN_POINT('Ctrl Pts',(40.9,26.5627078993772,-17.0680373636797));
#32713=CARTESIAN_POINT('Ctrl Pts',(6.37427268165564,34.7583359408307,3.85496595036636));
#32714=CARTESIAN_POINT('Ctrl Pts',(6.46448755772839,34.7802475524424,3.66446375246399));
#32715=CARTESIAN_POINT('Ctrl Pts',(6.55512331969025,34.8005635888992,3.47417181608893));
#32716=CARTESIAN_POINT('Ctrl Pts',(7.61410548625795,35.0185788676571,1.26339052014804));
#32717=CARTESIAN_POINT('Ctrl Pts',(8.61145388480624,35.0093532870147,-0.76560245720769));
#32718=CARTESIAN_POINT('Ctrl Pts',(10.6635149436019,34.747974440135,-4.43910992978125));
#32719=CARTESIAN_POINT('Ctrl Pts',(11.6608017032625,34.4619345886989,-6.13747453196185));
#32720=CARTESIAN_POINT('Ctrl Pts',(13.7353542747945,33.7990269238398,-9.16685810272324));
#32721=CARTESIAN_POINT('Ctrl Pts',(14.7402715202386,33.3736740493576,-10.526297955279));
#32722=CARTESIAN_POINT('Ctrl Pts',(16.8491677832147,32.5473921410153,-12.9054531131771));
#32723=CARTESIAN_POINT('Ctrl Pts',(17.8672809631136,32.092886041556,-13.9382203331611));
#32724=CARTESIAN_POINT('Ctrl Pts',(19.2587625104673,31.577179869867,-15.0707179501981));
#32725=CARTESIAN_POINT('Ctrl Pts',(19.7635899403542,31.3885503410944,-15.4658689812884));
#32726=CARTESIAN_POINT('Ctrl Pts',(20.5586991602297,31.0991569516509,-16.0362969262867));
#32727=CARTESIAN_POINT('Ctrl Pts',(21.3785272493018,30.819343278526,-16.564533786793));
#32728=CARTESIAN_POINT('Ctrl Pts',(21.9479176287994,30.6451300260617,-16.8867906552356));
#32729=CARTESIAN_POINT('Ctrl Pts',(22.3729695502115,30.525234440013,-17.1090467735268));
#32730=CARTESIAN_POINT('Ctrl Pts',(22.6337096028248,30.45253373981,-17.2413581349254));
#32731=CARTESIAN_POINT('Ctrl Pts',(23.1707519864209,30.3080867629256,-17.4975676797996));
#32732=CARTESIAN_POINT('Ctrl Pts',(23.7186485394885,30.170626807131,-17.7328951431605));
#32733=CARTESIAN_POINT('Ctrl Pts',(24.2804077704385,30.0435395405948,-17.946249160495));
#32734=CARTESIAN_POINT('Ctrl Pts',(24.7075732751058,29.9548357769835,-18.0938968083019));
#32735=CARTESIAN_POINT('Ctrl Pts',(25.0692008252975,29.8872739715487,-18.2061112471098));
#32736=CARTESIAN_POINT('Ctrl Pts',(25.3613771492325,29.8377189043884,-18.28880476277));
#32737=CARTESIAN_POINT('Ctrl Pts',(25.5084154817281,29.8145466170753,-18.3277015544066));
#32738=CARTESIAN_POINT('Ctrl Pts',(26.1512870025444,29.7173716879777,-18.4915385207408));
#32739=CARTESIAN_POINT('Ctrl Pts',(27.3223884400173,29.6052740416531,-18.6726738474942));
#32740=CARTESIAN_POINT('Ctrl Pts',(28.3731396048321,29.559177524821,-18.7409825767551));
#32741=CARTESIAN_POINT('Ctrl Pts',(28.9547046473315,29.5324480977279,-18.7836137746098));
#32742=CARTESIAN_POINT('Ctrl Pts',(29.1479037067738,29.5247529606444,-18.7960320303041));
#32743=CARTESIAN_POINT('Ctrl Pts',(29.5140802367921,29.51400582112,-18.8132921881813));
#32744=CARTESIAN_POINT('Ctrl Pts',(29.9718311305158,29.5067996680497,-18.8248686377542));
#32745=CARTESIAN_POINT('Ctrl Pts',(30.5051365276119,29.5060845192011,-18.8260067178222));
#32746=CARTESIAN_POINT('Ctrl Pts',(31.551298475448,29.5150383037988,-18.8116639693829));
#32747=CARTESIAN_POINT('Ctrl Pts',(32.3749555043413,29.5335081969199,-18.7822473977007));
#32748=CARTESIAN_POINT('Ctrl Pts',(33.1551698865007,29.5333957726549,-18.7824304492383));
#32749=CARTESIAN_POINT('Ctrl Pts',(33.4909201969602,29.5333841560219,-18.782448957068));
#32750=CARTESIAN_POINT('Ctrl Pts',(33.981699427726,29.5333602907362,-18.7824875453788));
#32751=CARTESIAN_POINT('Ctrl Pts',(34.4771077390558,29.533343676228,-18.7825142819534));
#32752=CARTESIAN_POINT('Ctrl Pts',(35.1351798881798,29.5333214285967,-18.7825501686284));
#32753=CARTESIAN_POINT('Ctrl Pts',(35.958882261465,29.5332901329543,-18.7826006107083));
#32754=CARTESIAN_POINT('Ctrl Pts',(37.9341479260215,29.5332581373787,-18.7826521993715));
#32755=CARTESIAN_POINT('Ctrl Pts',(39.5833333333333,29.5330603026358,-18.7829711232891));
#32756=CARTESIAN_POINT('Ctrl Pts',(40.9,29.5330603026358,-18.7829711232891));
#32757=CARTESIAN_POINT('',(40.9,27.7992994660114,-17.7819838375536));
#32758=CARTESIAN_POINT('Ctrl Pts',(40.9,27.7992994660114,-17.7819838375536));
#32759=CARTESIAN_POINT('Ctrl Pts',(40.9,28.2327406817405,-18.0322312401327));
#32760=CARTESIAN_POINT('Ctrl Pts',(40.9,28.6661818974695,-18.2824786427117));
#32761=CARTESIAN_POINT('Ctrl Pts',(40.9,29.0996231131986,-18.5327260452908));
#32762=CARTESIAN_POINT('',(38.,27.7992994660114,-17.7819838375536));
#32763=CARTESIAN_POINT('Ctrl Pts',(38.,27.7992994660114,-17.7819838375536));
#32764=CARTESIAN_POINT('Ctrl Pts',(38.9666666666667,27.7992994660114,-17.7819838375536));
#32765=CARTESIAN_POINT('Ctrl Pts',(39.9333333333333,27.7992994660114,-17.7819838375536));
#32766=CARTESIAN_POINT('Ctrl Pts',(40.9,27.7992994660114,-17.7819838375536));
#32767=CARTESIAN_POINT('Ctrl Pts',(37.4972396727241,27.2792903521173,-17.4814222894395));
#32768=CARTESIAN_POINT('Ctrl Pts',(37.6643013627084,27.4529632561668,-17.5817051235871));
#32769=CARTESIAN_POINT('Ctrl Pts',(37.8311425499706,27.6263785906016,-17.6818420596932));
#32770=CARTESIAN_POINT('Ctrl Pts',(37.9976538234737,27.7994318724651,-17.7817719425585));
#32771=CARTESIAN_POINT('',(6.9,29.9143312995417,2.26556458774883));
#32772=CARTESIAN_POINT('Ctrl Pts',(6.9,29.9143312995417,2.26556458774883));
#32773=CARTESIAN_POINT('Ctrl Pts',(6.9,27.3056186709172,2.00382962437802));
#32774=CARTESIAN_POINT('Ctrl Pts',(6.90000000000115,24.6693701926632,1.73285728374608));
#32775=CARTESIAN_POINT('Ctrl Pts',(6.90000000000115,18.7182130985667,1.09593289590079));
#32776=CARTESIAN_POINT('Ctrl Pts',(6.9,14.7845781982083,0.654794893503689));
#32777=CARTESIAN_POINT('Ctrl Pts',(6.9,11.02768739857,0.168526548660245));
#32778=CARTESIAN_POINT('',(22.9245129145126,27.5141512254856,-15.8853026165582));
#32779=CARTESIAN_POINT('Ctrl Pts',(22.9245129145126,27.5141512254856,-15.8853026165582));
#32780=CARTESIAN_POINT('Ctrl Pts',(22.7202811020963,27.5032269692373,-15.7659233420327));
#32781=CARTESIAN_POINT('Ctrl Pts',(22.5089075447093,27.4959054260063,-15.6398559109135));
#32782=CARTESIAN_POINT('Ctrl Pts',(22.2913349439917,27.4928730439354,-15.5073965833875));
#32783=CARTESIAN_POINT('Ctrl Pts',(21.4451770585291,27.4810798586143,-14.9922512750188));
#32784=CARTESIAN_POINT('Ctrl Pts',(20.5220951556665,27.5650257717264,-14.3509960808544));
#32785=CARTESIAN_POINT('Ctrl Pts',(19.7671428819535,27.6762399607749,-13.7859304181011));
#32786=CARTESIAN_POINT('Ctrl Pts',(19.5194773058389,27.7127242885422,-13.600558020691));
#32787=CARTESIAN_POINT('Ctrl Pts',(19.286571638609,27.7514615171004,-13.421872324025));
#32788=CARTESIAN_POINT('Ctrl Pts',(19.0728538401323,27.7894004949774,-13.2552441975238));
#32789=CARTESIAN_POINT('Ctrl Pts',(18.7028555998036,27.8550822264681,-12.966769797946));
#32790=CARTESIAN_POINT('Ctrl Pts',(18.4144703596237,27.9152561335183,-12.7292901983116));
#32791=CARTESIAN_POINT('Ctrl Pts',(18.064287487154,27.994606215575,-12.4284122845048));
#32792=CARTESIAN_POINT('Ctrl Pts',(17.4420927116723,28.1355931408966,-11.8938211301514));
#32793=CARTESIAN_POINT('Ctrl Pts',(16.7224564418219,28.3254287038798,-11.2282910364348));
#32794=CARTESIAN_POINT('Ctrl Pts',(15.9202806616111,28.5439924969395,-10.4246142212493));
#32795=CARTESIAN_POINT('Ctrl Pts',(15.4090529834518,28.6832834892781,-9.91242993152956));
#32796=CARTESIAN_POINT('Ctrl Pts',(14.8739602945714,28.8377564730262,-9.33532862360329));
#32797=CARTESIAN_POINT('Ctrl Pts',(14.3169794331154,28.9944199787763,-8.69171842999367));
#32798=CARTESIAN_POINT('Ctrl Pts',(13.8864206762836,29.1155243989539,-8.19419324731421));
#32799=CARTESIAN_POINT('Ctrl Pts',(13.3867890027804,29.2546860278643,-7.5917385218513));
#32800=CARTESIAN_POINT('Ctrl Pts',(12.8146824059514,29.3960736315876,-6.86770373383358));
#32801=CARTESIAN_POINT('Ctrl Pts',(12.2526665517595,29.5349674589251,-6.15643937836581));
#32802=CARTESIAN_POINT('Ctrl Pts',(11.6379478462803,29.678401911158,-5.32066918438564));
#32803=CARTESIAN_POINT('Ctrl Pts',(10.9739250490308,29.7956367796097,-4.35448584004002));
#32804=CARTESIAN_POINT('Ctrl Pts',(10.5683455447963,29.8672428449776,-3.76434923114274));
#32805=CARTESIAN_POINT('Ctrl Pts',(10.1437415406956,29.9275397584159,-3.12422765605936));
#32806=CARTESIAN_POINT('Ctrl Pts',(9.74137929176525,29.9670595377668,-2.50486371218385));
#32807=CARTESIAN_POINT('Ctrl Pts',(8.72285779294234,30.0670981099855,-0.93703399130421));
#32808=CARTESIAN_POINT('Ctrl Pts',(7.81323138778195,30.0560666286387,0.638451825302682));
#32809=CARTESIAN_POINT('Ctrl Pts',(6.9,29.9143312995417,2.26556458774884));
#32810=CARTESIAN_POINT('Ctrl Pts',(30.5,29.5059919176187,-18.8254200738635));
#32811=CARTESIAN_POINT('Ctrl Pts',(29.9560179420816,29.293615660989,-18.7064245513841));
#32812=CARTESIAN_POINT('Ctrl Pts',(29.4152668325132,29.0895919906434,-18.5734800115823));
#32813=CARTESIAN_POINT('Ctrl Pts',(28.8740459957565,28.9020067835811,-18.4125151878636));
#32814=CARTESIAN_POINT('Ctrl Pts',(28.353527792344,28.7215970352204,-18.2577075471291));
#32815=CARTESIAN_POINT('Ctrl Pts',(27.8179515912466,28.533139934629,-18.1008601332298));
#32816=CARTESIAN_POINT('Ctrl Pts',(27.2695051149491,28.3565719042575,-17.9186544331585));
#32817=CARTESIAN_POINT('Ctrl Pts',(26.9554553615883,28.2554660556724,-17.8143203592948));
#32818=CARTESIAN_POINT('Ctrl Pts',(26.6378099296971,28.1585101274348,-17.7019284120276));
#32819=CARTESIAN_POINT('Ctrl Pts',(26.3179304017917,28.0701057587103,-17.5778023417279));
#32820=CARTESIAN_POINT('Ctrl Pts',(26.1078196745982,28.012037940737,-17.4962709631331));
#32821=CARTESIAN_POINT('Ctrl Pts',(25.8967402232745,27.9576659729224,-17.409683568055));
#32822=CARTESIAN_POINT('Ctrl Pts',(25.6850706236774,27.9082593406129,-17.3169960819306));
#32823=CARTESIAN_POINT('Ctrl Pts',(25.6562210027417,27.9015254373195,-17.3043631915899));
#32824=CARTESIAN_POINT('Ctrl Pts',(25.6277737638215,27.8949772388532,-17.2918013331136));
#32825=CARTESIAN_POINT('Ctrl Pts',(25.5983858063598,27.8883138877393,-17.2787081509674));
#32826=CARTESIAN_POINT('Ctrl Pts',(25.1249357452756,27.7809650188704,-17.067772501732));
#32827=CARTESIAN_POINT('Ctrl Pts',(24.1510084067019,27.5797558484168,-16.6022239440147));
#32828=CARTESIAN_POINT('Ctrl Pts',(22.9245129145126,27.5141512254856,-15.8853026165582));
#32829=CARTESIAN_POINT('Origin',(49.9,0.,0.));
#32830=CARTESIAN_POINT('',(50.15,-9.2,1.12667505521557E-15));
#32831=CARTESIAN_POINT('Origin',(50.15,0.,0.));
#32832=CARTESIAN_POINT('',(49.65,-8.7,-1.0654427152582E-15));
#32833=CARTESIAN_POINT('',(49.9,-8.95,-1.09605888523688E-15));
#32834=CARTESIAN_POINT('Origin',(49.65,0.,0.));
#32835=CARTESIAN_POINT('Origin',(49.65,7.7,0.));
#32836=CARTESIAN_POINT('',(49.65,-7.7,-9.42978035343462E-16));
#32837=CARTESIAN_POINT('Origin',(49.65,0.,0.));
#32838=CARTESIAN_POINT('Origin',(49.75,0.,0.));
#32839=CARTESIAN_POINT('',(51.6,-9.2,1.12667505521557E-15));
#32840=CARTESIAN_POINT('Origin',(51.6,0.,0.));
#32841=CARTESIAN_POINT('',(49.75,-9.2,-1.12667505521557E-15));
#32842=CARTESIAN_POINT('Origin',(47.75,0.,0.));
#32843=CARTESIAN_POINT('',(47.5,-9.2,-1.12667505521557E-15));
#32844=CARTESIAN_POINT('Origin',(47.5,0.,0.));
#32845=CARTESIAN_POINT('',(48.,-8.7,1.0654427152582E-15));
#32846=CARTESIAN_POINT('',(47.75,-8.95,1.09605888523688E-15));
#32847=CARTESIAN_POINT('Origin',(48.,0.,0.));
#32848=CARTESIAN_POINT('Origin',(48.,9.7,0.));
#32849=CARTESIAN_POINT('',(48.,-7.7,-9.42978035343462E-16));
#32850=CARTESIAN_POINT('Origin',(48.,0.,0.));
#32851=CARTESIAN_POINT('Origin',(49.75,0.,0.));
#32852=CARTESIAN_POINT('',(44.4,-9.2,-1.12667505521557E-15));
#32853=CARTESIAN_POINT('',(49.75,-9.2,-1.12667505521557E-15));
#32854=CARTESIAN_POINT('Origin',(44.4,0.,0.));
#32855=CARTESIAN_POINT('Origin',(39.5,29.8970448036199,13.5172791635421));
#32856=CARTESIAN_POINT('',(37.6890795305109,29.8980142324913,13.062275865462));
#32857=CARTESIAN_POINT('',(38.,29.8960753747485,13.9722824616222));
#32858=CARTESIAN_POINT('Ctrl Pts',(37.6890795305109,29.8980142324913,13.062275865462));
#32859=CARTESIAN_POINT('Ctrl Pts',(37.8392820392456,29.8970503150544,13.5146923611995));
#32860=CARTESIAN_POINT('Ctrl Pts',(38.,29.8960753747485,13.9722824616222));
#32861=CARTESIAN_POINT('',(41.,29.8960753747485,13.9722824616222));
#32862=CARTESIAN_POINT('',(39.5,29.8960753747485,13.9722824616222));
#32863=CARTESIAN_POINT('',(41.1878146323178,29.897037739141,13.520600663113));
#32864=CARTESIAN_POINT('Ctrl Pts',(41.,29.8960753747485,13.9722824616222));
#32865=CARTESIAN_POINT('Ctrl Pts',(41.0954573034532,29.8965579362819,13.7457970542549));
#32866=CARTESIAN_POINT('Ctrl Pts',(41.1878146323178,29.897037739141,13.520600663113));
#32867=CARTESIAN_POINT('',(41.,29.8980142324913,13.062275865462));
#32868=CARTESIAN_POINT('Ctrl Pts',(41.1878146323178,29.897037739141,13.520600663113));
#32869=CARTESIAN_POINT('Ctrl Pts',(41.0874190143433,29.8975316564897,13.2887794747321));
#32870=CARTESIAN_POINT('Ctrl Pts',(41.,29.8980142324913,13.062275865462));
#32871=CARTESIAN_POINT('',(39.5,29.8980142324913,13.062275865462));
#32872=CARTESIAN_POINT('Origin',(41.25,37.284736894758,9.9904151409573));
#32873=CARTESIAN_POINT('',(41.5,29.553277056526,13.5223450340618));
#32874=CARTESIAN_POINT('Ctrl Pts',(41.1878146323178,29.8970377514405,13.5206006631392));
#32875=CARTESIAN_POINT('Ctrl Pts',(41.2916267029318,29.7825583314293,13.5218058342594));
#32876=CARTESIAN_POINT('Ctrl Pts',(41.3956918967678,29.6679697026706,13.5223797770881));
#32877=CARTESIAN_POINT('Ctrl Pts',(41.5,29.553277056526,13.5223450340618));
#32878=CARTESIAN_POINT('',(41.5,32.3550612130622,3.06594421002715));
#32879=CARTESIAN_POINT('Origin',(41.5,37.284736894758,9.9904151409573));
#32880=CARTESIAN_POINT('',(41.1878146546253,32.6518945010449,3.23933521449283));
#32881=CARTESIAN_POINT('Ctrl Pts',(41.5,32.3550612130622,3.06594421002716));
#32882=CARTESIAN_POINT('Ctrl Pts',(41.39570853676,32.4543894816631,3.12325130125064));
#32883=CARTESIAN_POINT('Ctrl Pts',(41.2916432763383,32.5533392901647,3.18104250345541));
#32884=CARTESIAN_POINT('Ctrl Pts',(41.1878146546253,32.6518945010449,3.23933521449283));
#32885=CARTESIAN_POINT('',(41.,32.4235777807772,3.63674438551515));
#32886=CARTESIAN_POINT('Ctrl Pts',(41.1878146546253,32.6518945010449,3.23933521449283));
#32887=CARTESIAN_POINT('Ctrl Pts',(41.0874190341598,32.5364116500246,3.44034521515088));
#32888=CARTESIAN_POINT('Ctrl Pts',(41.,32.4235777807772,3.63674438551515));
#32889=CARTESIAN_POINT('Origin',(41.,37.284736894758,9.9904151409573));
#32890=CARTESIAN_POINT('Origin',(41.25,0.,0.));
#32891=CARTESIAN_POINT('',(41.,27.0483892479909,18.9046195171755));
#32892=CARTESIAN_POINT('Origin',(41.,0.,0.));
#32893=CARTESIAN_POINT('',(41.1878146339918,26.6577025178081,19.1312938476316));
#32894=CARTESIAN_POINT('Ctrl Pts',(41.1878146339918,26.6577025178081,19.1312938476316));
#32895=CARTESIAN_POINT('Ctrl Pts',(41.0954573053938,26.8524884122049,19.0182801301661));
#32896=CARTESIAN_POINT('Ctrl Pts',(41.,27.0483892479909,18.9046195171755));
#32897=CARTESIAN_POINT('',(41.5,26.4873328464988,18.8327161790004));
#32898=CARTESIAN_POINT('Ctrl Pts',(41.5,26.4873328464988,18.8327161790004));
#32899=CARTESIAN_POINT('Ctrl Pts',(41.3957085361513,26.5447001051442,18.9320097106969));
#32900=CARTESIAN_POINT('Ctrl Pts',(41.2916417549508,26.6014983751947,19.0315347253102));
#32901=CARTESIAN_POINT('Ctrl Pts',(41.1878146339918,26.6577025235174,19.1312938574719));
#32902=CARTESIAN_POINT('Origin',(41.5,0.,0.));
#32903=CARTESIAN_POINT('Origin',(39.5,0.,0.));
#32904=CARTESIAN_POINT('Origin',(38.,0.,0.));
#32905=CARTESIAN_POINT('',(40.9,27.7992994660114,17.7819838375536));
#32906=CARTESIAN_POINT('Origin',(40.9,0.,0.));
#32907=CARTESIAN_POINT('',(38.,27.7992994660114,17.7819838375536));
#32908=CARTESIAN_POINT('Ctrl Pts',(40.9,27.7992994660114,17.7819838375536));
#32909=CARTESIAN_POINT('Ctrl Pts',(39.9333333333333,27.7992994660114,17.7819838375536));
#32910=CARTESIAN_POINT('Ctrl Pts',(38.9666666666667,27.7992994660114,17.7819838375536));
#32911=CARTESIAN_POINT('Ctrl Pts',(38.,27.7992994660114,17.7819838375536));
#32912=CARTESIAN_POINT('',(38.,27.0483892479909,18.9046195171755));
#32913=CARTESIAN_POINT('Origin',(38.,0.,0.));
#32914=CARTESIAN_POINT('',(39.5,27.0483892479909,18.9046195171755));
#32915=CARTESIAN_POINT('Origin',(39.5,26.6548295474835,19.1329607162453));
#32916=CARTESIAN_POINT('',(37.6890795305109,26.2612698469761,19.3613019153151));
#32917=CARTESIAN_POINT('Ctrl Pts',(38.,27.0483892479909,18.9046195171755));
#32918=CARTESIAN_POINT('Ctrl Pts',(37.8392820392454,26.6525920666572,19.1342588904591));
#32919=CARTESIAN_POINT('Ctrl Pts',(37.6890795305109,26.2612698469761,19.3613019153151));
#32920=CARTESIAN_POINT('',(41.,26.2612698469761,19.3613019153151));
#32921=CARTESIAN_POINT('',(39.5,26.2612698469761,19.3613019153151));
#32922=CARTESIAN_POINT('Ctrl Pts',(41.,26.2612698469761,19.3613019153151));
#32923=CARTESIAN_POINT('Ctrl Pts',(41.0874190154267,26.4571864382329,19.2476321871109));
#32924=CARTESIAN_POINT('Ctrl Pts',(41.1878146339918,26.6577025178081,19.1312938476316));
#32925=CARTESIAN_POINT('Origin',(41.25,27.2943217538007,27.2943217538007));
#32926=CARTESIAN_POINT('',(41.,19.3613019153151,26.2612698469761));
#32927=CARTESIAN_POINT('Origin',(41.,27.2943217538007,27.2943217538007));
#32928=CARTESIAN_POINT('',(41.1878146323178,19.1312938484417,26.6577025182511));
#32929=CARTESIAN_POINT('Ctrl Pts',(41.1878146323178,19.1312938484417,26.6577025182511));
#32930=CARTESIAN_POINT('Ctrl Pts',(41.0874190143433,19.2476321876035,26.457186438652));
#32931=CARTESIAN_POINT('Ctrl Pts',(41.,19.3613019153151,26.2612698469761));
#32932=CARTESIAN_POINT('',(41.5,18.8327161790004,26.4873328464988));
#32933=CARTESIAN_POINT('Ctrl Pts',(41.1878146323178,19.1312938590803,26.6577025244235));
#32934=CARTESIAN_POINT('Ctrl Pts',(41.2916267029318,19.0315491875799,26.601506523224));
#32935=CARTESIAN_POINT('Ctrl Pts',(41.3956918967678,18.9320255526757,26.5447092579146));
#32936=CARTESIAN_POINT('Ctrl Pts',(41.5,18.8327161790004,26.4873328464988));
#32937=CARTESIAN_POINT('Origin',(41.5,27.2943217538007,27.2943217538007));
#32938=CARTESIAN_POINT('Origin',(39.5,19.1329607162453,26.6548295474835));
#32939=CARTESIAN_POINT('',(37.6890795305109,19.3613019153151,26.2612698469761));
#32940=CARTESIAN_POINT('',(38.,18.9046195171755,27.0483892479908));
#32941=CARTESIAN_POINT('Ctrl Pts',(37.6890795305109,19.3613019153151,26.2612698469761));
#32942=CARTESIAN_POINT('Ctrl Pts',(37.8392820392454,19.1342588904592,26.652592066657));
#32943=CARTESIAN_POINT('Ctrl Pts',(38.,18.9046195171755,27.0483892479908));
#32944=CARTESIAN_POINT('',(41.,18.9046195171755,27.0483892479908));
#32945=CARTESIAN_POINT('',(39.5,18.9046195171755,27.0483892479908));
#32946=CARTESIAN_POINT('Ctrl Pts',(41.,18.9046195171755,27.0483892479908));
#32947=CARTESIAN_POINT('Ctrl Pts',(41.0954573034533,19.0182801314061,26.8524884123908));
#32948=CARTESIAN_POINT('Ctrl Pts',(41.1878146323178,19.1312938484417,26.6577025182511));
#32949=CARTESIAN_POINT('',(39.5,19.3613019153151,26.2612698469761));
#32950=CARTESIAN_POINT('Origin',(41.25,0.,0.));
#32951=CARTESIAN_POINT('',(41.,13.9722824616222,29.8960753747485));
#32952=CARTESIAN_POINT('Origin',(41.,0.,0.));
#32953=CARTESIAN_POINT('',(41.1878146339917,13.5206006631344,29.8970377382179));
#32954=CARTESIAN_POINT('Ctrl Pts',(41.1878146339917,13.5206006631344,29.8970377382179));
#32955=CARTESIAN_POINT('Ctrl Pts',(41.0954573053939,13.7457970547134,29.8965579351151));
#32956=CARTESIAN_POINT('Ctrl Pts',(41.,13.9722824616222,29.8960753747485));
#32957=CARTESIAN_POINT('',(41.5,13.5223450340618,29.553277056526));
#32958=CARTESIAN_POINT('Ctrl Pts',(41.5,13.5223450340618,29.553277056526));
#32959=CARTESIAN_POINT('Ctrl Pts',(41.3957085361513,13.5223797715459,29.6679514067293));
#32960=CARTESIAN_POINT('Ctrl Pts',(41.2916417549508,13.521806008994,29.7825417327217));
#32961=CARTESIAN_POINT('Ctrl Pts',(41.1878146339918,13.5206006631586,29.8970377495945));
#32962=CARTESIAN_POINT('Origin',(41.5,0.,0.));
#32963=CARTESIAN_POINT('Origin',(39.5,0.,0.));
#32964=CARTESIAN_POINT('Origin',(38.,0.,0.));
#32965=CARTESIAN_POINT('',(40.9,15.1839076262003,29.2992994660114));
#32966=CARTESIAN_POINT('Origin',(40.9,0.,0.));
#32967=CARTESIAN_POINT('',(38.,15.1839076262003,29.2992994660114));
#32968=CARTESIAN_POINT('Ctrl Pts',(40.9,15.1839076262003,29.2992994660114));
#32969=CARTESIAN_POINT('Ctrl Pts',(39.9333333333333,15.1839076262003,29.2992994660114));
#32970=CARTESIAN_POINT('Ctrl Pts',(38.9666666666667,15.1839076262003,29.2992994660114));
#32971=CARTESIAN_POINT('Ctrl Pts',(38.,15.1839076262003,29.2992994660114));
#32972=CARTESIAN_POINT('',(38.,13.9722824616222,29.8960753747485));
#32973=CARTESIAN_POINT('Origin',(38.,0.,0.));
#32974=CARTESIAN_POINT('',(39.5,13.9722824616222,29.8960753747485));
#32975=CARTESIAN_POINT('Origin',(39.5,13.5172791635421,29.8970448036199));
#32976=CARTESIAN_POINT('',(37.6890795305109,13.062275865462,29.8980142324913));
#32977=CARTESIAN_POINT('Ctrl Pts',(38.,13.9722824616222,29.8960753747485));
#32978=CARTESIAN_POINT('Ctrl Pts',(37.8392820392454,13.5146923611992,29.8970503150544));
#32979=CARTESIAN_POINT('Ctrl Pts',(37.6890795305109,13.062275865462,29.8980142324913));
#32980=CARTESIAN_POINT('',(41.,13.062275865462,29.8980142324913));
#32981=CARTESIAN_POINT('',(39.5,13.062275865462,29.8980142324913));
#32982=CARTESIAN_POINT('Ctrl Pts',(41.,13.062275865462,29.8980142324913));
#32983=CARTESIAN_POINT('Ctrl Pts',(41.0874190154267,13.2887794746153,29.8975316558535));
#32984=CARTESIAN_POINT('Ctrl Pts',(41.1878146339917,13.5206006631344,29.8970377382179));
#32985=CARTESIAN_POINT('Origin',(41.25,9.99041514095731,37.284736894758));
#32986=CARTESIAN_POINT('',(41.,3.63674438551516,32.4235777807772));
#32987=CARTESIAN_POINT('Origin',(41.,9.99041514095731,37.284736894758));
#32988=CARTESIAN_POINT('',(41.1878146323178,3.23933522088993,32.6518945115547));
#32989=CARTESIAN_POINT('Ctrl Pts',(41.1878146323178,3.23933522088992,32.6518945115547));
#32990=CARTESIAN_POINT('Ctrl Pts',(41.0874190143434,3.44034521783764,32.5364116623356));
#32991=CARTESIAN_POINT('Ctrl Pts',(41.,3.63674438551516,32.4235777807772));
#32992=CARTESIAN_POINT('',(41.5,3.06594421002715,32.3550612130622));
#32993=CARTESIAN_POINT('Ctrl Pts',(41.1878146323177,3.23933522701702,32.6518945222195));
#32994=CARTESIAN_POINT('Ctrl Pts',(41.2916267029318,3.18105180820533,32.5533550218394));
#32995=CARTESIAN_POINT('Ctrl Pts',(41.3956918967678,3.12326044475599,32.4544053297638));
#32996=CARTESIAN_POINT('Ctrl Pts',(41.5,3.06594421002716,32.3550612130622));
#32997=CARTESIAN_POINT('Origin',(41.5,9.99041514095731,37.284736894758));
#32998=CARTESIAN_POINT('Origin',(39.5,3.24221525613641,32.6502398797874));
#32999=CARTESIAN_POINT('',(37.6890795305109,3.63674438551516,32.4235777807772));
#33000=CARTESIAN_POINT('',(38.,2.84768612675767,32.8769019787977));
#33001=CARTESIAN_POINT('Ctrl Pts',(37.6890795305109,3.63674438551516,32.4235777807772));
#33002=CARTESIAN_POINT('Ctrl Pts',(37.8392820392455,3.24445824839702,32.6489512516584));
#33003=CARTESIAN_POINT('Ctrl Pts',(38.,2.84768612675767,32.8769019787977));
#33004=CARTESIAN_POINT('',(41.,2.84768612675767,32.8769019787977));
#33005=CARTESIAN_POINT('',(39.5,2.84768612675767,32.8769019787977));
#33006=CARTESIAN_POINT('Ctrl Pts',(41.,2.84768612675767,32.8769019787977));
#33007=CARTESIAN_POINT('Ctrl Pts',(41.0954573034532,3.04406952389089,32.7640771856609));
#33008=CARTESIAN_POINT('Ctrl Pts',(41.1878146323178,3.23933522088993,32.6518945115547));
#33009=CARTESIAN_POINT('',(39.5,3.63674438551516,32.4235777807772));
#33010=CARTESIAN_POINT('Origin',(41.25,0.,0.));
#33011=CARTESIAN_POINT('',(41.,-2.84768612675766,32.8769019787977));
#33012=CARTESIAN_POINT('Origin',(41.,0.,0.));
#33013=CARTESIAN_POINT('',(41.1878146339918,-3.23933522040986,32.651894510766));
#33014=CARTESIAN_POINT('Ctrl Pts',(41.1878146339918,-3.23933522040986,32.651894510766));
#33015=CARTESIAN_POINT('Ctrl Pts',(41.095457305394,-3.04406952291064,32.7640771848795));
#33016=CARTESIAN_POINT('Ctrl Pts',(41.,-2.84768612675766,32.8769019787977));
#33017=CARTESIAN_POINT('',(41.5,-3.06594421002714,32.3550612130622));
#33018=CARTESIAN_POINT('Ctrl Pts',(41.5,-3.06594421002715,32.3550612130622));
#33019=CARTESIAN_POINT('Ctrl Pts',(41.3957085361513,-3.1232513015851,32.4543894822428));
#33020=CARTESIAN_POINT('Ctrl Pts',(41.2916417549508,-3.181043357527,32.5533407343041));
#33021=CARTESIAN_POINT('Ctrl Pts',(41.1878146339918,-3.23933522607716,32.6518945206305));
#33022=CARTESIAN_POINT('Origin',(41.5,0.,0.));
#33023=CARTESIAN_POINT('Origin',(39.5,0.,0.));
#33024=CARTESIAN_POINT('Origin',(38.,0.,0.));
#33025=CARTESIAN_POINT('',(40.9,-1.5,32.9658914637539));
#33026=CARTESIAN_POINT('Origin',(40.9,0.,0.));
#33027=CARTESIAN_POINT('',(38.,-1.5,32.9658914637539));
#33028=CARTESIAN_POINT('Ctrl Pts',(40.9,-1.5,32.9658914637539));
#33029=CARTESIAN_POINT('Ctrl Pts',(39.9333333333333,-1.5,32.9658914637539));
#33030=CARTESIAN_POINT('Ctrl Pts',(38.9666666666667,-1.5,32.9658914637539));
#33031=CARTESIAN_POINT('Ctrl Pts',(38.,-1.5,32.9658914637539));
#33032=CARTESIAN_POINT('',(38.,-2.84768612675766,32.8769019787977));
#33033=CARTESIAN_POINT('Origin',(38.,0.,0.));
#33034=CARTESIAN_POINT('',(39.5,-2.84768612675766,32.8769019787977));
#33035=CARTESIAN_POINT('Origin',(39.5,-3.2422152561364,32.6502398797874));
#33036=CARTESIAN_POINT('',(37.6890795305109,-3.63674438551515,32.4235777807772));
#33037=CARTESIAN_POINT('Ctrl Pts',(38.,-2.84768612675766,32.8769019787977));
#33038=CARTESIAN_POINT('Ctrl Pts',(37.8392820392455,-3.244458248397,32.6489512516584));
#33039=CARTESIAN_POINT('Ctrl Pts',(37.6890795305109,-3.63674438551515,32.4235777807772));
#33040=CARTESIAN_POINT('',(41.,-3.63674438551515,32.4235777807772));
#33041=CARTESIAN_POINT('',(39.5,-3.63674438551515,32.4235777807772));
#33042=CARTESIAN_POINT('Ctrl Pts',(41.,-3.63674438551515,32.4235777807772));
#33043=CARTESIAN_POINT('Ctrl Pts',(41.0874190154267,-3.44034521762067,32.5364116617262));
#33044=CARTESIAN_POINT('Ctrl Pts',(41.1878146339918,-3.23933522040986,32.651894510766));
#33045=CARTESIAN_POINT('Origin',(41.25,-9.9904151409573,37.284736894758));
#33046=CARTESIAN_POINT('',(41.,-13.062275865462,29.8980142324913));
#33047=CARTESIAN_POINT('Origin',(41.,-9.9904151409573,37.284736894758));
#33048=CARTESIAN_POINT('',(41.1878146323178,-13.520600663113,29.897037739141));
#33049=CARTESIAN_POINT('Ctrl Pts',(41.1878146323178,-13.520600663113,29.897037739141));
#33050=CARTESIAN_POINT('Ctrl Pts',(41.0874190143433,-13.2887794747321,29.8975316564897));
#33051=CARTESIAN_POINT('Ctrl Pts',(41.,-13.062275865462,29.8980142324913));
#33052=CARTESIAN_POINT('',(41.5,-13.5223450340618,29.553277056526));
#33053=CARTESIAN_POINT('Ctrl Pts',(41.1878146323178,-13.5206006631392,29.8970377514405));
#33054=CARTESIAN_POINT('Ctrl Pts',(41.2916267029318,-13.5218058342594,29.7825583314293));
#33055=CARTESIAN_POINT('Ctrl Pts',(41.3956918967678,-13.5223797770881,29.6679697026706));
#33056=CARTESIAN_POINT('Ctrl Pts',(41.5,-13.5223450340618,29.553277056526));
#33057=CARTESIAN_POINT('Origin',(41.5,-9.9904151409573,37.284736894758));
#33058=CARTESIAN_POINT('Origin',(39.5,-13.5172791635421,29.8970448036199));
#33059=CARTESIAN_POINT('',(37.6890795305109,-13.062275865462,29.8980142324913));
#33060=CARTESIAN_POINT('',(38.,-13.9722824616222,29.8960753747485));
#33061=CARTESIAN_POINT('Ctrl Pts',(37.6890795305109,-13.062275865462,29.8980142324913));
#33062=CARTESIAN_POINT('Ctrl Pts',(37.8392820392455,-13.5146923611994,29.8970503150544));
#33063=CARTESIAN_POINT('Ctrl Pts',(38.,-13.9722824616222,29.8960753747485));
#33064=CARTESIAN_POINT('',(41.,-13.9722824616222,29.8960753747485));
#33065=CARTESIAN_POINT('',(39.5,-13.9722824616222,29.8960753747485));
#33066=CARTESIAN_POINT('Ctrl Pts',(41.,-13.9722824616222,29.8960753747485));
#33067=CARTESIAN_POINT('Ctrl Pts',(41.0954573034533,-13.7457970542547,29.8965579362819));
#33068=CARTESIAN_POINT('Ctrl Pts',(41.1878146323178,-13.520600663113,29.897037739141));
#33069=CARTESIAN_POINT('',(39.5,-13.062275865462,29.8980142324913));
#33070=CARTESIAN_POINT('Origin',(41.25,0.,0.));
#33071=CARTESIAN_POINT('',(41.,-18.9046195171755,27.0483892479909));
#33072=CARTESIAN_POINT('Origin',(41.,0.,0.));
#33073=CARTESIAN_POINT('',(41.1878146339917,-19.1312938476316,26.6577025178081));
#33074=CARTESIAN_POINT('Ctrl Pts',(41.1878146339917,-19.1312938476316,26.6577025178081));
#33075=CARTESIAN_POINT('Ctrl Pts',(41.0954573053939,-19.0182801301662,26.8524884122047));
#33076=CARTESIAN_POINT('Ctrl Pts',(41.,-18.9046195171755,27.0483892479909));
#33077=CARTESIAN_POINT('',(41.5,-18.8327161790004,26.4873328464988));
#33078=CARTESIAN_POINT('Ctrl Pts',(41.5,-18.8327161790004,26.4873328464988));
#33079=CARTESIAN_POINT('Ctrl Pts',(41.3957085361513,-18.9320097106969,26.5447001051442));
#33080=CARTESIAN_POINT('Ctrl Pts',(41.2916417549508,-19.0315347253102,26.6014983751947));
#33081=CARTESIAN_POINT('Ctrl Pts',(41.1878146339918,-19.1312938574719,26.6577025235174));
#33082=CARTESIAN_POINT('Origin',(41.5,0.,0.));
#33083=CARTESIAN_POINT('Origin',(39.5,0.,0.));
#33084=CARTESIAN_POINT('Origin',(38.,0.,0.));
#33085=CARTESIAN_POINT('',(40.9,-17.7819838375536,27.7992994660114));
#33086=CARTESIAN_POINT('Origin',(40.9,0.,0.));
#33087=CARTESIAN_POINT('',(38.,-17.7819838375536,27.7992994660114));
#33088=CARTESIAN_POINT('Ctrl Pts',(40.9,-17.7819838375536,27.7992994660114));
#33089=CARTESIAN_POINT('Ctrl Pts',(39.9333333333333,-17.7819838375536,27.7992994660114));
#33090=CARTESIAN_POINT('Ctrl Pts',(38.9666666666667,-17.7819838375536,27.7992994660114));
#33091=CARTESIAN_POINT('Ctrl Pts',(38.,-17.7819838375536,27.7992994660114));
#33092=CARTESIAN_POINT('',(38.,-18.9046195171755,27.0483892479909));
#33093=CARTESIAN_POINT('Origin',(38.,0.,0.));
#33094=CARTESIAN_POINT('',(39.5,-18.9046195171755,27.0483892479909));
#33095=CARTESIAN_POINT('Origin',(39.5,-19.1329607162453,26.6548295474835));
#33096=CARTESIAN_POINT('',(37.6890795305109,-19.3613019153151,26.2612698469761));
#33097=CARTESIAN_POINT('Ctrl Pts',(38.,-18.9046195171755,27.0483892479909));
#33098=CARTESIAN_POINT('Ctrl Pts',(37.8392820392454,-19.1342588904591,26.6525920666571));
#33099=CARTESIAN_POINT('Ctrl Pts',(37.6890795305109,-19.3613019153151,26.2612698469761));
#33100=CARTESIAN_POINT('',(41.,-19.3613019153151,26.2612698469761));
#33101=CARTESIAN_POINT('',(39.5,-19.3613019153151,26.2612698469761));
#33102=CARTESIAN_POINT('Ctrl Pts',(41.,-19.3613019153151,26.2612698469761));
#33103=CARTESIAN_POINT('Ctrl Pts',(41.0874190154267,-19.2476321871109,26.4571864382329));
#33104=CARTESIAN_POINT('Ctrl Pts',(41.1878146339917,-19.1312938476316,26.6577025178081));
#33105=CARTESIAN_POINT('Origin',(41.25,-27.2943217538007,27.2943217538008));
#33106=CARTESIAN_POINT('',(41.,-26.2612698469761,19.3613019153151));
#33107=CARTESIAN_POINT('Origin',(41.,-27.2943217538007,27.2943217538008));
#33108=CARTESIAN_POINT('',(41.1878146323178,-26.657702518251,19.1312938484417));
#33109=CARTESIAN_POINT('Ctrl Pts',(41.1878146323178,-26.657702518251,19.1312938484417));
#33110=CARTESIAN_POINT('Ctrl Pts',(41.0874190143433,-26.457186438652,19.2476321876035));
#33111=CARTESIAN_POINT('Ctrl Pts',(41.,-26.2612698469761,19.3613019153152));
#33112=CARTESIAN_POINT('',(41.5,-26.4873328464988,18.8327161790004));
#33113=CARTESIAN_POINT('Ctrl Pts',(41.1878146323178,-26.6577025244235,19.1312938590803));
#33114=CARTESIAN_POINT('Ctrl Pts',(41.2916267029318,-26.6015065232239,19.0315491875799));
#33115=CARTESIAN_POINT('Ctrl Pts',(41.3956918967678,-26.5447092579146,18.9320255526757));
#33116=CARTESIAN_POINT('Ctrl Pts',(41.5,-26.4873328464988,18.8327161790004));
#33117=CARTESIAN_POINT('Origin',(41.5,-27.2943217538007,27.2943217538008));
#33118=CARTESIAN_POINT('Origin',(39.5,-26.6548295474835,19.1329607162453));
#33119=CARTESIAN_POINT('',(37.6890795305109,-26.2612698469761,19.3613019153151));
#33120=CARTESIAN_POINT('',(38.,-27.0483892479908,18.9046195171755));
#33121=CARTESIAN_POINT('Ctrl Pts',(37.6890795305109,-26.2612698469761,19.3613019153151));
#33122=CARTESIAN_POINT('Ctrl Pts',(37.8392820392455,-26.6525920666574,19.134258890459));
#33123=CARTESIAN_POINT('Ctrl Pts',(38.,-27.0483892479908,18.9046195171755));
#33124=CARTESIAN_POINT('',(41.,-27.0483892479908,18.9046195171755));
#33125=CARTESIAN_POINT('',(39.5,-27.0483892479908,18.9046195171755));
#33126=CARTESIAN_POINT('Ctrl Pts',(41.,-27.0483892479908,18.9046195171755));
#33127=CARTESIAN_POINT('Ctrl Pts',(41.0954573034532,-26.8524884123911,19.0182801314059));
#33128=CARTESIAN_POINT('Ctrl Pts',(41.1878146323178,-26.6577025182511,19.1312938484417));
#33129=CARTESIAN_POINT('',(39.5,-26.2612698469761,19.3613019153151));
#33130=CARTESIAN_POINT('Origin',(41.25,0.,0.));
#33131=CARTESIAN_POINT('',(41.,-29.8960753747485,13.9722824616222));
#33132=CARTESIAN_POINT('Origin',(41.,0.,0.));
#33133=CARTESIAN_POINT('',(41.1878146339917,-29.8970377382179,13.5206006631344));
#33134=CARTESIAN_POINT('Ctrl Pts',(41.1878146339917,-29.8970377382179,13.5206006631344));
#33135=CARTESIAN_POINT('Ctrl Pts',(41.0954573053939,-29.8965579351151,13.7457970547134));
#33136=CARTESIAN_POINT('Ctrl Pts',(41.,-29.8960753747485,13.9722824616222));
#33137=CARTESIAN_POINT('',(41.5,-29.553277056526,13.5223450340618));
#33138=CARTESIAN_POINT('Ctrl Pts',(41.5,-29.553277056526,13.5223450340618));
#33139=CARTESIAN_POINT('Ctrl Pts',(41.3957085361513,-29.6679514067293,13.5223797715459));
#33140=CARTESIAN_POINT('Ctrl Pts',(41.2916417549508,-29.7825417327216,13.521806008994));
#33141=CARTESIAN_POINT('Ctrl Pts',(41.1878146339918,-29.8970377495945,13.5206006631586));
#33142=CARTESIAN_POINT('Origin',(41.5,0.,0.));
#33143=CARTESIAN_POINT('Origin',(39.5,0.,0.));
#33144=CARTESIAN_POINT('Origin',(38.,0.,0.));
#33145=CARTESIAN_POINT('',(40.9,-29.2992994660114,15.1839076262003));
#33146=CARTESIAN_POINT('Origin',(40.9,0.,0.));
#33147=CARTESIAN_POINT('',(38.,-29.2992994660114,15.1839076262003));
#33148=CARTESIAN_POINT('Ctrl Pts',(40.9,-29.2992994660114,15.1839076262003));
#33149=CARTESIAN_POINT('Ctrl Pts',(39.9333333333333,-29.2992994660114,15.1839076262003));
#33150=CARTESIAN_POINT('Ctrl Pts',(38.9666666666667,-29.2992994660114,15.1839076262003));
#33151=CARTESIAN_POINT('Ctrl Pts',(38.,-29.2992994660114,15.1839076262003));
#33152=CARTESIAN_POINT('',(38.,-29.8960753747485,13.9722824616222));
#33153=CARTESIAN_POINT('Origin',(38.,0.,0.));
#33154=CARTESIAN_POINT('',(39.5,-29.8960753747485,13.9722824616222));
#33155=CARTESIAN_POINT('Origin',(39.5,-29.8970448036199,13.5172791635421));
#33156=CARTESIAN_POINT('',(37.6890795305109,-29.8980142324913,13.0622758654621));
#33157=CARTESIAN_POINT('Ctrl Pts',(38.,-29.8960753747485,13.9722824616222));
#33158=CARTESIAN_POINT('Ctrl Pts',(37.8392820392455,-29.8970503150544,13.5146923611995));
#33159=CARTESIAN_POINT('Ctrl Pts',(37.6890795305109,-29.8980142324913,13.0622758654621));
#33160=CARTESIAN_POINT('',(41.,-29.8980142324913,13.0622758654621));
#33161=CARTESIAN_POINT('',(39.5,-29.8980142324913,13.0622758654621));
#33162=CARTESIAN_POINT('Ctrl Pts',(41.,-29.8980142324913,13.0622758654621));
#33163=CARTESIAN_POINT('Ctrl Pts',(41.0874190154267,-29.8975316558535,13.2887794746154));
#33164=CARTESIAN_POINT('Ctrl Pts',(41.1878146339917,-29.8970377382179,13.5206006631344));
#33165=CARTESIAN_POINT('Origin',(41.25,-37.284736894758,9.99041514095732));
#33166=CARTESIAN_POINT('',(41.,-32.4235777807772,3.63674438551517));
#33167=CARTESIAN_POINT('Origin',(41.,-37.284736894758,9.99041514095732));
#33168=CARTESIAN_POINT('',(41.1878146546253,-32.6518945010449,3.23933521449285));
#33169=CARTESIAN_POINT('Ctrl Pts',(41.,-32.4235777807772,3.63674438551517));
#33170=CARTESIAN_POINT('Ctrl Pts',(41.0874190341598,-32.5364116500246,3.44034521515094));
#33171=CARTESIAN_POINT('Ctrl Pts',(41.1878146546253,-32.6518945010449,3.23933521449285));
#33172=CARTESIAN_POINT('',(41.5,-32.3550612130622,3.06594421002716));
#33173=CARTESIAN_POINT('Ctrl Pts',(41.1878146546253,-32.6518945010449,3.23933521449284));
#33174=CARTESIAN_POINT('Ctrl Pts',(41.2916290694684,-32.5533527754738,3.18105047964687));
#33175=CARTESIAN_POINT('Ctrl Pts',(41.3956920266496,-32.454405206063,3.12326037338726));
#33176=CARTESIAN_POINT('Ctrl Pts',(41.5,-32.3550612130622,3.06594421002717));
#33177=CARTESIAN_POINT('Origin',(41.5,-37.284736894758,9.99041514095732));
#33178=CARTESIAN_POINT('Origin',(41.5,14.,0.));
#33179=CARTESIAN_POINT('',(41.5,-32.3550612130622,-3.06594421002714));
#33180=CARTESIAN_POINT('Origin',(41.5,0.,0.));
#33181=CARTESIAN_POINT('',(41.5,-29.553277056526,-13.5223450340618));
#33182=CARTESIAN_POINT('Origin',(41.5,-37.284736894758,-9.9904151409573));
#33183=CARTESIAN_POINT('',(41.5,-26.4873328464988,-18.8327161790004));
#33184=CARTESIAN_POINT('Origin',(41.5,0.,0.));
#33185=CARTESIAN_POINT('',(41.5,-18.8327161790004,-26.4873328464988));
#33186=CARTESIAN_POINT('Origin',(41.5,-27.2943217538008,-27.2943217538007));
#33187=CARTESIAN_POINT('',(41.5,-13.5223450340618,-29.553277056526));
#33188=CARTESIAN_POINT('Origin',(41.5,0.,0.));
#33189=CARTESIAN_POINT('',(41.5,-3.06594421002716,-32.3550612130622));
#33190=CARTESIAN_POINT('Origin',(41.5,-9.99041514095732,-37.284736894758));
#33191=CARTESIAN_POINT('',(41.5,3.06594421002714,-32.3550612130622));
#33192=CARTESIAN_POINT('Origin',(41.5,0.,0.));
#33193=CARTESIAN_POINT('',(41.5,13.5223450340618,-29.553277056526));
#33194=CARTESIAN_POINT('Origin',(41.5,9.99041514095729,-37.284736894758));
#33195=CARTESIAN_POINT('',(41.5,18.8327161790004,-26.4873328464989));
#33196=CARTESIAN_POINT('Origin',(41.5,0.,0.));
#33197=CARTESIAN_POINT('',(41.5,26.4873328464988,-18.8327161790004));
#33198=CARTESIAN_POINT('Origin',(41.5,27.2943217538007,-27.2943217538008));
#33199=CARTESIAN_POINT('',(41.5,29.553277056526,-13.5223450340618));
#33200=CARTESIAN_POINT('Origin',(41.5,0.,0.));
#33201=CARTESIAN_POINT('',(41.5,32.3550612130622,-3.06594421002716));
#33202=CARTESIAN_POINT('Origin',(41.5,37.284736894758,-9.99041514095732));
#33203=CARTESIAN_POINT('Origin',(41.5,0.,0.));
#33204=CARTESIAN_POINT('',(41.5,-14.,-1.71450551880629E-15));
#33205=CARTESIAN_POINT('Origin',(41.5,0.,0.));
#33206=CARTESIAN_POINT('Origin',(41.25,0.,0.));
#33207=CARTESIAN_POINT('',(41.,-32.8769019787977,2.84768612675768));
#33208=CARTESIAN_POINT('Ctrl Pts',(41.,-32.8769019787977,2.84768612675768));
#33209=CARTESIAN_POINT('Ctrl Pts',(41.0954573242615,-32.7640771770247,3.04406951423267));
#33210=CARTESIAN_POINT('Ctrl Pts',(41.1878146546253,-32.6518945010449,3.23933521449286));
#33211=CARTESIAN_POINT('',(41.,-32.8769019787977,-2.84768612675766));
#33212=CARTESIAN_POINT('Origin',(41.,0.,0.));
#33213=CARTESIAN_POINT('',(41.1878146339919,-32.6518945107659,-3.23933522040983));
#33214=CARTESIAN_POINT('Ctrl Pts',(41.1878146339919,-32.6518945107659,-3.23933522040983));
#33215=CARTESIAN_POINT('Ctrl Pts',(41.0954573053598,-32.7640771848917,-3.0440695229333));
#33216=CARTESIAN_POINT('Ctrl Pts',(41.,-32.8769019787977,-2.84768612675766));
#33217=CARTESIAN_POINT('Ctrl Pts',(41.5,-32.3550612130622,-3.06594421002715));
#33218=CARTESIAN_POINT('Ctrl Pts',(41.3957085374147,-32.4543894810395,-3.12325130089087));
#33219=CARTESIAN_POINT('Ctrl Pts',(41.2916417560968,-32.5533407332163,-3.18104335688356));
#33220=CARTESIAN_POINT('Ctrl Pts',(41.1878146339919,-32.6518945206304,-3.23933522607709));
#33221=CARTESIAN_POINT('Origin',(39.5,-32.6502398797874,3.24221525613642));
#33222=CARTESIAN_POINT('',(37.6890795305109,-32.4235777807772,3.63674438551517));
#33223=CARTESIAN_POINT('',(39.5,-32.4235777807772,3.63674438551517));
#33224=CARTESIAN_POINT('',(38.,-32.8769019787977,2.84768612675768));
#33225=CARTESIAN_POINT('Ctrl Pts',(37.6890795305109,-32.4235777807772,3.63674438551517));
#33226=CARTESIAN_POINT('Ctrl Pts',(37.8392820392454,-32.6489512516583,3.2444582483972));
#33227=CARTESIAN_POINT('Ctrl Pts',(38.,-32.8769019787977,2.84768612675768));
#33228=CARTESIAN_POINT('',(39.5,-32.8769019787977,2.84768612675768));
#33229=CARTESIAN_POINT('Origin',(36.8,27.2943217538007,27.2943217538007));
#33230=CARTESIAN_POINT('Ctrl Pts',(37.5,25.9430157904516,19.4092743732572));
#33231=CARTESIAN_POINT('Ctrl Pts',(37.5185015343068,25.9748214246282,19.4038236586252));
#33232=CARTESIAN_POINT('Ctrl Pts',(37.537045458494,26.0064935487318,19.3985939360341));
#33233=CARTESIAN_POINT('Ctrl Pts',(37.599346002575,26.1122358651254,19.3817798286965));
#33234=CARTESIAN_POINT('Ctrl Pts',(37.6438438231274,26.18666663184,19.3710168782449));
#33235=CARTESIAN_POINT('Ctrl Pts',(37.6890795305109,26.2612698469761,19.3613019153151));
#33236=CARTESIAN_POINT('Origin',(36.8,27.2943217538007,27.2943217538007));
#33237=CARTESIAN_POINT('Ctrl Pts',(37.6890795305109,19.3613019153151,26.2612698469761));
#33238=CARTESIAN_POINT('Ctrl Pts',(37.6438438231274,19.3710168782449,26.18666663184));
#33239=CARTESIAN_POINT('Ctrl Pts',(37.599346002575,19.3817798286965,26.1122358651254));
#33240=CARTESIAN_POINT('Ctrl Pts',(37.537045458494,19.3985939360341,26.0064935487318));
#33241=CARTESIAN_POINT('Ctrl Pts',(37.5185015343068,19.4038236586252,25.9748214246282));
#33242=CARTESIAN_POINT('Ctrl Pts',(37.5,19.4092743732572,25.9430157904516));
#33243=CARTESIAN_POINT('Origin',(36.8,37.284736894758,9.9904151409573));
#33244=CARTESIAN_POINT('',(37.6890795305109,32.4235777807772,3.63674438551515));
#33245=CARTESIAN_POINT('',(39.5,32.4235777807772,3.63674438551515));
#33246=CARTESIAN_POINT('Ctrl Pts',(37.5,32.1719479119405,3.83741678103717));
#33247=CARTESIAN_POINT('Ctrl Pts',(37.5185015343068,32.196767041805,3.8167935066088));
#33248=CARTESIAN_POINT('Ctrl Pts',(37.537045458494,32.2215810445749,3.79642837193837));
#33249=CARTESIAN_POINT('Ctrl Pts',(37.599346002575,32.304749523158,3.72899576964524));
#33250=CARTESIAN_POINT('Ctrl Pts',(37.6438438231274,32.3638269827301,3.6824593977772));
#33251=CARTESIAN_POINT('Ctrl Pts',(37.6890795305109,32.4235777807772,3.63674438551516));
#33252=CARTESIAN_POINT('Origin',(36.8,37.284736894758,9.9904151409573));
#33253=CARTESIAN_POINT('Ctrl Pts',(37.6890795305109,29.8980142324913,13.062275865462));
#33254=CARTESIAN_POINT('Ctrl Pts',(37.6438438231274,29.8691260296172,12.9928101044853));
#33255=CARTESIAN_POINT('Ctrl Pts',(37.599346002575,29.8412316347707,12.9229696944615));
#33256=CARTESIAN_POINT('Ctrl Pts',(37.537045458494,29.8029219206701,12.8229871085408));
#33257=CARTESIAN_POINT('Ctrl Pts',(37.5185015343068,29.791614931237,12.7929433831798));
#33258=CARTESIAN_POINT('Ctrl Pts',(37.5,29.7804325714888,12.7626735386834));
#33259=CARTESIAN_POINT('Origin',(39.5,32.6502398797874,3.24221525613641));
#33260=CARTESIAN_POINT('',(41.,32.8769019787977,2.84768612675766));
#33261=CARTESIAN_POINT('Ctrl Pts',(41.1878146546253,32.6518945010449,3.23933521449283));
#33262=CARTESIAN_POINT('Ctrl Pts',(41.0954573242617,32.7640771770245,3.04406951423305));
#33263=CARTESIAN_POINT('Ctrl Pts',(41.,32.8769019787977,2.84768612675766));
#33264=CARTESIAN_POINT('',(38.,32.8769019787977,2.84768612675766));
#33265=CARTESIAN_POINT('',(39.5,32.8769019787977,2.84768612675766));
#33266=CARTESIAN_POINT('Ctrl Pts',(38.,32.8769019787977,2.84768612675766));
#33267=CARTESIAN_POINT('Ctrl Pts',(37.8392820392456,32.6489512516586,3.24445824839666));
#33268=CARTESIAN_POINT('Ctrl Pts',(37.6890795305109,32.4235777807772,3.63674438551515));
#33269=CARTESIAN_POINT('Origin',(39.5,0.,0.));
#33270=CARTESIAN_POINT('Origin',(38.,0.,0.));
#33271=CARTESIAN_POINT('',(40.9,-32.9658914637539,-1.5));
#33272=CARTESIAN_POINT('Origin',(40.9,0.,0.));
#33273=CARTESIAN_POINT('',(38.,-32.9658914637539,-1.49999999999998));
#33274=CARTESIAN_POINT('Ctrl Pts',(40.9,-32.9658914637539,-1.5));
#33275=CARTESIAN_POINT('Ctrl Pts',(39.9333333333333,-32.9658914637539,-1.5));
#33276=CARTESIAN_POINT('Ctrl Pts',(38.9666666666667,-32.9658914637539,-1.5));
#33277=CARTESIAN_POINT('Ctrl Pts',(38.,-32.9658914637539,-1.5));
#33278=CARTESIAN_POINT('',(38.,-32.8769019787977,-2.84768612675766));
#33279=CARTESIAN_POINT('Origin',(38.,0.,0.));
#33280=CARTESIAN_POINT('',(39.5,-32.8769019787977,-2.84768612675766));
#33281=CARTESIAN_POINT('Origin',(39.5,-32.6502398797874,-3.2422152561364));
#33282=CARTESIAN_POINT('',(37.6890795305109,-32.4235777807772,-3.63674438551514));
#33283=CARTESIAN_POINT('Ctrl Pts',(38.,-32.8769019787977,-2.84768612675766));
#33284=CARTESIAN_POINT('Ctrl Pts',(37.8392820392454,-32.6489512516582,-3.24445824839731));
#33285=CARTESIAN_POINT('Ctrl Pts',(37.6890795305109,-32.4235777807772,-3.63674438551514));
#33286=CARTESIAN_POINT('',(41.,-32.4235777807772,-3.63674438551514));
#33287=CARTESIAN_POINT('',(39.5,-32.4235777807772,-3.63674438551514));
#33288=CARTESIAN_POINT('Ctrl Pts',(41.,-32.4235777807772,-3.63674438551515));
#33289=CARTESIAN_POINT('Ctrl Pts',(41.0874190154268,-32.5364116617262,-3.4403452176206));
#33290=CARTESIAN_POINT('Ctrl Pts',(41.1878146339919,-32.6518945107659,-3.23933522040983));
#33291=CARTESIAN_POINT('Origin',(41.25,-37.284736894758,-9.9904151409573));
#33292=CARTESIAN_POINT('',(41.,-29.8980142324913,-13.062275865462));
#33293=CARTESIAN_POINT('Origin',(41.,-37.284736894758,-9.9904151409573));
#33294=CARTESIAN_POINT('',(41.1878146546253,-29.8970377268407,-13.5206006633981));
#33295=CARTESIAN_POINT('Ctrl Pts',(41.,-29.8980142324913,-13.062275865462));
#33296=CARTESIAN_POINT('Ctrl Pts',(41.0874190341598,-29.8975316444848,-13.2887794709034));
#33297=CARTESIAN_POINT('Ctrl Pts',(41.1878146546253,-29.8970377268407,-13.5206006633981));
#33298=CARTESIAN_POINT('Ctrl Pts',(41.1878146546253,-29.8970377268407,-13.5206006633982));
#33299=CARTESIAN_POINT('Ctrl Pts',(41.2916290694684,-29.7825557217404,-13.5218058616421));
#33300=CARTESIAN_POINT('Ctrl Pts',(41.3956920266496,-29.6679695598581,-13.5223797770449));
#33301=CARTESIAN_POINT('Ctrl Pts',(41.5,-29.553277056526,-13.5223450340618));
#33302=CARTESIAN_POINT('Origin',(41.25,0.,0.));
#33303=CARTESIAN_POINT('',(41.,-29.8960753747485,-13.9722824616222));
#33304=CARTESIAN_POINT('Ctrl Pts',(41.,-29.8960753747485,-13.9722824616222));
#33305=CARTESIAN_POINT('Ctrl Pts',(41.0954573242615,-29.8965579239737,-13.7457970583011));
#33306=CARTESIAN_POINT('Ctrl Pts',(41.1878146546253,-29.8970377268408,-13.5206006633981));
#33307=CARTESIAN_POINT('',(41.,-27.0483892479909,-18.9046195171755));
#33308=CARTESIAN_POINT('Origin',(41.,0.,0.));
#33309=CARTESIAN_POINT('',(41.1878146339919,-26.657702517808,-19.1312938476315));
#33310=CARTESIAN_POINT('Ctrl Pts',(41.1878146339919,-26.657702517808,-19.1312938476315));
#33311=CARTESIAN_POINT('Ctrl Pts',(41.0954573053599,-26.8524884122035,-19.0182801301921));
#33312=CARTESIAN_POINT('Ctrl Pts',(41.,-27.0483892479909,-18.9046195171755));
#33313=CARTESIAN_POINT('Ctrl Pts',(41.5,-26.4873328464988,-18.8327161790004));
#33314=CARTESIAN_POINT('Ctrl Pts',(41.3957085374147,-26.5447001044493,-18.9320097094941));
#33315=CARTESIAN_POINT('Ctrl Pts',(41.2916417560968,-26.6014983745743,-19.031534724209));
#33316=CARTESIAN_POINT('Ctrl Pts',(41.1878146339919,-26.6577025235173,-19.1312938574718));
#33317=CARTESIAN_POINT('Origin',(39.5,-29.8970448036199,-13.5172791635421));
#33318=CARTESIAN_POINT('',(37.6890795305109,-29.8980142324913,-13.062275865462));
#33319=CARTESIAN_POINT('',(39.5,-29.8980142324913,-13.062275865462));
#33320=CARTESIAN_POINT('',(38.,-29.8960753747485,-13.9722824616222));
#33321=CARTESIAN_POINT('Ctrl Pts',(37.6890795305109,-29.8980142324913,-13.062275865462));
#33322=CARTESIAN_POINT('Ctrl Pts',(37.8392820392454,-29.8970503150544,-13.5146923611991));
#33323=CARTESIAN_POINT('Ctrl Pts',(38.,-29.8960753747485,-13.9722824616222));
#33324=CARTESIAN_POINT('',(39.5,-29.8960753747485,-13.9722824616222));
#33325=CARTESIAN_POINT('Origin',(39.5,0.,0.));
#33326=CARTESIAN_POINT('Origin',(38.,0.,0.));
#33327=CARTESIAN_POINT('',(40.9,-27.7992994660114,-17.7819838375536));
#33328=CARTESIAN_POINT('Origin',(40.9,0.,0.));
#33329=CARTESIAN_POINT('',(38.,-27.7992994660114,-17.7819838375536));
#33330=CARTESIAN_POINT('Ctrl Pts',(40.9,-27.7992994660114,-17.7819838375536));
#33331=CARTESIAN_POINT('Ctrl Pts',(39.9333333333333,-27.7992994660114,-17.7819838375536));
#33332=CARTESIAN_POINT('Ctrl Pts',(38.9666666666667,-27.7992994660114,-17.7819838375536));
#33333=CARTESIAN_POINT('Ctrl Pts',(38.,-27.7992994660114,-17.7819838375536));
#33334=CARTESIAN_POINT('',(38.,-27.0483892479909,-18.9046195171755));
#33335=CARTESIAN_POINT('Origin',(38.,0.,0.));
#33336=CARTESIAN_POINT('',(39.5,-27.0483892479909,-18.9046195171755));
#33337=CARTESIAN_POINT('Origin',(39.5,-26.6548295474835,-19.1329607162453));
#33338=CARTESIAN_POINT('',(37.6890795305109,-26.2612698469761,-19.3613019153151));
#33339=CARTESIAN_POINT('Ctrl Pts',(38.,-27.0483892479909,-18.9046195171755));
#33340=CARTESIAN_POINT('Ctrl Pts',(37.8392820392455,-26.6525920666573,-19.134258890459));
#33341=CARTESIAN_POINT('Ctrl Pts',(37.6890795305109,-26.2612698469761,-19.3613019153151));
#33342=CARTESIAN_POINT('',(41.,-26.2612698469761,-19.3613019153151));
#33343=CARTESIAN_POINT('',(39.5,-26.2612698469761,-19.3613019153151));
#33344=CARTESIAN_POINT('Ctrl Pts',(41.,-26.2612698469761,-19.3613019153151));
#33345=CARTESIAN_POINT('Ctrl Pts',(41.0874190154268,-26.4571864382328,-19.2476321871108));
#33346=CARTESIAN_POINT('Ctrl Pts',(41.1878146339919,-26.657702517808,-19.1312938476315));
#33347=CARTESIAN_POINT('Origin',(41.25,-27.2943217538008,-27.2943217538007));
#33348=CARTESIAN_POINT('',(41.,-19.3613019153151,-26.2612698469761));
#33349=CARTESIAN_POINT('Origin',(41.,-27.2943217538008,-27.2943217538007));
#33350=CARTESIAN_POINT('',(41.1878146546253,-19.1312938376468,-26.6577025123479));
#33351=CARTESIAN_POINT('Ctrl Pts',(41.,-19.3613019153151,-26.2612698469761));
#33352=CARTESIAN_POINT('Ctrl Pts',(41.0874190341598,-19.2476321791213,-26.4571864293338));
#33353=CARTESIAN_POINT('Ctrl Pts',(41.1878146546253,-19.1312938376468,-26.6577025123479));
#33354=CARTESIAN_POINT('Ctrl Pts',(41.1878146546253,-19.1312938376468,-26.6577025123479));
#33355=CARTESIAN_POINT('Ctrl Pts',(41.2916290694684,-19.0315469138318,-26.6015052420936));
#33356=CARTESIAN_POINT('Ctrl Pts',(41.3956920266496,-18.9320254290181,-26.5447091864709));
#33357=CARTESIAN_POINT('Ctrl Pts',(41.5,-18.8327161790004,-26.4873328464988));
#33358=CARTESIAN_POINT('Origin',(41.25,0.,0.));
#33359=CARTESIAN_POINT('',(41.,-18.9046195171755,-27.0483892479908));
#33360=CARTESIAN_POINT('Ctrl Pts',(41.,-18.9046195171755,-27.0483892479908));
#33361=CARTESIAN_POINT('Ctrl Pts',(41.0954573242616,-19.0182801187237,-26.8524884097409));
#33362=CARTESIAN_POINT('Ctrl Pts',(41.1878146546253,-19.1312938376468,-26.6577025123479));
#33363=CARTESIAN_POINT('',(41.,-13.9722824616222,-29.8960753747485));
#33364=CARTESIAN_POINT('Origin',(41.,0.,0.));
#33365=CARTESIAN_POINT('',(41.1878146339919,-13.5206006631344,-29.8970377382179));
#33366=CARTESIAN_POINT('Ctrl Pts',(41.1878146339919,-13.5206006631344,-29.8970377382179));
#33367=CARTESIAN_POINT('Ctrl Pts',(41.0954573053598,-13.7457970546997,-29.8965579351369));
#33368=CARTESIAN_POINT('Ctrl Pts',(41.,-13.9722824616222,-29.8960753747485));
#33369=CARTESIAN_POINT('Ctrl Pts',(41.5,-13.5223450340618,-29.553277056526));
#33370=CARTESIAN_POINT('Ctrl Pts',(41.3957085374147,-13.5223797715455,-29.6679514053401));
#33371=CARTESIAN_POINT('Ctrl Pts',(41.2916417560968,-13.5218060090073,-29.7825417314578));
#33372=CARTESIAN_POINT('Ctrl Pts',(41.1878146339919,-13.5206006631586,-29.8970377495944));
#33373=CARTESIAN_POINT('Origin',(39.5,-19.1329607162453,-26.6548295474835));
#33374=CARTESIAN_POINT('',(37.6890795305109,-19.3613019153152,-26.2612698469761));
#33375=CARTESIAN_POINT('',(39.5,-19.3613019153151,-26.2612698469761));
#33376=CARTESIAN_POINT('',(38.,-18.9046195171755,-27.0483892479908));
#33377=CARTESIAN_POINT('Ctrl Pts',(37.6890795305109,-19.3613019153152,-26.2612698469761));
#33378=CARTESIAN_POINT('Ctrl Pts',(37.8392820392454,-19.1342588904591,-26.6525920666571));
#33379=CARTESIAN_POINT('Ctrl Pts',(38.,-18.9046195171755,-27.0483892479908));
#33380=CARTESIAN_POINT('',(39.5,-18.9046195171755,-27.0483892479908));
#33381=CARTESIAN_POINT('Origin',(39.5,0.,0.));
#33382=CARTESIAN_POINT('Origin',(38.,0.,0.));
#33383=CARTESIAN_POINT('',(40.9,-15.1839076262003,-29.2992994660114));
#33384=CARTESIAN_POINT('Origin',(40.9,0.,0.));
#33385=CARTESIAN_POINT('',(38.,-15.1839076262003,-29.2992994660114));
#33386=CARTESIAN_POINT('Ctrl Pts',(40.9,-15.1839076262003,-29.2992994660114));
#33387=CARTESIAN_POINT('Ctrl Pts',(39.9333333333333,-15.1839076262003,-29.2992994660114));
#33388=CARTESIAN_POINT('Ctrl Pts',(38.9666666666667,-15.1839076262003,-29.2992994660114));
#33389=CARTESIAN_POINT('Ctrl Pts',(38.,-15.1839076262003,-29.2992994660114));
#33390=CARTESIAN_POINT('',(38.,-13.9722824616222,-29.8960753747485));
#33391=CARTESIAN_POINT('Origin',(38.,0.,0.));
#33392=CARTESIAN_POINT('',(39.5,-13.9722824616222,-29.8960753747485));
#33393=CARTESIAN_POINT('Origin',(39.5,-13.5172791635421,-29.8970448036199));
#33394=CARTESIAN_POINT('',(37.6890795305109,-13.0622758654621,-29.8980142324913));
#33395=CARTESIAN_POINT('Ctrl Pts',(38.,-13.9722824616222,-29.8960753747485));
#33396=CARTESIAN_POINT('Ctrl Pts',(37.8392820392453,-13.5146923611989,-29.8970503150544));
#33397=CARTESIAN_POINT('Ctrl Pts',(37.6890795305109,-13.0622758654621,-29.8980142324913));
#33398=CARTESIAN_POINT('',(41.,-13.0622758654621,-29.8980142324913));
#33399=CARTESIAN_POINT('',(39.5,-13.0622758654621,-29.8980142324913));
#33400=CARTESIAN_POINT('Ctrl Pts',(41.,-13.0622758654621,-29.8980142324913));
#33401=CARTESIAN_POINT('Ctrl Pts',(41.0874190154268,-13.2887794746153,-29.8975316558534));
#33402=CARTESIAN_POINT('Ctrl Pts',(41.1878146339919,-13.5206006631344,-29.8970377382179));
#33403=CARTESIAN_POINT('Origin',(41.25,-9.99041514095732,-37.284736894758));
#33404=CARTESIAN_POINT('',(41.,-3.63674438551517,-32.4235777807772));
#33405=CARTESIAN_POINT('Origin',(41.,-9.99041514095732,-37.284736894758));
#33406=CARTESIAN_POINT('',(41.1878146546253,-3.23933521449285,-32.6518945010449));
#33407=CARTESIAN_POINT('Ctrl Pts',(41.,-3.63674438551517,-32.4235777807772));
#33408=CARTESIAN_POINT('Ctrl Pts',(41.0874190341598,-3.44034521515094,-32.5364116500246));
#33409=CARTESIAN_POINT('Ctrl Pts',(41.1878146546253,-3.23933521449285,-32.6518945010449));
#33410=CARTESIAN_POINT('Ctrl Pts',(41.1878146546253,-3.23933521449285,-32.6518945010449));
#33411=CARTESIAN_POINT('Ctrl Pts',(41.2916290694684,-3.18105047964687,-32.5533527754738));
#33412=CARTESIAN_POINT('Ctrl Pts',(41.3956920266496,-3.12326037338726,-32.454405206063));
#33413=CARTESIAN_POINT('Ctrl Pts',(41.5,-3.06594421002717,-32.3550612130622));
#33414=CARTESIAN_POINT('Origin',(41.25,0.,0.));
#33415=CARTESIAN_POINT('',(41.,-2.84768612675768,-32.8769019787977));
#33416=CARTESIAN_POINT('Ctrl Pts',(41.,-2.84768612675768,-32.8769019787977));
#33417=CARTESIAN_POINT('Ctrl Pts',(41.0954573242614,-3.04406951423239,-32.7640771770249));
#33418=CARTESIAN_POINT('Ctrl Pts',(41.1878146546253,-3.23933521449284,-32.6518945010449));
#33419=CARTESIAN_POINT('',(41.,2.84768612675766,-32.8769019787977));
#33420=CARTESIAN_POINT('Origin',(41.,0.,0.));
#33421=CARTESIAN_POINT('',(41.1878146339919,3.23933522040982,-32.6518945107659));
#33422=CARTESIAN_POINT('Ctrl Pts',(41.1878146339919,3.23933522040982,-32.6518945107659));
#33423=CARTESIAN_POINT('Ctrl Pts',(41.0954573053598,3.04406952293321,-32.7640771848917));
#33424=CARTESIAN_POINT('Ctrl Pts',(41.,2.84768612675766,-32.8769019787977));
#33425=CARTESIAN_POINT('Ctrl Pts',(41.5,3.06594421002715,-32.3550612130622));
#33426=CARTESIAN_POINT('Ctrl Pts',(41.3957085374147,3.12325130089087,-32.4543894810395));
#33427=CARTESIAN_POINT('Ctrl Pts',(41.2916417560968,3.18104335688356,-32.5533407332163));
#33428=CARTESIAN_POINT('Ctrl Pts',(41.1878146339919,3.2393352260771,-32.6518945206304));
#33429=CARTESIAN_POINT('Origin',(39.5,-3.24221525613642,-32.6502398797874));
#33430=CARTESIAN_POINT('',(37.6890795305109,-3.63674438551517,-32.4235777807772));
#33431=CARTESIAN_POINT('',(39.5,-3.63674438551517,-32.4235777807772));
#33432=CARTESIAN_POINT('',(38.,-2.84768612675768,-32.8769019787977));
#33433=CARTESIAN_POINT('Ctrl Pts',(37.6890795305109,-3.63674438551517,-32.4235777807772));
#33434=CARTESIAN_POINT('Ctrl Pts',(37.8392820392455,-3.24445824839701,-32.6489512516584));
#33435=CARTESIAN_POINT('Ctrl Pts',(38.,-2.84768612675768,-32.8769019787977));
#33436=CARTESIAN_POINT('',(39.5,-2.84768612675768,-32.8769019787977));
#33437=CARTESIAN_POINT('Origin',(39.5,0.,0.));
#33438=CARTESIAN_POINT('Origin',(38.,0.,0.));
#33439=CARTESIAN_POINT('',(40.9,1.5,-32.9658914637539));
#33440=CARTESIAN_POINT('Origin',(40.9,0.,0.));
#33441=CARTESIAN_POINT('',(38.,1.49999999999998,-32.9658914637539));
#33442=CARTESIAN_POINT('Ctrl Pts',(40.9,1.49999999999999,-32.9658914637539));
#33443=CARTESIAN_POINT('Ctrl Pts',(39.9333333333333,1.49999999999999,-32.9658914637539));
#33444=CARTESIAN_POINT('Ctrl Pts',(38.9666666666667,1.49999999999999,-32.9658914637539));
#33445=CARTESIAN_POINT('Ctrl Pts',(38.,1.49999999999999,-32.9658914637539));
#33446=CARTESIAN_POINT('',(38.,2.84768612675766,-32.8769019787977));
#33447=CARTESIAN_POINT('Origin',(38.,0.,0.));
#33448=CARTESIAN_POINT('',(39.5,2.84768612675766,-32.8769019787977));
#33449=CARTESIAN_POINT('Origin',(39.5,3.2422152561364,-32.6502398797874));
#33450=CARTESIAN_POINT('',(37.6890795305109,3.63674438551514,-32.4235777807772));
#33451=CARTESIAN_POINT('Ctrl Pts',(38.,2.84768612675766,-32.8769019787977));
#33452=CARTESIAN_POINT('Ctrl Pts',(37.8392820392455,3.24445824839707,-32.6489512516583));
#33453=CARTESIAN_POINT('Ctrl Pts',(37.6890795305109,3.63674438551514,-32.4235777807772));
#33454=CARTESIAN_POINT('',(41.,3.63674438551514,-32.4235777807772));
#33455=CARTESIAN_POINT('',(39.5,3.63674438551514,-32.4235777807772));
#33456=CARTESIAN_POINT('Ctrl Pts',(41.,3.63674438551514,-32.4235777807772));
#33457=CARTESIAN_POINT('Ctrl Pts',(41.0874190154268,3.44034521762059,-32.5364116617262));
#33458=CARTESIAN_POINT('Ctrl Pts',(41.1878146339919,3.23933522040982,-32.6518945107659));
#33459=CARTESIAN_POINT('Origin',(41.25,9.99041514095729,-37.284736894758));
#33460=CARTESIAN_POINT('',(41.,13.0622758654621,-29.8980142324913));
#33461=CARTESIAN_POINT('Origin',(41.,9.99041514095729,-37.284736894758));
#33462=CARTESIAN_POINT('',(41.1878146546253,13.5206006633982,-29.8970377268407));
#33463=CARTESIAN_POINT('Ctrl Pts',(41.,13.0622758654621,-29.8980142324913));
#33464=CARTESIAN_POINT('Ctrl Pts',(41.0874190341598,13.2887794709034,-29.8975316444848));
#33465=CARTESIAN_POINT('Ctrl Pts',(41.1878146546253,13.5206006633982,-29.8970377268407));
#33466=CARTESIAN_POINT('Ctrl Pts',(41.1878146546253,13.5206006633982,-29.8970377268407));
#33467=CARTESIAN_POINT('Ctrl Pts',(41.2916290694684,13.5218058616421,-29.7825557217404));
#33468=CARTESIAN_POINT('Ctrl Pts',(41.3956920266496,13.5223797770449,-29.6679695598581));
#33469=CARTESIAN_POINT('Ctrl Pts',(41.5,13.5223450340618,-29.553277056526));
#33470=CARTESIAN_POINT('Origin',(41.25,0.,0.));
#33471=CARTESIAN_POINT('',(41.,13.9722824616222,-29.8960753747485));
#33472=CARTESIAN_POINT('Ctrl Pts',(41.,13.9722824616222,-29.8960753747485));
#33473=CARTESIAN_POINT('Ctrl Pts',(41.0954573242616,13.745797058301,-29.8965579239736));
#33474=CARTESIAN_POINT('Ctrl Pts',(41.1878146546253,13.5206006633982,-29.8970377268407));
#33475=CARTESIAN_POINT('',(41.,18.9046195171755,-27.0483892479909));
#33476=CARTESIAN_POINT('Origin',(41.,0.,0.));
#33477=CARTESIAN_POINT('',(41.1878146339919,19.1312938476315,-26.6577025178081));
#33478=CARTESIAN_POINT('Ctrl Pts',(41.1878146339919,19.1312938476315,-26.6577025178081));
#33479=CARTESIAN_POINT('Ctrl Pts',(41.09545730536,19.0182801301922,-26.8524884122034));
#33480=CARTESIAN_POINT('Ctrl Pts',(41.,18.9046195171755,-27.0483892479909));
#33481=CARTESIAN_POINT('Ctrl Pts',(41.5,18.8327161790004,-26.4873328464988));
#33482=CARTESIAN_POINT('Ctrl Pts',(41.3957085374147,18.932009709494,-26.5447001044493));
#33483=CARTESIAN_POINT('Ctrl Pts',(41.2916417560968,19.031534724209,-26.6014983745743));
#33484=CARTESIAN_POINT('Ctrl Pts',(41.1878146339919,19.1312938574718,-26.6577025235173));
#33485=CARTESIAN_POINT('Origin',(39.5,13.5172791635421,-29.8970448036199));
#33486=CARTESIAN_POINT('',(37.6890795305109,13.0622758654621,-29.8980142324913));
#33487=CARTESIAN_POINT('',(39.5,13.0622758654621,-29.8980142324913));
#33488=CARTESIAN_POINT('',(38.,13.9722824616222,-29.8960753747485));
#33489=CARTESIAN_POINT('Ctrl Pts',(37.6890795305109,13.0622758654621,-29.8980142324913));
#33490=CARTESIAN_POINT('Ctrl Pts',(37.8392820392456,13.5146923611998,-29.8970503150544));
#33491=CARTESIAN_POINT('Ctrl Pts',(38.,13.9722824616222,-29.8960753747485));
#33492=CARTESIAN_POINT('',(39.5,13.9722824616222,-29.8960753747485));
#33493=CARTESIAN_POINT('Origin',(39.5,0.,0.));
#33494=CARTESIAN_POINT('Origin',(38.,0.,0.));
#33495=CARTESIAN_POINT('',(40.9,17.7819838375536,-27.7992994660114));
#33496=CARTESIAN_POINT('Origin',(40.9,0.,0.));
#33497=CARTESIAN_POINT('',(38.,17.7819838375536,-27.7992994660114));
#33498=CARTESIAN_POINT('Ctrl Pts',(40.9,17.7819838375536,-27.7992994660114));
#33499=CARTESIAN_POINT('Ctrl Pts',(39.9333333333333,17.7819838375536,-27.7992994660114));
#33500=CARTESIAN_POINT('Ctrl Pts',(38.9666666666667,17.7819838375536,-27.7992994660114));
#33501=CARTESIAN_POINT('Ctrl Pts',(38.,17.7819838375536,-27.7992994660114));
#33502=CARTESIAN_POINT('',(38.,18.9046195171755,-27.0483892479909));
#33503=CARTESIAN_POINT('Origin',(38.,0.,0.));
#33504=CARTESIAN_POINT('',(39.5,18.9046195171755,-27.0483892479909));
#33505=CARTESIAN_POINT('Origin',(39.5,19.1329607162453,-26.6548295474835));
#33506=CARTESIAN_POINT('',(37.6890795305109,19.3613019153151,-26.2612698469762));
#33507=CARTESIAN_POINT('Ctrl Pts',(38.,18.9046195171755,-27.0483892479909));
#33508=CARTESIAN_POINT('Ctrl Pts',(37.8392820392454,19.1342588904591,-26.6525920666571));
#33509=CARTESIAN_POINT('Ctrl Pts',(37.6890795305109,19.3613019153151,-26.2612698469762));
#33510=CARTESIAN_POINT('',(41.,19.3613019153151,-26.2612698469762));
#33511=CARTESIAN_POINT('',(39.5,19.3613019153151,-26.2612698469762));
#33512=CARTESIAN_POINT('Ctrl Pts',(41.,19.3613019153151,-26.2612698469762));
#33513=CARTESIAN_POINT('Ctrl Pts',(41.0874190154268,19.2476321871109,-26.4571864382327));
#33514=CARTESIAN_POINT('Ctrl Pts',(41.1878146339919,19.1312938476315,-26.6577025178081));
#33515=CARTESIAN_POINT('Origin',(41.25,27.2943217538007,-27.2943217538008));
#33516=CARTESIAN_POINT('',(41.,26.2612698469761,-19.3613019153152));
#33517=CARTESIAN_POINT('Origin',(41.,27.2943217538007,-27.2943217538008));
#33518=CARTESIAN_POINT('',(41.1878146546253,26.6577025123479,-19.1312938376468));
#33519=CARTESIAN_POINT('Ctrl Pts',(41.,26.2612698469761,-19.3613019153152));
#33520=CARTESIAN_POINT('Ctrl Pts',(41.0874190341598,26.4571864293338,-19.2476321791213));
#33521=CARTESIAN_POINT('Ctrl Pts',(41.1878146546253,26.6577025123479,-19.1312938376468));
#33522=CARTESIAN_POINT('Ctrl Pts',(41.1878146546253,26.6577025123479,-19.1312938376468));
#33523=CARTESIAN_POINT('Ctrl Pts',(41.2916290694684,26.6015052420936,-19.0315469138318));
#33524=CARTESIAN_POINT('Ctrl Pts',(41.3956920266496,26.5447091864709,-18.9320254290182));
#33525=CARTESIAN_POINT('Ctrl Pts',(41.5,26.4873328464988,-18.8327161790004));
#33526=CARTESIAN_POINT('Origin',(41.25,0.,0.));
#33527=CARTESIAN_POINT('',(41.,27.0483892479908,-18.9046195171755));
#33528=CARTESIAN_POINT('Ctrl Pts',(41.,27.0483892479908,-18.9046195171755));
#33529=CARTESIAN_POINT('Ctrl Pts',(41.0954573242615,26.852488409741,-19.0182801187236));
#33530=CARTESIAN_POINT('Ctrl Pts',(41.1878146546253,26.6577025123479,-19.1312938376468));
#33531=CARTESIAN_POINT('',(41.,29.8960753747485,-13.9722824616222));
#33532=CARTESIAN_POINT('Origin',(41.,0.,0.));
#33533=CARTESIAN_POINT('',(41.1878146339919,29.8970377382179,-13.5206006631344));
#33534=CARTESIAN_POINT('Ctrl Pts',(41.1878146339919,29.8970377382179,-13.5206006631344));
#33535=CARTESIAN_POINT('Ctrl Pts',(41.0954573053599,29.8965579351369,-13.7457970546994));
#33536=CARTESIAN_POINT('Ctrl Pts',(41.,29.8960753747485,-13.9722824616222));
#33537=CARTESIAN_POINT('Ctrl Pts',(41.5,29.553277056526,-13.5223450340618));
#33538=CARTESIAN_POINT('Ctrl Pts',(41.3957085374147,29.6679514053401,-13.5223797715455));
#33539=CARTESIAN_POINT('Ctrl Pts',(41.2916417560968,29.7825417314578,-13.5218060090073));
#33540=CARTESIAN_POINT('Ctrl Pts',(41.1878146339919,29.8970377495944,-13.5206006631586));
#33541=CARTESIAN_POINT('Origin',(39.5,26.6548295474835,-19.1329607162453));
#33542=CARTESIAN_POINT('',(37.6890795305109,26.2612698469761,-19.3613019153152));
#33543=CARTESIAN_POINT('',(39.5,26.2612698469761,-19.3613019153152));
#33544=CARTESIAN_POINT('',(38.,27.0483892479908,-18.9046195171755));
#33545=CARTESIAN_POINT('Ctrl Pts',(37.6890795305109,26.2612698469761,-19.3613019153152));
#33546=CARTESIAN_POINT('Ctrl Pts',(37.8392820392455,26.6525920666573,-19.1342588904591));
#33547=CARTESIAN_POINT('Ctrl Pts',(38.,27.0483892479908,-18.9046195171755));
#33548=CARTESIAN_POINT('',(39.5,27.0483892479908,-18.9046195171755));
#33549=CARTESIAN_POINT('Origin',(39.5,0.,0.));
#33550=CARTESIAN_POINT('',(41.,32.8769019787977,-2.84768612675768));
#33551=CARTESIAN_POINT('Origin',(41.,0.,0.));
#33552=CARTESIAN_POINT('',(38.,32.8769019787977,-2.84768612675768));
#33553=CARTESIAN_POINT('',(39.5,32.8769019787977,-2.84768612675768));
#33554=CARTESIAN_POINT('Origin',(38.,0.,0.));
#33555=CARTESIAN_POINT('',(40.9,32.9658914637539,1.5));
#33556=CARTESIAN_POINT('Origin',(40.9,0.,0.));
#33557=CARTESIAN_POINT('',(38.,32.9658914637539,1.5));
#33558=CARTESIAN_POINT('Ctrl Pts',(40.9,32.9658914637539,1.5));
#33559=CARTESIAN_POINT('Ctrl Pts',(39.9333333333333,32.9658914637539,1.5));
#33560=CARTESIAN_POINT('Ctrl Pts',(38.9666666666667,32.9658914637539,1.5));
#33561=CARTESIAN_POINT('Ctrl Pts',(38.,32.9658914637539,1.5));
#33562=CARTESIAN_POINT('Origin',(38.,0.,0.));
#33563=CARTESIAN_POINT('Origin',(41.25,0.,0.));
#33564=CARTESIAN_POINT('',(41.1878146546253,32.6518945010449,-3.23933521449284));
#33565=CARTESIAN_POINT('Ctrl Pts',(41.1878146546253,32.6518945010449,-3.23933521449285));
#33566=CARTESIAN_POINT('Ctrl Pts',(41.2916290694684,32.5533527754738,-3.18105047964687));
#33567=CARTESIAN_POINT('Ctrl Pts',(41.3956920266496,32.454405206063,-3.12326037338726));
#33568=CARTESIAN_POINT('Ctrl Pts',(41.5,32.3550612130622,-3.06594421002717));
#33569=CARTESIAN_POINT('Ctrl Pts',(41.,32.8769019787977,-2.84768612675768));
#33570=CARTESIAN_POINT('Ctrl Pts',(41.0954573242615,32.7640771770247,-3.04406951423265));
#33571=CARTESIAN_POINT('Ctrl Pts',(41.1878146546253,32.6518945010449,-3.23933521449285));
#33572=CARTESIAN_POINT('Origin',(39.5,0.,0.));
#33573=CARTESIAN_POINT('Origin',(38.,0.,0.));
#33574=CARTESIAN_POINT('',(40.9,29.2992994660114,-15.1839076262003));
#33575=CARTESIAN_POINT('Origin',(40.9,0.,0.));
#33576=CARTESIAN_POINT('',(38.,29.2992994660114,-15.1839076262003));
#33577=CARTESIAN_POINT('Ctrl Pts',(40.9,29.2992994660114,-15.1839076262003));
#33578=CARTESIAN_POINT('Ctrl Pts',(39.9333333333333,29.2992994660114,-15.1839076262003));
#33579=CARTESIAN_POINT('Ctrl Pts',(38.9666666666667,29.2992994660114,-15.1839076262003));
#33580=CARTESIAN_POINT('Ctrl Pts',(38.,29.2992994660114,-15.1839076262003));
#33581=CARTESIAN_POINT('',(38.,29.8960753747485,-13.9722824616222));
#33582=CARTESIAN_POINT('Origin',(38.,0.,0.));
#33583=CARTESIAN_POINT('',(39.5,29.8960753747485,-13.9722824616222));
#33584=CARTESIAN_POINT('Origin',(39.5,29.8970448036199,-13.5172791635421));
#33585=CARTESIAN_POINT('',(37.6890795305109,29.8980142324913,-13.0622758654621));
#33586=CARTESIAN_POINT('Ctrl Pts',(38.,29.8960753747485,-13.9722824616222));
#33587=CARTESIAN_POINT('Ctrl Pts',(37.8392820392455,29.8970503150544,-13.5146923611996));
#33588=CARTESIAN_POINT('Ctrl Pts',(37.6890795305109,29.8980142324913,-13.0622758654621));
#33589=CARTESIAN_POINT('',(41.,29.8980142324913,-13.0622758654621));
#33590=CARTESIAN_POINT('',(39.5,29.8980142324913,-13.0622758654621));
#33591=CARTESIAN_POINT('Ctrl Pts',(41.,29.8980142324913,-13.0622758654621));
#33592=CARTESIAN_POINT('Ctrl Pts',(41.0874190154268,29.8975316558534,-13.2887794746153));
#33593=CARTESIAN_POINT('Ctrl Pts',(41.1878146339919,29.8970377382179,-13.5206006631344));
#33594=CARTESIAN_POINT('Origin',(41.25,37.284736894758,-9.99041514095732));
#33595=CARTESIAN_POINT('',(41.,32.4235777807772,-3.63674438551517));
#33596=CARTESIAN_POINT('Origin',(41.,37.284736894758,-9.99041514095732));
#33597=CARTESIAN_POINT('Ctrl Pts',(41.,32.4235777807772,-3.63674438551517));
#33598=CARTESIAN_POINT('Ctrl Pts',(41.0874190341598,32.5364116500246,-3.44034521515093));
#33599=CARTESIAN_POINT('Ctrl Pts',(41.1878146546253,32.6518945010449,-3.23933521449284));
#33600=CARTESIAN_POINT('Origin',(39.5,32.6502398797874,-3.24221525613642));
#33601=CARTESIAN_POINT('',(37.6890795305109,32.4235777807772,-3.63674438551517));
#33602=CARTESIAN_POINT('',(39.5,32.4235777807772,-3.63674438551517));
#33603=CARTESIAN_POINT('Ctrl Pts',(37.6890795305109,32.4235777807772,-3.63674438551517));
#33604=CARTESIAN_POINT('Ctrl Pts',(37.8392820392455,32.6489512516583,-3.24445824839707));
#33605=CARTESIAN_POINT('Ctrl Pts',(38.,32.8769019787977,-2.84768612675768));
#33606=CARTESIAN_POINT('Origin',(37.75,0.,0.));
#33607=CARTESIAN_POINT('',(37.5,32.1719479119405,-3.83741678103716));
#33608=CARTESIAN_POINT('Ctrl Pts',(37.6890795305109,32.4235777807772,-3.63674438551516));
#33609=CARTESIAN_POINT('Ctrl Pts',(37.6438438231274,32.3638269827301,-3.68245939777721));
#33610=CARTESIAN_POINT('Ctrl Pts',(37.599346002575,32.304749523158,-3.72899576964525));
#33611=CARTESIAN_POINT('Ctrl Pts',(37.537045458494,32.2215810445749,-3.79642837193839));
#33612=CARTESIAN_POINT('Ctrl Pts',(37.5185015343068,32.196767041805,-3.81679350660881));
#33613=CARTESIAN_POINT('Ctrl Pts',(37.5,32.1719479119405,-3.83741678103718));
#33614=CARTESIAN_POINT('Origin',(37.5,0.,0.));
#33615=CARTESIAN_POINT('Origin',(36.8,37.284736894758,-9.99041514095732));
#33616=CARTESIAN_POINT('',(37.5,29.7804325714888,-12.7626735386834));
#33617=CARTESIAN_POINT('Ctrl Pts',(37.5,29.7804325714888,-12.7626735386834));
#33618=CARTESIAN_POINT('Ctrl Pts',(37.5185015343068,29.791614931237,-12.7929433831798));
#33619=CARTESIAN_POINT('Ctrl Pts',(37.537045458494,29.8029219206701,-12.8229871085408));
#33620=CARTESIAN_POINT('Ctrl Pts',(37.599346002575,29.8412316347707,-12.9229696944615));
#33621=CARTESIAN_POINT('Ctrl Pts',(37.6438438231274,29.8691260296172,-12.9928101044853));
#33622=CARTESIAN_POINT('Ctrl Pts',(37.6890795305109,29.8980142324913,-13.0622758654621));
#33623=CARTESIAN_POINT('',(36.8,29.4900464626661,-11.7911930472673));
#33624=CARTESIAN_POINT('Ctrl Pts',(36.8,29.4900464626661,-11.7911930472673));
#33625=CARTESIAN_POINT('Ctrl Pts',(37.0122659037828,29.5692859507914,-12.1341821953296));
#33626=CARTESIAN_POINT('Ctrl Pts',(37.2470086540955,29.6681218786624,-12.458656561616));
#33627=CARTESIAN_POINT('Ctrl Pts',(37.5,29.7804325714888,-12.7626735386834));
#33628=CARTESIAN_POINT('',(36.8,31.4347259190859,-4.53355051147316));
#33629=CARTESIAN_POINT('Origin',(36.8,37.284736894758,-9.99041514095732));
#33630=CARTESIAN_POINT('Ctrl Pts',(37.5,32.1719479119405,-3.83741678103719));
#33631=CARTESIAN_POINT('Ctrl Pts',(37.2470086540956,31.9226755103027,-4.04454785994595));
#33632=CARTESIAN_POINT('Ctrl Pts',(37.0122659037829,31.6748439028165,-4.27613294009144));
#33633=CARTESIAN_POINT('Ctrl Pts',(36.8,31.4347259190859,-4.53355051147316));
#33634=CARTESIAN_POINT('Origin',(173.058,8.10351388986772E-16,-1.22178682300763E-16));
#33635=CARTESIAN_POINT('',(173.058,-0.317020535431457,3.42736954239177));
#33636=CARTESIAN_POINT('Ctrl Pts',(173.058,2.6445394957829,-1.13133757670322));
#33637=CARTESIAN_POINT('Ctrl Pts',(173.058,2.68388676478393,-1.06040744504102));
#33638=CARTESIAN_POINT('Ctrl Pts',(173.058,2.71996664284584,-0.987874460436406));
#33639=CARTESIAN_POINT('Ctrl Pts',(173.058,2.75260599077044,-0.913896544786152));
#33640=CARTESIAN_POINT('Ctrl Pts',(173.058,2.79080948766531,-0.827307343391491));
#33641=CARTESIAN_POINT('Ctrl Pts',(173.058,2.82430130285621,-0.738739077560077));
#33642=CARTESIAN_POINT('Ctrl Pts',(173.058,2.85320325444538,-0.6485602460535));
#33643=CARTESIAN_POINT('Ctrl Pts',(173.058,2.87052216452721,-0.594522404721965));
#33644=CARTESIAN_POINT('Ctrl Pts',(173.058,2.8861921276262,-0.539905615643428));
#33645=CARTESIAN_POINT('Ctrl Pts',(173.058,2.90023180440349,-0.484784713552764));
#33646=CARTESIAN_POINT('Ctrl Pts',(173.058,2.90495816775042,-0.466228630287898));
#33647=CARTESIAN_POINT('Ctrl Pts',(173.058,2.90949972520718,-0.447615393832835));
#33648=CARTESIAN_POINT('Ctrl Pts',(173.058,2.91385704339701,-0.428947796047142));
#33649=CARTESIAN_POINT('Ctrl Pts',(173.058,2.91798497003428,-0.41126295624517));
#33650=CARTESIAN_POINT('Ctrl Pts',(173.058,2.92194557683693,-0.39353765489647));
#33651=CARTESIAN_POINT('Ctrl Pts',(173.058,2.92573901615535,-0.375778161205653));
#33652=CARTESIAN_POINT('Ctrl Pts',(173.058,2.94706671207049,-0.275929699361356));
#33653=CARTESIAN_POINT('Ctrl Pts',(173.058,2.96312338895318,-0.17496588958598));
#33654=CARTESIAN_POINT('Ctrl Pts',(173.058,2.97405583198172,-0.0733312989060914));
#33655=CARTESIAN_POINT('Ctrl Pts',(173.058,2.98362171963169,0.0155989679388112));
#33656=CARTESIAN_POINT('Ctrl Pts',(173.058,2.98926355991625,0.105043810517558));
#33657=CARTESIAN_POINT('Ctrl Pts',(173.058,2.99104538503735,0.194721159461318));
#33658=CARTESIAN_POINT('Ctrl Pts',(173.058,2.9919477288971,0.240135158972413));
#33659=CARTESIAN_POINT('Ctrl Pts',(173.058,2.99185963655175,0.285608966682687));
#33660=CARTESIAN_POINT('Ctrl Pts',(173.058,2.99078627853696,0.331106705631171));
#33661=CARTESIAN_POINT('Ctrl Pts',(173.058,2.99039011742852,0.347899271061504));
#33662=CARTESIAN_POINT('Ctrl Pts',(173.058,2.98985962973635,0.364695414585539));
#33663=CARTESIAN_POINT('Ctrl Pts',(173.058,2.98919583576813,0.381478052754939));
#33664=CARTESIAN_POINT('Ctrl Pts',(173.058,2.98517361899542,0.483171367196758));
#33665=CARTESIAN_POINT('Ctrl Pts',(173.058,2.97625835266948,0.584503472695341));
#33666=CARTESIAN_POINT('Ctrl Pts',(173.058,2.96258323513638,0.685067958781066));
#33667=CARTESIAN_POINT('Ctrl Pts',(173.058,2.94869737691069,0.787182196040461));
#33668=CARTESIAN_POINT('Ctrl Pts',(173.058,2.92990395107091,0.88850588487361));
#33669=CARTESIAN_POINT('Ctrl Pts',(173.058,2.90629107171056,0.988628707087666));
#33670=CARTESIAN_POINT('Ctrl Pts',(173.058,2.88278756415779,1.08828777332012));
#33671=CARTESIAN_POINT('Ctrl Pts',(173.058,2.85450910237203,1.18675804608544));
#33672=CARTESIAN_POINT('Ctrl Pts',(173.058,2.82149181038043,1.28363554367967));
#33673=CARTESIAN_POINT('Ctrl Pts',(173.058,2.80072893032535,1.34455682889888));
#33674=CARTESIAN_POINT('Ctrl Pts',(173.058,2.77809106867539,1.40484821518742));
#33675=CARTESIAN_POINT('Ctrl Pts',(173.058,2.75357694953202,1.46440672670599));
#33676=CARTESIAN_POINT('Ctrl Pts',(173.058,2.74765579823695,1.47879251619931));
#33677=CARTESIAN_POINT('Ctrl Pts',(173.058,2.74162514642604,1.49313553453836));
#33678=CARTESIAN_POINT('Ctrl Pts',(173.058,2.73548490672827,1.50743430130681));
#33679=CARTESIAN_POINT('Ctrl Pts',(173.058,2.7297149744626,1.52087073372598));
#33680=CARTESIAN_POINT('Ctrl Pts',(173.058,2.72385220696792,1.53425892684204));
#33681=CARTESIAN_POINT('Ctrl Pts',(173.058,2.71789703616041,1.54759752544682));
#33682=CARTESIAN_POINT('Ctrl Pts',(173.058,2.67487005930043,1.64397084404051));
#33683=CARTESIAN_POINT('Ctrl Pts',(173.058,2.6270219018787,1.737759129436));
#33684=CARTESIAN_POINT('Ctrl Pts',(173.058,2.57444790271155,1.82854142353784));
#33685=CARTESIAN_POINT('Ctrl Pts',(173.058,2.54586514607472,1.87789677523928));
#33686=CARTESIAN_POINT('Ctrl Pts',(173.058,2.51588464763651,1.92636367759785));
#33687=CARTESIAN_POINT('Ctrl Pts',(173.058,2.48451528981652,1.97387379690175));
#33688=CARTESIAN_POINT('Ctrl Pts',(173.058,2.4286458194415,2.05849029489302));
#33689=CARTESIAN_POINT('Ctrl Pts',(173.058,2.36837369723511,2.14007342029795));
#33690=CARTESIAN_POINT('Ctrl Pts',(173.058,2.30406148503067,2.21852057948255));
#33691=CARTESIAN_POINT('Ctrl Pts',(173.058,2.23853237955843,2.29845208847597));
#33692=CARTESIAN_POINT('Ctrl Pts',(173.058,2.16880835636398,2.37512837214474));
#33693=CARTESIAN_POINT('Ctrl Pts',(173.058,2.09522678862175,2.4484128735308));
#33694=CARTESIAN_POINT('Ctrl Pts',(173.058,2.0767086217718,2.46685627812007));
#33695=CARTESIAN_POINT('Ctrl Pts',(173.058,2.05794592621631,2.48508469783389));
#33696=CARTESIAN_POINT('Ctrl Pts',(173.058,2.03894369044655,2.5030956193348));
#33697=CARTESIAN_POINT('Ctrl Pts',(173.058,2.02757992226549,2.5138665590886));
#33698=CARTESIAN_POINT('Ctrl Pts',(173.058,2.01613687709355,2.52455362818136));
#33699=CARTESIAN_POINT('Ctrl Pts',(173.058,2.00461862649846,2.53515407788848));
#33700=CARTESIAN_POINT('Ctrl Pts',(173.058,1.92673714454547,2.60682978295701));
#33701=CARTESIAN_POINT('Ctrl Pts',(173.058,1.84538286439517,2.67458398376605));
#33702=CARTESIAN_POINT('Ctrl Pts',(173.058,1.76097463544042,2.73832174508392));
#33703=CARTESIAN_POINT('Ctrl Pts',(173.058,1.67547637152312,2.80288260610582));
#33704=CARTESIAN_POINT('Ctrl Pts',(173.058,1.58684416396937,2.86332314304966));
#33705=CARTESIAN_POINT('Ctrl Pts',(173.058,1.49546564431326,2.91951596239309));
#33706=CARTESIAN_POINT('Ctrl Pts',(173.058,1.40339423056955,2.97613487391262));
#33707=CARTESIAN_POINT('Ctrl Pts',(173.058,1.30853399756601,3.02844194726936));
#33708=CARTESIAN_POINT('Ctrl Pts',(173.058,1.21124337720924,3.07626987325074));
#33709=CARTESIAN_POINT('Ctrl Pts',(173.058,1.15206303145065,3.10536284424954));
#33710=CARTESIAN_POINT('Ctrl Pts',(173.058,1.09198272382463,3.1327977355338));
#33711=CARTESIAN_POINT('Ctrl Pts',(173.058,1.03107802904275,3.15852895038418));
#33712=CARTESIAN_POINT('Ctrl Pts',(173.058,1.0114596465522,3.1668173888484));
#33713=CARTESIAN_POINT('Ctrl Pts',(173.058,0.991755702241084,3.17492900566073));
#33714=CARTESIAN_POINT('Ctrl Pts',(173.058,0.971968657952046,3.18286212972466));
#33715=CARTESIAN_POINT('Ctrl Pts',(173.058,0.956867573602449,3.18891653451071));
#33716=CARTESIAN_POINT('Ctrl Pts',(173.058,0.94172575171078,3.1948638770094));
#33717=CARTESIAN_POINT('Ctrl Pts',(173.058,0.926549215256223,3.20070193666412));
#33718=CARTESIAN_POINT('Ctrl Pts',(173.058,0.822753641283176,3.24062967344152));
#33719=CARTESIAN_POINT('Ctrl Pts',(173.058,0.717267605953907,3.27547679138173));
#33720=CARTESIAN_POINT('Ctrl Pts',(173.058,0.610497881757582,3.3051135063329));
#33721=CARTESIAN_POINT('Ctrl Pts',(173.058,0.503660205739328,3.33476908308026));
#33722=CARTESIAN_POINT('Ctrl Pts',(173.058,0.395536406906948,3.35920812012469));
#33723=CARTESIAN_POINT('Ctrl Pts',(173.058,0.286502176775991,3.37825926969399));
#33724=CARTESIAN_POINT('Ctrl Pts',(173.058,0.17972562081492,3.3969159441683));
#33725=CARTESIAN_POINT('Ctrl Pts',(173.058,0.072075126876207,3.41040586117002));
#33726=CARTESIAN_POINT('Ctrl Pts',(173.058,-0.0361149137713203,3.41852273121879));
#33727=CARTESIAN_POINT('Ctrl Pts',(173.058,-0.129418258192251,3.42552273895746));
#33728=CARTESIAN_POINT('Ctrl Pts',(173.058,-0.223123452753258,3.42852607773628));
#33729=CARTESIAN_POINT('Ctrl Pts',(173.058,-0.317020535431506,3.42736954239176));
#33730=CARTESIAN_POINT('',(173.058,-3.44200000000001,-4.2152342826652E-16));
#33731=CARTESIAN_POINT('Origin',(173.058,0.,0.));
#33732=CARTESIAN_POINT('',(173.058,-2.9035416885497,1.85819928779561));
#33733=CARTESIAN_POINT('Origin',(173.058,0.,0.));
#33734=CARTESIAN_POINT('Ctrl Pts',(173.058,-2.90354168854955,1.85819928779586));
#33735=CARTESIAN_POINT('Ctrl Pts',(173.058,-2.94927698134181,1.77348528868279));
#33736=CARTESIAN_POINT('Ctrl Pts',(173.058,-2.99114946863433,1.68689959241407));
#33737=CARTESIAN_POINT('Ctrl Pts',(173.058,-3.02892190972098,1.59857426255952));
#33738=CARTESIAN_POINT('Ctrl Pts',(173.058,-3.07225686000619,1.4972418183738));
#33739=CARTESIAN_POINT('Ctrl Pts',(173.058,-3.11019621799762,1.39361911367756));
#33740=CARTESIAN_POINT('Ctrl Pts',(173.058,-3.1427908688464,1.28813764211491));
#33741=CARTESIAN_POINT('Ctrl Pts',(173.058,-3.16081628017585,1.22980454563925));
#33742=CARTESIAN_POINT('Ctrl Pts',(173.058,-3.17720619857394,1.17090282854363));
#33743=CARTESIAN_POINT('Ctrl Pts',(173.058,-3.19196248863544,1.1115053227446));
#33744=CARTESIAN_POINT('Ctrl Pts',(173.058,-3.19769929159171,1.08841335413712));
#33745=CARTESIAN_POINT('Ctrl Pts',(173.058,-3.2031891341079,1.06524645577256));
#33746=CARTESIAN_POINT('Ctrl Pts',(173.058,-3.20843193488223,1.04200893503998));
#33747=CARTESIAN_POINT('Ctrl Pts',(173.058,-3.21256128773105,1.0237065187234));
#33748=CARTESIAN_POINT('Ctrl Pts',(173.058,-3.21653710764215,1.00536119930646));
#33749=CARTESIAN_POINT('Ctrl Pts',(173.058,-3.22035696748742,0.986987648751191));
#33750=CARTESIAN_POINT('Ctrl Pts',(173.058,-3.24273618152464,0.879343484526355));
#33751=CARTESIAN_POINT('Ctrl Pts',(173.058,-3.25979279126121,0.7706167253394));
#33752=CARTESIAN_POINT('Ctrl Pts',(173.058,-3.27158446109908,0.661236741394953));
#33753=CARTESIAN_POINT('Ctrl Pts',(173.058,-3.2818639471905,0.565883832171975));
#33754=CARTESIAN_POINT('Ctrl Pts',(173.058,-3.2881413770772,0.470033964546229));
#33755=CARTESIAN_POINT('Ctrl Pts',(173.058,-3.29042275668324,0.373974651407001));
#33756=CARTESIAN_POINT('Ctrl Pts',(173.058,-3.29142086026088,0.331948701908589));
#33757=CARTESIAN_POINT('Ctrl Pts',(173.058,-3.29165371669549,0.289882748038347));
#33758=CARTESIAN_POINT('Ctrl Pts',(173.058,-3.29112009188747,0.247801422509378));
#33759=CARTESIAN_POINT('Ctrl Pts',(173.058,-3.29076373357566,0.219699224300322));
#33760=CARTESIAN_POINT('Ctrl Pts',(173.058,-3.29006552909826,0.191590178903719));
#33761=CARTESIAN_POINT('Ctrl Pts',(173.058,-3.2890248546268,0.163481743603303));
#33762=CARTESIAN_POINT('Ctrl Pts',(173.058,-3.28844078257146,0.147706059632424));
#33763=CARTESIAN_POINT('Ctrl Pts',(173.058,-3.28774893091277,0.131934287123879));
#33764=CARTESIAN_POINT('Ctrl Pts',(173.058,-3.28694984088798,0.116175937424863));
#33765=CARTESIAN_POINT('Ctrl Pts',(173.058,-3.28147503817363,0.00821081080604001));
#33766=CARTESIAN_POINT('Ctrl Pts',(173.058,-3.27096658134644,-0.0992403578637111));
#33767=CARTESIAN_POINT('Ctrl Pts',(173.058,-3.25547394530537,-0.205775224611218));
#33768=CARTESIAN_POINT('Ctrl Pts',(173.058,-3.24008355632353,-0.311606991072829));
#33769=CARTESIAN_POINT('Ctrl Pts',(173.058,-3.21977431584416,-0.416535404155237));
#33770=CARTESIAN_POINT('Ctrl Pts',(173.058,-3.19454570367412,-0.520151630293488));
#33771=CARTESIAN_POINT('Ctrl Pts',(173.058,-3.17007291782756,-0.620663608337271));
#33772=CARTESIAN_POINT('Ctrl Pts',(173.058,-3.14097073517173,-0.719941511152529));
#33773=CARTESIAN_POINT('Ctrl Pts',(173.058,-3.1071971623692,-0.817587324307012));
#33774=CARTESIAN_POINT('Ctrl Pts',(173.058,-3.08548206143738,-0.880369805172085));
#33775=CARTESIAN_POINT('Ctrl Pts',(173.058,-3.06183499229822,-0.942477053141852));
#33776=CARTESIAN_POINT('Ctrl Pts',(173.058,-3.03623629418228,-1.00379570569807));
#33777=CARTESIAN_POINT('Ctrl Pts',(173.058,-3.02812773113467,-1.02321880909165));
#33778=CARTESIAN_POINT('Ctrl Pts',(173.058,-3.01982330277573,-1.04256273766869));
#33779=CARTESIAN_POINT('Ctrl Pts',(173.058,-3.01132224969803,-1.06182373964142));
#33780=CARTESIAN_POINT('Ctrl Pts',(173.058,-3.00479372173366,-1.076615552944));
#33781=CARTESIAN_POINT('Ctrl Pts',(173.058,-2.99815215727783,-1.0913517307087));
#33782=CARTESIAN_POINT('Ctrl Pts',(173.058,-2.99140048475794,-1.10602445977451));
#33783=CARTESIAN_POINT('Ctrl Pts',(173.058,-2.94870774535495,-1.19880428529069));
#33784=CARTESIAN_POINT('Ctrl Pts',(173.058,-2.90158057124625,-1.28912974556565));
#33785=CARTESIAN_POINT('Ctrl Pts',(173.058,-2.8500188206114,-1.37663588218576));
#33786=CARTESIAN_POINT('Ctrl Pts',(173.058,-2.81978995482352,-1.42793769461331));
#33787=CARTESIAN_POINT('Ctrl Pts',(173.058,-2.78803607036402,-1.47827002836663));
#33788=CARTESIAN_POINT('Ctrl Pts',(173.058,-2.75475040343885,-1.52755433789291));
#33789=CARTESIAN_POINT('Ctrl Pts',(173.058,-2.69695413048116,-1.61313019287923));
#33790=CARTESIAN_POINT('Ctrl Pts',(173.058,-2.63454105743263,-1.69554864285166));
#33791=CARTESIAN_POINT('Ctrl Pts',(173.058,-2.56786860476729,-1.77461959696379));
#33792=CARTESIAN_POINT('Ctrl Pts',(173.058,-2.50091177594761,-1.85402781021296));
#33793=CARTESIAN_POINT('Ctrl Pts',(173.058,-2.42965826721123,-1.93006033993478));
#33794=CARTESIAN_POINT('Ctrl Pts',(173.058,-2.35444524775537,-2.00247889412283));
#33795=CARTESIAN_POINT('Ctrl Pts',(173.058,-2.34043558406068,-2.01596804263422));
#33796=CARTESIAN_POINT('Ctrl Pts',(173.058,-2.32628849698641,-2.02933166582729));
#33797=CARTESIAN_POINT('Ctrl Pts',(173.058,-2.31200610941859,-2.04256803058097));
#33798=CARTESIAN_POINT('Ctrl Pts',(173.058,-2.30065881337112,-2.05308426596102));
#33799=CARTESIAN_POINT('Ctrl Pts',(173.058,-2.28923218286527,-2.06351451415364));
#33800=CARTESIAN_POINT('Ctrl Pts',(173.058,-2.27773101546705,-2.07385511502059));
#33801=CARTESIAN_POINT('Ctrl Pts',(173.058,-2.20204585166299,-2.14190299601807));
#33802=CARTESIAN_POINT('Ctrl Pts',(173.058,-2.12308768631656,-2.20611658225596));
#33803=CARTESIAN_POINT('Ctrl Pts',(173.058,-2.04121912336534,-2.26634216288826));
#33804=CARTESIAN_POINT('Ctrl Pts',(173.058,-1.95923481267905,-2.32665289188886));
#33805=CARTESIAN_POINT('Ctrl Pts',(173.058,-1.87433096669665,-2.38296469657146));
#33806=CARTESIAN_POINT('Ctrl Pts',(173.058,-1.7868466424218,-2.43507739372807));
#33807=CARTESIAN_POINT('Ctrl Pts',(173.058,-1.70047530653565,-2.48652710551765));
#33808=CARTESIAN_POINT('Ctrl Pts',(173.058,-1.61158786513365,-2.53388410814607));
#33809=CARTESIAN_POINT('Ctrl Pts',(173.058,-1.52049938149984,-2.57690684306378));
#33810=CARTESIAN_POINT('Ctrl Pts',(173.058,-1.46934261688622,-2.60106910634249));
#33811=CARTESIAN_POINT('Ctrl Pts',(173.058,-1.41749148596287,-2.62386338352615));
#33812=CARTESIAN_POINT('Ctrl Pts',(173.058,-1.36500174485935,-2.64523955756217));
#33813=CARTESIAN_POINT('Ctrl Pts',(173.058,-1.35022593925688,-2.65125692753658));
#33814=CARTESIAN_POINT('Ctrl Pts',(173.058,-1.33539953217638,-2.65716189129253));
#33815=CARTESIAN_POINT('Ctrl Pts',(173.058,-1.32052377671622,-2.66295325147544));
#33816=CARTESIAN_POINT('Ctrl Pts',(173.058,-1.30634201517583,-2.66847442916141));
#33817=CARTESIAN_POINT('Ctrl Pts',(173.058,-1.29212315263705,-2.67388931397687));
#33818=CARTESIAN_POINT('Ctrl Pts',(173.058,-1.27787268843006,-2.67919566395992));
#33819=CARTESIAN_POINT('Ctrl Pts',(173.058,-1.18535651693264,-2.71364529155983));
#33820=CARTESIAN_POINT('Ctrl Pts',(173.058,-1.09145092288641,-2.74354721992335));
#33821=CARTESIAN_POINT('Ctrl Pts',(173.058,-0.996467560098021,-2.76872192402909));
#33822=CARTESIAN_POINT('Ctrl Pts',(173.058,-0.902843142461929,-2.79353644882447));
#33823=CARTESIAN_POINT('Ctrl Pts',(173.058,-0.808170782502429,-2.81375820684046));
#33824=CARTESIAN_POINT('Ctrl Pts',(173.058,-0.71274438433838,-2.82916570405975));
#33825=CARTESIAN_POINT('Ctrl Pts',(173.058,-0.620307640495166,-2.84409049322842));
#33826=CARTESIAN_POINT('Ctrl Pts',(173.058,-0.527162731451988,-2.85449793884808));
#33827=CARTESIAN_POINT('Ctrl Pts',(173.058,-0.433582809923952,-2.86013906025488));
#33828=CARTESIAN_POINT('Ctrl Pts',(173.058,-0.358936314546988,-2.86463884969835));
#33829=CARTESIAN_POINT('Ctrl Pts',(173.058,-0.284013023602468,-2.86610502511712));
#33830=CARTESIAN_POINT('Ctrl Pts',(173.058,-0.208958374082637,-2.86438831129802));
#33831=CARTESIAN_POINT('Ctrl Pts',(156.641910346562,-1.26059492705642,2.58055893749389));
#33832=CARTESIAN_POINT('Ctrl Pts',(156.694526018528,-2.1137122723725,2.16381379671687));
#33833=CARTESIAN_POINT('Ctrl Pts',(156.79975736246,-3.35978581135109,0.42459068590928));
#33834=CARTESIAN_POINT('Ctrl Pts',(156.957604378359,-2.19296763671057,-2.58504463930359));
#33835=CARTESIAN_POINT('Ctrl Pts',(157.115451394257,0.963301600147334,-3.24751306779502));
#33836=CARTESIAN_POINT('Ctrl Pts',(157.273298410156,3.24548551852033,-0.972003967714269));
#33837=CARTESIAN_POINT('Ctrl Pts',(157.431145426054,2.58940221207372,2.18521955033239));
#33838=CARTESIAN_POINT('Ctrl Pts',(157.588992441952,-0.412068725742385,
3.36277947991426));
#33839=CARTESIAN_POINT('Ctrl Pts',(157.746839457851,-3.04016140279596,1.49535934622665));
#33840=CARTESIAN_POINT('Ctrl Pts',(157.904686473749,-2.91518172767359,-1.72643828285233));
#33841=CARTESIAN_POINT('Ctrl Pts',(158.062533489648,-0.150157556215628,
-3.38468261701631));
#33842=CARTESIAN_POINT('Ctrl Pts',(158.220380505546,2.7508243349508,-1.97779608453694));
#33843=CARTESIAN_POINT('Ctrl Pts',(158.378227521445,3.1606675065917,1.2202074592191));
#33844=CARTESIAN_POINT('Ctrl Pts',(158.536074537343,0.708198630334437,3.31317840661986));
#33845=CARTESIAN_POINT('Ctrl Pts',(158.693921553242,-2.38561307487835,2.40573461840344));
#33846=CARTESIAN_POINT('Ctrl Pts',(158.85176856914,-3.31901103198709,-0.68034914075078));
#33847=CARTESIAN_POINT('Ctrl Pts',(159.009615585039,-1.24670620219767,-3.15030627040552));
#33848=CARTESIAN_POINT('Ctrl Pts',(159.167462600937,1.95461751556788,-2.76734131891007));
#33849=CARTESIAN_POINT('Ctrl Pts',(159.325309616835,3.38583646824711,0.121732956096346));
#33850=CARTESIAN_POINT('Ctrl Pts',(159.483156632734,1.75083606284643,2.90056550260836));
#33851=CARTESIAN_POINT('Ctrl Pts',(159.641003648632,-1.46972441564107,3.05264107133596));
#33852=CARTESIAN_POINT('Ctrl Pts',(159.798850664531,-3.35929998446003,0.440239652832843));
#33853=CARTESIAN_POINT('Ctrl Pts',(159.956697680429,-2.20668775975965,-2.57084352550351));
#33854=CARTESIAN_POINT('Ctrl Pts',(160.114544696328,0.944304649918255,-3.25376644164669));
#33855=CARTESIAN_POINT('Ctrl Pts',(160.272391712226,3.24013316437363,-0.99007292658079));
#33856=CARTESIAN_POINT('Ctrl Pts',(160.430238728125,2.6016915700248,2.17023231333377));
#33857=CARTESIAN_POINT('Ctrl Pts',(160.588085744023,-0.392846336843677,
3.36517147828997));
#33858=CARTESIAN_POINT('Ctrl Pts',(160.745932759922,-3.03162193287603,1.51260562534786));
#33859=CARTESIAN_POINT('Ctrl Pts',(160.90377977582,-2.92495554734722,-1.70977845567023));
#33860=CARTESIAN_POINT('Ctrl Pts',(161.061626791718,-0.169444440750171,
-3.38378425779796));
#33861=CARTESIAN_POINT('Ctrl Pts',(161.219473807617,2.73951583977761,-1.99342927772498));
#33862=CARTESIAN_POINT('Ctrl Pts',(161.377320823515,3.16756591388022,1.2021786484908));
#33863=CARTESIAN_POINT('Ctrl Pts',(161.535167839414,0.727062906055984,3.30909154487233));
#33864=CARTESIAN_POINT('Ctrl Pts',(161.693014855312,-2.37186950675857,2.41928550704491));
#33865=CARTESIAN_POINT('Ctrl Pts',(161.850861871211,-3.32283285798019,-0.661429602917294));
#33866=CARTESIAN_POINT('Ctrl Pts',(162.008708887109,-1.26463311846787,-3.14315293890823));
#33867=CARTESIAN_POINT('Ctrl Pts',(162.166555903007,1.93882052518752,-2.77843162464046));
#33868=CARTESIAN_POINT('Ctrl Pts',(162.324402918906,3.38647500189316,0.102442097028211));
#33869=CARTESIAN_POINT('Ctrl Pts',(162.482249934804,1.76733195403479,2.89054408130007));
#33870=CARTESIAN_POINT('Ctrl Pts',(162.640096950703,-1.4523099189108,3.0609644266349));
#33871=CARTESIAN_POINT('Ctrl Pts',(162.797943966601,-3.3567374578584,0.459370178289061));
#33872=CARTESIAN_POINT('Ctrl Pts',(162.9557909825,-2.2212978427249,-2.55823048523718));
#33873=CARTESIAN_POINT('Ctrl Pts',(163.113637998398,0.925752878818704,-3.25909326792743));
#33874=CARTESIAN_POINT('Ctrl Pts',(163.271485014297,3.23444021792712,-1.00851564110162));
#33875=CARTESIAN_POINT('Ctrl Pts',(163.429332030195,2.61401299155246,2.15537546652226));
#33876=CARTESIAN_POINT('Ctrl Pts',(163.587179046093,-0.37366884830378,3.36735488380693));
#33877=CARTESIAN_POINT('Ctrl Pts',(163.745026061992,-3.02295554325443,1.52985198800354));
#33878=CARTESIAN_POINT('Ctrl Pts',(163.90287307789,-2.93464855399438,-1.69308747152348));
#33879=CARTESIAN_POINT('Ctrl Pts',(164.060720093789,-0.188718840271762,
-3.38276403566928));
#33880=CARTESIAN_POINT('Ctrl Pts',(164.218567109687,2.72811497634857,-2.00900373257834));
#33881=CARTESIAN_POINT('Ctrl Pts',(164.376414125585,3.17436322788575,1.18411376950773));
#33882=CARTESIAN_POINT('Ctrl Pts',(164.534261141484,0.74590273835584,3.30489582689142));
#33883=CARTESIAN_POINT('Ctrl Pts',(164.692108157382,-2.35804854035057,2.43275859941788));
#33884=CARTESIAN_POINT('Ctrl Pts',(164.849955173281,-3.32654704816499,-0.642488955575008));
#33885=CARTESIAN_POINT('Ctrl Pts',(165.007802189179,-1.28251888829241,-3.13589741905954));
#33886=CARTESIAN_POINT('Ctrl Pts',(165.165649205078,1.92296055931244,-2.78943184340823));
#33887=CARTESIAN_POINT('Ctrl Pts',(165.323496220976,3.38700365205358,0.0831479564798997));
#33888=CARTESIAN_POINT('Ctrl Pts',(165.481343236875,1.78377047374568,2.88042882548487));
#33889=CARTESIAN_POINT('Ctrl Pts',(165.639190252773,-1.43484828107338,3.06918844843256));
#33890=CARTESIAN_POINT('Ctrl Pts',(165.797037268672,-3.35406599083499,0.478485789564522));
#33891=CARTESIAN_POINT('Ctrl Pts',(165.95488428457,-2.23583583159796,-2.54553441458444));
#33892=CARTESIAN_POINT('Ctrl Pts',(166.112731300469,0.90717106151226,-3.26431432108579));
#33893=CARTESIAN_POINT('Ctrl Pts',(166.270578316367,3.22864229756116,-1.02692562344606));
#33894=CARTESIAN_POINT('Ctrl Pts',(166.428425332265,2.62624957467685,2.14044866633159));
#33895=CARTESIAN_POINT('Ctrl Pts',(166.586272348164,-0.354479232189763,
3.36942900142401));
#33896=CARTESIAN_POINT('Ctrl Pts',(166.744119364062,-3.01419104315912,1.54704869898476));
#33897=CARTESIAN_POINT('Ctrl Pts',(166.901966379961,-2.94424631611884,-1.67634153790678));
#33898=CARTESIAN_POINT('Ctrl Pts',(167.059813395859,-0.207987114903346,
-3.38163402539736));
#33899=CARTESIAN_POINT('Ctrl Pts',(167.217660411758,2.71662557150557,-2.02451298487645));
#33900=CARTESIAN_POINT('Ctrl Pts',(167.375507427656,3.18105751740887,1.16601045991334));
#33901=CARTESIAN_POINT('Ctrl Pts',(167.533354443555,0.764718362261322,3.3005928479761));
#33902=CARTESIAN_POINT('Ctrl Pts',(167.691201459453,-2.34415104309101,2.44615273621018));
#33903=CARTESIAN_POINT('Ctrl Pts',(167.849048475351,-3.33015327471841,-0.623527456148029));
#33904=CARTESIAN_POINT('Ctrl Pts',(168.00689549125,-1.30036303375706,-3.12854012314479));
#33905=CARTESIAN_POINT('Ctrl Pts',(168.164742507148,1.90703818343888,-2.80034153070911));
#33906=CARTESIAN_POINT('Ctrl Pts',(168.322589523047,3.38742237645021,0.0638511173542441));
#33907=CARTESIAN_POINT('Ctrl Pts',(168.480436538945,1.80015110090155,2.87022008487266));
#33908=CARTESIAN_POINT('Ctrl Pts',(168.638283554844,-1.41734007501666,3.07731285922868));
#33909=CARTESIAN_POINT('Ctrl Pts',(168.796130570742,-3.3512856670145,0.497585871478016));
#33910=CARTESIAN_POINT('Ctrl Pts',(168.953977586641,-2.25030125612222,-2.53275572813956));
#33911=CARTESIAN_POINT('Ctrl Pts',(169.111824602539,0.888559801961863,-3.26942943049782));
#33912=CARTESIAN_POINT('Ctrl Pts',(169.269671618437,3.2227395907929,-1.04530227652681));
#33913=CARTESIAN_POINT('Ctrl Pts',(169.427518634336,2.63840092301917,2.12545239707543));
#33914=CARTESIAN_POINT('Ctrl Pts',(169.585365650234,-0.335278112564125,
3.37139376458444));
#33915=CARTESIAN_POINT('Ctrl Pts',(169.743212666133,-3.00532871463423,1.564195198398));
#33916=CARTESIAN_POINT('Ctrl Pts',(169.901059682031,-2.95374852702394,-1.65954119461478));
#33917=CARTESIAN_POINT('Ctrl Pts',(170.05890669793,-0.227248629623084,-3.38039427118688));
#33918=CARTESIAN_POINT('Ctrl Pts',(170.216753713828,2.7050479786207,-2.03995651601825));
#33919=CARTESIAN_POINT('Ctrl Pts',(170.374600729726,3.18764860462061,1.14786927643015));
#33920=CARTESIAN_POINT('Ctrl Pts',(170.532447745625,0.783509087420058,3.2961828100762));
#33921=CARTESIAN_POINT('Ctrl Pts',(170.690294761523,-2.33017730499065,2.45946735681956));
#33922=CARTESIAN_POINT('Ctrl Pts',(170.848141777422,-3.33365174602366,-0.604545465623319));
#33923=CARTESIAN_POINT('Ctrl Pts',(171.00598879332,-1.31816431809934,-3.12108180407131));
#33924=CARTESIAN_POINT('Ctrl Pts',(171.163835809219,1.89105258537231,-2.81115929350443));
#33925=CARTESIAN_POINT('Ctrl Pts',(171.321682825117,3.38773384709925,0.04455010635921));
#33926=CARTESIAN_POINT('Ctrl Pts',(171.479529841016,1.81646787669691,2.85992243368512));
#33927=CARTESIAN_POINT('Ctrl Pts',(171.637376856914,-1.39977490155201,3.08532882114793));
#33928=CARTESIAN_POINT('Ctrl Pts',(171.795223872812,-3.34841873999253,0.516687131179943));
#33929=CARTESIAN_POINT('Ctrl Pts',(171.953070888711,-2.26464885829485,-2.51992985577406));
#33930=CARTESIAN_POINT('Ctrl Pts',(172.110917904609,0.869829193827587,-3.27436767007504));
#33931=CARTESIAN_POINT('Ctrl Pts',(172.268764920508,3.21691519730582,-1.0637880016197));
#33932=CARTESIAN_POINT('Ctrl Pts',(172.426611936406,2.65009699317679,2.11067616912988));
#33933=CARTESIAN_POINT('Ctrl Pts',(172.584458952305,-0.315318796737369,
3.37266439996185));
#33934=CARTESIAN_POINT('Ctrl Pts',(172.742305968203,-2.9978837177994,1.58248414128088));
#33935=CARTESIAN_POINT('Ctrl Pts',(172.900152984102,-2.96002690825633,-1.64519866615417));
#33936=CARTESIAN_POINT('Ctrl Pts',(173.005384328034,-1.15590801223433,-2.79530792301902));
#33937=CARTESIAN_POINT('Ctrl Pts',(173.058,-0.208958374082637,-2.86438831129802));
#33938=CARTESIAN_POINT('Ctrl Pts',(156.751606897708,-1.34399083100512,2.75127836581));
#33939=CARTESIAN_POINT('Ctrl Pts',(156.804222569674,-2.25354699791245,2.30696303814315));
#33940=CARTESIAN_POINT('Ctrl Pts',(156.909453913606,-3.58205576405188,0.452679902595504));
#33941=CARTESIAN_POINT('Ctrl Pts',(157.067300929505,-2.33804557925064,-2.75606082365862));
#33942=CARTESIAN_POINT('Ctrl Pts',(157.225147945403,1.02702977007349,-3.46235550612409));
#33943=CARTESIAN_POINT('Ctrl Pts',(157.382994961302,3.46019382232215,-1.03630785137227));
#33944=CARTESIAN_POINT('Ctrl Pts',(157.5408419772,2.76070667596441,2.32978491055631));
#33945=CARTESIAN_POINT('Ctrl Pts',(157.698688993099,-0.439329539771279,
3.58524748171918));
#33946=CARTESIAN_POINT('Ctrl Pts',(157.856536008997,-3.24128628668565,1.59428632247425));
#33947=CARTESIAN_POINT('Ctrl Pts',(158.014383024895,-3.10803845756845,-1.84065251465661));
#33948=CARTESIAN_POINT('Ctrl Pts',(158.172230040794,-0.160091377831587,
-3.6085996425153));
#33949=CARTESIAN_POINT('Ctrl Pts',(158.330077056692,2.93280783900394,-2.10863914026887));
#33950=CARTESIAN_POINT('Ctrl Pts',(158.487924072591,3.36976459094144,1.30093149029555));
#33951=CARTESIAN_POINT('Ctrl Pts',(158.645771088489,0.755050211032075,3.53236500037256));
#33952=CARTESIAN_POINT('Ctrl Pts',(158.803618104388,-2.54343566687934,2.56488837101372));
#33953=CARTESIAN_POINT('Ctrl Pts',(158.961465120286,-3.5385834888386,-0.725358310925775));
#33954=CARTESIAN_POINT('Ctrl Pts',(159.119312136185,-1.3291832838194,-3.35871789692955));
#33955=CARTESIAN_POINT('Ctrl Pts',(159.277159152083,2.0839271701493,-2.95041752037001));
#33956=CARTESIAN_POINT('Ctrl Pts',(159.435006167982,3.60982982791527,0.129786320183477));
#33957=CARTESIAN_POINT('Ctrl Pts',(159.59285318388,1.86666435391219,3.09245528168063));
#33958=CARTESIAN_POINT('Ctrl Pts',(159.750700199778,-1.56695548770644,3.25459156003856));
#33959=CARTESIAN_POINT('Ctrl Pts',(159.908547215677,-3.58153779680244,0.4693641424005));
#33960=CARTESIAN_POINT('Ctrl Pts',(160.066394231575,-2.35267337060728,-2.74092022113221));
#33961=CARTESIAN_POINT('Ctrl Pts',(160.224241247474,1.00677605781672,-3.46902257810661));
#33962=CARTESIAN_POINT('Ctrl Pts',(160.382088263372,3.45448737789416,-1.05557218008024));
#33963=CARTESIAN_POINT('Ctrl Pts',(160.539935279271,2.77380904854317,2.3138061780738));
#33964=CARTESIAN_POINT('Ctrl Pts',(160.697782295169,-0.418835474726765,
3.58779772511277));
#33965=CARTESIAN_POINT('Ctrl Pts',(160.855629311068,-3.23218187968885,1.61267354624485));
#33966=CARTESIAN_POINT('Ctrl Pts',(161.013476326966,-3.1184588739475,-1.82289054013307));
#33967=CARTESIAN_POINT('Ctrl Pts',(161.171323342865,-0.180654205284504,
-3.60764185145451));
#33968=CARTESIAN_POINT('Ctrl Pts',(161.329170358763,2.92075121915007,-2.12530656281126));
#33969=CARTESIAN_POINT('Ctrl Pts',(161.487017374661,3.37711936918567,1.28170996576558));
#33970=CARTESIAN_POINT('Ctrl Pts',(161.64486439056,0.77516247156807,3.5280077682448));
#33971=CARTESIAN_POINT('Ctrl Pts',(161.802711406458,-2.52878287942016,2.57933573209316));
#33972=CARTESIAN_POINT('Ctrl Pts',(161.960558422357,-3.54265815150952,-0.705187132358178));
#33973=CARTESIAN_POINT('Ctrl Pts',(162.118405438255,-1.34829617296264,-3.35109132971343));
#33974=CARTESIAN_POINT('Ctrl Pts',(162.276252454154,2.06708511424935,-2.96224151624273));
#33975=CARTESIAN_POINT('Ctrl Pts',(162.434099470052,3.61051060438609,0.109219255257768));
#33976=CARTESIAN_POINT('Ctrl Pts',(162.59194648595,1.88425154709422,3.08177088333593));
#33977=CARTESIAN_POINT('Ctrl Pts',(162.749793501849,-1.54838891772451,3.26346555513791));
#33978=CARTESIAN_POINT('Ctrl Pts',(162.907640517747,-3.57880574371951,0.489760266685644));
#33979=CARTESIAN_POINT('Ctrl Pts',(163.065487533646,-2.36824999805838,-2.72747275271455));
#33980=CARTESIAN_POINT('Ctrl Pts',(163.223334549544,0.986996975955014,-3.47470180584743));
#33981=CARTESIAN_POINT('Ctrl Pts',(163.381181565443,3.44841780894597,-1.07523499061742));
#33982=CARTESIAN_POINT('Ctrl Pts',(163.539028581341,2.78694560589613,2.29796646187016));
#33983=CARTESIAN_POINT('Ctrl Pts',(163.69687559724,-0.398389280468699,3.59012557598079));
#33984=CARTESIAN_POINT('Ctrl Pts',(163.854722613138,-3.222942156492,1.63106085907622));
#33985=CARTESIAN_POINT('Ctrl Pts',(164.012569629037,-3.12879313103441,-1.80509534742508));
#33986=CARTESIAN_POINT('Ctrl Pts',(164.170416644935,-0.201203721766088,
-3.60655413552205));
#33987=CARTESIAN_POINT('Ctrl Pts',(164.328263660833,2.90859612032705,-2.14191136112637));
#33988=CARTESIAN_POINT('Ctrl Pts',(164.486110676732,3.38436636622082,1.26244998684979));
#33989=CARTESIAN_POINT('Ctrl Pts',(164.64395769263,0.795248671603639,3.52353447839189));
#33990=CARTESIAN_POINT('Ctrl Pts',(164.801804708528,-2.51404757331246,2.59370015021503));
#33991=CARTESIAN_POINT('Ctrl Pts',(164.959651724427,-3.54661805761881,-0.68499344776135));
#33992=CARTESIAN_POINT('Ctrl Pts',(165.117498740325,-1.3673651935764,-3.34335581377447));
#33993=CARTESIAN_POINT('Ctrl Pts',(165.275345756224,2.05017591664855,-2.97396946536074));
#33994=CARTESIAN_POINT('Ctrl Pts',(165.433192772122,3.61107422792063,0.0886486917623198));
#33995=CARTESIAN_POINT('Ctrl Pts',(165.591039788021,1.90177757333195,3.07098644276972));
#33996=CARTESIAN_POINT('Ctrl Pts',(165.748886803919,-1.52977208796888,3.27223364522999));
#33997=CARTESIAN_POINT('Ctrl Pts',(165.906733819818,-3.57595754315345,0.510140490127658));
#33998=CARTESIAN_POINT('Ctrl Pts',(166.064580835716,-2.38374976196135,-2.71393676095317));
#33999=CARTESIAN_POINT('Ctrl Pts',(166.222427851615,0.967185860149888,-3.48026826294036));
#34000=CARTESIAN_POINT('Ctrl Pts',(166.380274867513,3.44223632142488,-1.09486290354871));
#34001=CARTESIAN_POINT('Ctrl Pts',(166.538121883411,2.79999171227736,2.2820521644524));
#34002=CARTESIAN_POINT('Ctrl Pts',(166.69596889931,-0.377930156324856,3.59233690889983));
#34003=CARTESIAN_POINT('Ctrl Pts',(166.853815915208,-3.21359783222604,1.64939523547751));
#34004=CARTESIAN_POINT('Ctrl Pts',(167.011662931107,-3.13902584260304,-1.78724157001062));
#34005=CARTESIAN_POINT('Ctrl Pts',(167.169509947005,-0.22174670815951,-3.60534936830317));
#34006=CARTESIAN_POINT('Ctrl Pts',(167.327356962904,2.89634662254527,-2.15844664334671));
#34007=CARTESIAN_POINT('Ctrl Pts',(167.485203978802,3.39150352308704,1.24314903490759));
#34008=CARTESIAN_POINT('Ctrl Pts',(167.643050994701,0.815309061714566,3.51894683165139));
#34009=CARTESIAN_POINT('Ctrl Pts',(167.800898010599,-2.49923067337904,2.60798038937174));
#34010=CARTESIAN_POINT('Ctrl Pts',(167.958745026497,-3.55046285765591,-0.664777531589554));
#34011=CARTESIAN_POINT('Ctrl Pts',(168.116592042396,-1.38638983612959,-3.33551178867316));
#34012=CARTESIAN_POINT('Ctrl Pts',(168.274439058294,2.03320018025411,-2.98560089381315));
#34013=CARTESIAN_POINT('Ctrl Pts',(168.432286074193,3.61152065344378,0.0680752511624752));
#34014=CARTESIAN_POINT('Ctrl Pts',(168.590133090091,1.91924187707542,3.06010233282732));
#34015=CARTESIAN_POINT('Ctrl Pts',(168.74798010599,-1.51110560922735,3.28089553445622));
#34016=CARTESIAN_POINT('Ctrl Pts',(168.905827121888,-3.57299328426128,0.530504156847406));
#34017=CARTESIAN_POINT('Ctrl Pts',(169.063674137786,-2.39917216094927,-2.70031268787022));
#34018=CARTESIAN_POINT('Ctrl Pts',(169.221521153685,0.947343354320042,-3.48572176747365));
#34019=CARTESIAN_POINT('Ctrl Pts',(169.379368169583,3.43594311525342,-1.11445528228592));
#34020=CARTESIAN_POINT('Ctrl Pts',(169.537215185482,2.81294694508522,2.26606380217442));
#34021=CARTESIAN_POINT('Ctrl Pts',(169.69506220138,-0.357458767643203,3.59443165291001));
#34022=CARTESIAN_POINT('Ctrl Pts',(169.852909217279,-3.204149207594,1.66767607851488));
#34023=CARTESIAN_POINT('Ctrl Pts',(170.010756233177,-3.1491566816669,-1.76932978339498));
#34024=CARTESIAN_POINT('Ctrl Pts',(170.168603249076,-0.242282487432436,
-3.60402759692696));
#34025=CARTESIAN_POINT('Ctrl Pts',(170.326450264974,2.8840031025545,-2.17491185656266));
#34026=CARTESIAN_POINT('Ctrl Pts',(170.484297280873,3.39853065019093,1.22380770349201));
#34027=CARTESIAN_POINT('Ctrl Pts',(170.642144296771,0.835342905877536,3.51424504333333));
#34028=CARTESIAN_POINT('Ctrl Pts',(170.79999131267,-2.48433248881662,2.62217585187379));
#34029=CARTESIAN_POINT('Ctrl Pts',(170.957838328568,-3.55419277378985,-0.644539768711187));
#34030=CARTESIAN_POINT('Ctrl Pts',(171.115685344466,-1.40536878204047,-3.32756005712616));
#34031=CARTESIAN_POINT('Ctrl Pts',(171.273532360365,2.01615703913996,-2.99713431640342));
#34032=CARTESIAN_POINT('Ctrl Pts',(171.431379376263,3.61185272974161,0.0474973626991037));
#34033=CARTESIAN_POINT('Ctrl Pts',(171.589226392162,1.93663810530849,3.04912343034255));
#34034=CARTESIAN_POINT('Ctrl Pts',(171.74707340806,-1.49237839434269,3.28944180026288));
#34035=CARTESIAN_POINT('Ctrl Pts',(171.904920423959,-3.56993669284718,0.550869079273346));
#34036=CARTESIAN_POINT('Ctrl Pts',(172.062767439857,-2.41446894293137,-2.68663830723542));
#34037=CARTESIAN_POINT('Ctrl Pts',(172.220614455756,0.927373604282732,-3.49098670117333));
#34038=CARTESIAN_POINT('Ctrl Pts',(172.378461471654,3.42973340325571,-1.13416394880208));
#34039=CARTESIAN_POINT('Ctrl Pts',(172.536308487552,2.82541678032987,2.25031003825753));
#34040=CARTESIAN_POINT('Ctrl Pts',(172.694155503451,-0.336179023541002,
3.59578634842729));
#34041=CARTESIAN_POINT('Ctrl Pts',(172.852002519349,-3.19621167963151,1.68717494449934));
#34042=CARTESIAN_POINT('Ctrl Pts',(173.009849535248,-3.15585041541815,-1.75403841078134));
#34043=CARTESIAN_POINT('Ctrl Pts',(173.11508087918,-1.23237824981253,-2.98023428282876));
#34044=CARTESIAN_POINT('Ctrl Pts',(173.167696551146,-0.222782221950241,
-3.05388475250506));
#34045=CARTESIAN_POINT('Ctrl Pts',(156.861303448854,-1.42738673495382,2.92199779412611));
#34046=CARTESIAN_POINT('Ctrl Pts',(156.91391912082,-2.3933817234524,2.45011227956942));
#34047=CARTESIAN_POINT('Ctrl Pts',(157.019150464752,-3.80432571675269,0.480769119281727));
#34048=CARTESIAN_POINT('Ctrl Pts',(157.176997480651,-2.4831235217907,-2.92707700801364));
#34049=CARTESIAN_POINT('Ctrl Pts',(157.334844496549,1.09075793999965,-3.67719794445316));
#34050=CARTESIAN_POINT('Ctrl Pts',(157.492691512448,3.67490212612398,-1.10061173503027));
#34051=CARTESIAN_POINT('Ctrl Pts',(157.650538528346,2.93201113985509,2.47435027078023));
#34052=CARTESIAN_POINT('Ctrl Pts',(157.808385544245,-0.466590353800172,
3.8077154835241));
#34053=CARTESIAN_POINT('Ctrl Pts',(157.966232560143,-3.44241117057535,1.69321329872186));
#34054=CARTESIAN_POINT('Ctrl Pts',(158.124079576041,-3.3008951874633,-1.95486674646089));
#34055=CARTESIAN_POINT('Ctrl Pts',(158.28192659194,-0.17002519944755,-3.83251666801428));
#34056=CARTESIAN_POINT('Ctrl Pts',(158.439773607838,3.11479134305708,-2.23948219600079));
#34057=CARTESIAN_POINT('Ctrl Pts',(158.597620623737,3.57886167529118,1.381655521372));
#34058=CARTESIAN_POINT('Ctrl Pts',(158.755467639635,0.801901791729711,3.75155159412526));
#34059=CARTESIAN_POINT('Ctrl Pts',(158.913314655534,-2.70125825888032,2.72404212362399));
#34060=CARTESIAN_POINT('Ctrl Pts',(159.071161671432,-3.75815594569012,-0.770367481100765));
#34061=CARTESIAN_POINT('Ctrl Pts',(159.229008687331,-1.41166036544114,-3.56712952345359));
#34062=CARTESIAN_POINT('Ctrl Pts',(159.386855703229,2.21323682473072,-3.13349372182995));
#34063=CARTESIAN_POINT('Ctrl Pts',(159.544702719128,3.83382318758342,0.137839684270605));
#34064=CARTESIAN_POINT('Ctrl Pts',(159.702549735026,1.98249264497796,3.2843450607529));
#34065=CARTESIAN_POINT('Ctrl Pts',(159.860396750924,-1.66418655977181,3.45654204874115));
#34066=CARTESIAN_POINT('Ctrl Pts',(160.018243766823,-3.80377560914485,0.498488631968156));
#34067=CARTESIAN_POINT('Ctrl Pts',(160.176090782721,-2.49865898145491,-2.9109969167609));
#34068=CARTESIAN_POINT('Ctrl Pts',(160.33393779862,1.06924746571519,-3.68427871456653));
#34069=CARTESIAN_POINT('Ctrl Pts',(160.491784814518,3.66884159141469,-1.12107143357969));
#34070=CARTESIAN_POINT('Ctrl Pts',(160.649631830417,2.94592652706154,2.45738004281382));
#34071=CARTESIAN_POINT('Ctrl Pts',(160.807478846315,-0.444824612609852,
3.81042397193558));
#34072=CARTESIAN_POINT('Ctrl Pts',(160.965325862214,-3.43274182650167,1.71274146714184));
#34073=CARTESIAN_POINT('Ctrl Pts',(161.123172878112,-3.31196220054779,-1.93600262459591));
#34074=CARTESIAN_POINT('Ctrl Pts',(161.28101989401,-0.191863969818835,-3.83149944511106));
#34075=CARTESIAN_POINT('Ctrl Pts',(161.438866909909,3.10198659852252,-2.25718384789754));
#34076=CARTESIAN_POINT('Ctrl Pts',(161.596713925807,3.58667282449113,1.36124128304037));
#34077=CARTESIAN_POINT('Ctrl Pts',(161.754560941706,0.823262037080152,3.74692399161727));
#34078=CARTESIAN_POINT('Ctrl Pts',(161.912407957604,-2.68569625208175,2.73938595714142));
#34079=CARTESIAN_POINT('Ctrl Pts',(162.070254973503,-3.76248344503886,-0.748944661799061));
#34080=CARTESIAN_POINT('Ctrl Pts',(162.228101989401,-1.4319592274574,-3.55902972051863));
#34081=CARTESIAN_POINT('Ctrl Pts',(162.385949005299,2.19534970331118,-3.146051407845));
#34082=CARTESIAN_POINT('Ctrl Pts',(162.543796021198,3.83454620687902,0.115996413487326));
#34083=CARTESIAN_POINT('Ctrl Pts',(162.701643037096,2.00117114015365,3.27299768537179));
#34084=CARTESIAN_POINT('Ctrl Pts',(162.859490052995,-1.64446791653823,3.46596668364093));
#34085=CARTESIAN_POINT('Ctrl Pts',(163.017337068893,-3.80087402958061,0.52015035508223));
#34086=CARTESIAN_POINT('Ctrl Pts',(163.175184084792,-2.51520215339187,-2.89671502019193));
#34087=CARTESIAN_POINT('Ctrl Pts',(163.33303110069,1.04824107309133,-3.69031034376743));
#34088=CARTESIAN_POINT('Ctrl Pts',(163.490878116589,3.66239539996482,-1.14195434013322));
#34089=CARTESIAN_POINT('Ctrl Pts',(163.648725132487,2.95987822023979,2.44055745721806));
#34090=CARTESIAN_POINT('Ctrl Pts',(163.806572148386,-0.423109712633618,
3.81289626815465));
#34091=CARTESIAN_POINT('Ctrl Pts',(163.964419164284,-3.42292876972957,1.7322697301489));
#34092=CARTESIAN_POINT('Ctrl Pts',(164.122266180182,-3.32293770807444,-1.91710322332668));
#34093=CARTESIAN_POINT('Ctrl Pts',(164.280113196081,-0.213688603260413,
-3.83034423537483));
#34094=CARTESIAN_POINT('Ctrl Pts',(164.437960211979,3.08907726430553,-2.2748189896744));
#34095=CARTESIAN_POINT('Ctrl Pts',(164.595807227878,3.59436950455589,1.34078620419185));
#34096=CARTESIAN_POINT('Ctrl Pts',(164.753654243776,0.844594604851437,3.74217312989237));
#34097=CARTESIAN_POINT('Ctrl Pts',(164.911501259674,-2.67004660627436,2.75464170101219));
#34098=CARTESIAN_POINT('Ctrl Pts',(165.069348275573,-3.76668906707262,-0.727497939947697));
#34099=CARTESIAN_POINT('Ctrl Pts',(165.227195291472,-1.45221149886039,-3.5508142084894));
#34100=CARTESIAN_POINT('Ctrl Pts',(165.38504230737,2.17739127398466,-3.15850708731325));
#34101=CARTESIAN_POINT('Ctrl Pts',(165.542889323269,3.83514480378769,0.0941494270447407));
#34102=CARTESIAN_POINT('Ctrl Pts',(165.700736339167,2.0197846729182,3.26154406005457));
#34103=CARTESIAN_POINT('Ctrl Pts',(165.858583355065,-1.62469589486439,3.47527884202741));
#34104=CARTESIAN_POINT('Ctrl Pts',(166.016430370963,-3.79784909547192,0.541795190690796));
#34105=CARTESIAN_POINT('Ctrl Pts',(166.174277386862,-2.53166369232474,-2.8823391073219));
#34106=CARTESIAN_POINT('Ctrl Pts',(166.33212440276,1.02720065878751,-3.69622220479493));
#34107=CARTESIAN_POINT('Ctrl Pts',(166.489971418659,3.6558303452886,-1.16280018365137));
#34108=CARTESIAN_POINT('Ctrl Pts',(166.647818434557,2.97373384987786,2.4236556625732));
#34109=CARTESIAN_POINT('Ctrl Pts',(166.805665450456,-0.401381080459946,
3.81524481637566));
#34110=CARTESIAN_POINT('Ctrl Pts',(166.963512466354,-3.41300462129297,1.75174177197025));
#34111=CARTESIAN_POINT('Ctrl Pts',(167.121359482253,-3.33380536908723,-1.89814160211446));
#34112=CARTESIAN_POINT('Ctrl Pts',(167.279206498151,-0.235506301415678,
-3.82906471120899));
#34113=CARTESIAN_POINT('Ctrl Pts',(167.43705351405,3.07606767358497,-2.29238030181696));
#34114=CARTESIAN_POINT('Ctrl Pts',(167.594900529948,3.60194952876521,1.32028760990183));
#34115=CARTESIAN_POINT('Ctrl Pts',(167.752747545847,0.865899761167811,3.73730081532669));
#34116=CARTESIAN_POINT('Ctrl Pts',(167.910594561745,-2.65431030366708,2.76980804253329));
#34117=CARTESIAN_POINT('Ctrl Pts',(168.068441577643,-3.77077244059341,-0.706027607031077));
#34118=CARTESIAN_POINT('Ctrl Pts',(168.226288593542,-1.47241663850212,-3.54248345420153));
#34119=CARTESIAN_POINT('Ctrl Pts',(168.38413560944,2.15936217706934,-3.17086025691717));
#34120=CARTESIAN_POINT('Ctrl Pts',(168.541982625339,3.83561893043735,0.0722993849707047));
#34121=CARTESIAN_POINT('Ctrl Pts',(168.699829641237,2.03833265324929,3.24998458078198));
#34122=CARTESIAN_POINT('Ctrl Pts',(168.857676657136,-1.60487114343804,3.48447820968375));
#34123=CARTESIAN_POINT('Ctrl Pts',(169.015523673034,-3.79470090150806,0.5634224422168));
#34124=CARTESIAN_POINT('Ctrl Pts',(169.173370688933,-2.54804306577631,-2.86786964760089));
#34125=CARTESIAN_POINT('Ctrl Pts',(169.331217704831,1.00612690667822,-3.70201410444949));
#34126=CARTESIAN_POINT('Ctrl Pts',(169.489064720729,3.64914663971395,-1.18360828804503));
#34127=CARTESIAN_POINT('Ctrl Pts',(169.646911736628,2.98749296715126,2.4066752072734));
#34128=CARTESIAN_POINT('Ctrl Pts',(169.804758752526,-0.379639422722282,
3.81746954123559));
#34129=CARTESIAN_POINT('Ctrl Pts',(169.962605768425,-3.40296970055378,1.77115695863176));
#34130=CARTESIAN_POINT('Ctrl Pts',(170.120452784323,-3.34456483630987,-1.87911837217519));
#34131=CARTESIAN_POINT('Ctrl Pts',(170.278299800222,-0.257316345241784,
-3.82766092266703));
#34132=CARTESIAN_POINT('Ctrl Pts',(170.43614681612,3.06295822648831,-2.30986719710706));
#34133=CARTESIAN_POINT('Ctrl Pts',(170.593993832019,3.60941269576124,1.29974613055387));
#34134=CARTESIAN_POINT('Ctrl Pts',(170.751840847917,0.887176724335015,3.73230727659045));
#34135=CARTESIAN_POINT('Ctrl Pts',(170.909687863816,-2.63848767264258,2.78488434692803));
#34136=CARTESIAN_POINT('Ctrl Pts',(171.067534879714,-3.77473380155604,-0.684534071799058));
#34137=CARTESIAN_POINT('Ctrl Pts',(171.225381895612,-1.49257324598161,-3.534038310181));
#34138=CARTESIAN_POINT('Ctrl Pts',(171.383228911511,2.1412614929076,-3.1831093393024));
#34139=CARTESIAN_POINT('Ctrl Pts',(171.541075927409,3.83597161238398,0.0504446190389995));
#34140=CARTESIAN_POINT('Ctrl Pts',(171.698922943308,2.05680833392007,3.23832442699998));
#34141=CARTESIAN_POINT('Ctrl Pts',(171.856769959206,-1.58498188713336,3.49355477937783));
#34142=CARTESIAN_POINT('Ctrl Pts',(172.014616975104,-3.79145464570184,0.585051027366752));
#34143=CARTESIAN_POINT('Ctrl Pts',(172.172463991003,-2.56428902756788,-2.85334675869678));
#34144=CARTESIAN_POINT('Ctrl Pts',(172.330311006901,0.984918014737876,-3.70760573227161));
#34145=CARTESIAN_POINT('Ctrl Pts',(172.4881580228,3.6425516092056,-1.20453989598447));
#34146=CARTESIAN_POINT('Ctrl Pts',(172.646005038698,3.00073656748295,2.38994390738518));
#34147=CARTESIAN_POINT('Ctrl Pts',(172.803852054597,-0.357039250344633,
3.81890829689274));
#34148=CARTESIAN_POINT('Ctrl Pts',(172.961699070495,-3.39453964146364,1.7918657477178));
#34149=CARTESIAN_POINT('Ctrl Pts',(173.119546086394,-3.35167392257996,-1.86287815540851));
#34150=CARTESIAN_POINT('Ctrl Pts',(173.224777430326,-1.30884848739072,-3.16516064263851));
#34151=CARTESIAN_POINT('Ctrl Pts',(173.277393102292,-0.236606069817846,
-3.2433811937121));
#34152=CARTESIAN_POINT('Ctrl Pts',(156.971,-1.51078263890252,3.09271722244222));
#34153=CARTESIAN_POINT('Ctrl Pts',(157.023615671966,-2.53321644899234,2.59326152099569));
#34154=CARTESIAN_POINT('Ctrl Pts',(157.128847015899,-4.02659566945348,0.50885833596795));
#34155=CARTESIAN_POINT('Ctrl Pts',(157.286694031797,-2.62820146433077,-3.09809319236867));
#34156=CARTESIAN_POINT('Ctrl Pts',(157.444541047695,1.15448610992581,-3.89204038278222));
#34157=CARTESIAN_POINT('Ctrl Pts',(157.602388063594,3.88961042992581,-1.16491561868827));
#34158=CARTESIAN_POINT('Ctrl Pts',(157.760235079492,3.10331560374578,2.61891563100415));
#34159=CARTESIAN_POINT('Ctrl Pts',(157.918082095391,-0.493851167829066,
4.03018348532901));
#34160=CARTESIAN_POINT('Ctrl Pts',(158.075929111289,-3.64353605446504,1.79214027496947));
#34161=CARTESIAN_POINT('Ctrl Pts',(158.233776127187,-3.49375191735815,-2.06908097826516));
#34162=CARTESIAN_POINT('Ctrl Pts',(158.391623143086,-0.179959021063511,
-4.05643369351328));
#34163=CARTESIAN_POINT('Ctrl Pts',(158.549470158984,3.29677484711022,-2.37032525173271));
#34164=CARTESIAN_POINT('Ctrl Pts',(158.707317174883,3.78795875964091,1.46237955244845));
#34165=CARTESIAN_POINT('Ctrl Pts',(158.865164190781,0.848753372427349,3.97073818787796));
#34166=CARTESIAN_POINT('Ctrl Pts',(159.02301120668,-2.85908085088131,2.88319587623426));
#34167=CARTESIAN_POINT('Ctrl Pts',(159.180858222578,-3.97772840254164,-0.815376651275756));
#34168=CARTESIAN_POINT('Ctrl Pts',(159.338705238477,-1.49413744706287,-3.77554114997762));
#34169=CARTESIAN_POINT('Ctrl Pts',(159.496552254375,2.34254647931214,-3.31656992328989));
#34170=CARTESIAN_POINT('Ctrl Pts',(159.654399270274,4.05781654725159,0.145893048357734));
#34171=CARTESIAN_POINT('Ctrl Pts',(159.812246286172,2.09832093604372,3.47623483982516));
#34172=CARTESIAN_POINT('Ctrl Pts',(159.970093302071,-1.76141763183718,3.65849253744375));
#34173=CARTESIAN_POINT('Ctrl Pts',(160.127940317969,-4.02601342148726,0.527613121535813));
#34174=CARTESIAN_POINT('Ctrl Pts',(160.285787333867,-2.64464459230254,-3.0810736123896));
#34175=CARTESIAN_POINT('Ctrl Pts',(160.443634349766,1.13171887361366,-3.89953485102645));
#34176=CARTESIAN_POINT('Ctrl Pts',(160.601481365664,3.88319580493523,-1.18657068707914));
#34177=CARTESIAN_POINT('Ctrl Pts',(160.759328381563,3.1180440055799,2.60095390755385));
#34178=CARTESIAN_POINT('Ctrl Pts',(160.917175397461,-0.470813750492941,
4.03305021875839));
#34179=CARTESIAN_POINT('Ctrl Pts',(161.07502241336,-3.63330177331448,1.81280938803883));
#34180=CARTESIAN_POINT('Ctrl Pts',(161.232869429258,-3.50546552714807,-2.04911470905875));
#34181=CARTESIAN_POINT('Ctrl Pts',(161.390716445157,-0.203073734353165,
-4.05535703876761));
#34182=CARTESIAN_POINT('Ctrl Pts',(161.548563461055,3.28322197789498,-2.38906113298382));
#34183=CARTESIAN_POINT('Ctrl Pts',(161.706410476954,3.79622627979659,1.44077260031516));
#34184=CARTESIAN_POINT('Ctrl Pts',(161.864257492852,0.871361602592233,3.96584021498973));
#34185=CARTESIAN_POINT('Ctrl Pts',(162.02210450875,-2.84260962474333,2.89943618218967));
#34186=CARTESIAN_POINT('Ctrl Pts',(162.179951524649,-3.9823087385682,-0.792702191239944));
#34187=CARTESIAN_POINT('Ctrl Pts',(162.337798540547,-1.51562228195216,-3.76696811132383));
#34188=CARTESIAN_POINT('Ctrl Pts',(162.495645556446,2.32361429237301,-3.32986129944727));
#34189=CARTESIAN_POINT('Ctrl Pts',(162.653492572344,4.05858180937195,0.122773571716884));
#34190=CARTESIAN_POINT('Ctrl Pts',(162.811339588243,2.11809073321307,3.46422448740764));
#34191=CARTESIAN_POINT('Ctrl Pts',(162.969186604141,-1.74054691535194,3.66846781214395));
#34192=CARTESIAN_POINT('Ctrl Pts',(163.127033620039,-4.02294231544172,0.550540443478812));
#34193=CARTESIAN_POINT('Ctrl Pts',(163.284880635938,-2.66215430872536,-3.0659572876693));
#34194=CARTESIAN_POINT('Ctrl Pts',(163.442727651836,1.10948517022764,-3.90591888168743));
#34195=CARTESIAN_POINT('Ctrl Pts',(163.600574667735,3.87637299098367,-1.20867368964902));
#34196=CARTESIAN_POINT('Ctrl Pts',(163.758421683633,3.13281083458346,2.58314845256596));
#34197=CARTESIAN_POINT('Ctrl Pts',(163.916268699532,-0.447830144798535,
4.03566696032851));
#34198=CARTESIAN_POINT('Ctrl Pts',(164.07411571543,-3.62291538296715,1.83347860122158));
#34199=CARTESIAN_POINT('Ctrl Pts',(164.231962731329,-3.51708228511447,-2.02911109922828));
#34200=CARTESIAN_POINT('Ctrl Pts',(164.389809747227,-0.226173484754741,
-4.0541343352276));
#34201=CARTESIAN_POINT('Ctrl Pts',(164.547656763125,3.26955840828401,-2.40772661822243));
#34202=CARTESIAN_POINT('Ctrl Pts',(164.705503779024,3.80437264289096,1.41912242153392));
#34203=CARTESIAN_POINT('Ctrl Pts',(164.863350794922,0.893940538099236,3.96081178139284));
#34204=CARTESIAN_POINT('Ctrl Pts',(165.021197810821,-2.82604563923625,2.91558325180936));
#34205=CARTESIAN_POINT('Ctrl Pts',(165.179044826719,-3.98676007652644,-0.770002432134042));
#34206=CARTESIAN_POINT('Ctrl Pts',(165.336891842617,-1.53705780414438,-3.75827260320434));
#34207=CARTESIAN_POINT('Ctrl Pts',(165.494738858516,2.30460663132077,-3.34304470926576));
#34208=CARTESIAN_POINT('Ctrl Pts',(165.652585874414,4.05921537965474,0.0996501623271599));
#34209=CARTESIAN_POINT('Ctrl Pts',(165.810432890313,2.13779177250447,3.45210167733942));
#34210=CARTESIAN_POINT('Ctrl Pts',(165.968279906211,-1.71961970175989,3.67832403882484));
#34211=CARTESIAN_POINT('Ctrl Pts',(166.12612692211,-4.01974064779039,0.573449891253934));
#34212=CARTESIAN_POINT('Ctrl Pts',(166.283973938008,-2.67957762268814,-3.05074145369063));
#34213=CARTESIAN_POINT('Ctrl Pts',(166.441820953907,1.08721545742514,-3.9121761466495));
#34214=CARTESIAN_POINT('Ctrl Pts',(166.599667969805,3.86942436915232,-1.23073746375402));
#34215=CARTESIAN_POINT('Ctrl Pts',(166.757514985703,3.14747598747837,2.565259160694));
#34216=CARTESIAN_POINT('Ctrl Pts',(166.915362001602,-0.424832004595041,
4.03815272385149));
#34217=CARTESIAN_POINT('Ctrl Pts',(167.0732090175,-3.61241141035989,1.854088308463));
#34218=CARTESIAN_POINT('Ctrl Pts',(167.231056033399,-3.52858489557144,-2.0090416342183));
#34219=CARTESIAN_POINT('Ctrl Pts',(167.388903049297,-0.24926589467184,-4.0527800541148));
#34220=CARTESIAN_POINT('Ctrl Pts',(167.546750065196,3.25578872462467,-2.42631396028723));
#34221=CARTESIAN_POINT('Ctrl Pts',(167.704597081094,3.81239553444338,1.39742618489607));
#34222=CARTESIAN_POINT('Ctrl Pts',(167.862444096993,0.916490460621058,3.95565479900198));
#34223=CARTESIAN_POINT('Ctrl Pts',(168.020291112891,-2.80938993395512,2.93163569569484));
#34224=CARTESIAN_POINT('Ctrl Pts',(168.178138128789,-3.99108202353092,-0.747277682472601));
#34225=CARTESIAN_POINT('Ctrl Pts',(168.335985144688,-1.55844344087465,-3.74945511972991));
#34226=CARTESIAN_POINT('Ctrl Pts',(168.493832160586,2.28552417388456,-3.3561196200212));
#34227=CARTESIAN_POINT('Ctrl Pts',(168.651679176485,4.05971720743093,0.0765235187789346));
#34228=CARTESIAN_POINT('Ctrl Pts',(168.809526192383,2.15742342942316,3.43986682873663));
#34229=CARTESIAN_POINT('Ctrl Pts',(168.967373208282,-1.69863667764873,3.68806088491128));
#34230=CARTESIAN_POINT('Ctrl Pts',(169.12522022418,-4.01640851875484,0.596340727586192));
#34231=CARTESIAN_POINT('Ctrl Pts',(169.283067240078,-2.69691397060336,-3.03542660733155));
#34232=CARTESIAN_POINT('Ctrl Pts',(169.440914255977,1.0649104590364,-3.91830644142532));
#34233=CARTESIAN_POINT('Ctrl Pts',(169.598761271875,3.86235016417448,-1.25276129380414));
#34234=CARTESIAN_POINT('Ctrl Pts',(169.756608287774,3.16203898921731,2.54728661237238));
#34235=CARTESIAN_POINT('Ctrl Pts',(169.914455303672,-0.401820077801361,
4.04050742956116));
#34236=CARTESIAN_POINT('Ctrl Pts',(170.072302319571,-3.60179019351355,1.87463783874864));
#34237=CARTESIAN_POINT('Ctrl Pts',(170.230149335469,-3.53997299095283,-1.98890696095539));
#34238=CARTESIAN_POINT('Ctrl Pts',(170.387996351368,-0.272350203051137,
-4.05129424840711));
#34239=CARTESIAN_POINT('Ctrl Pts',(170.545843367266,3.24191335042212,-2.44482253765146));
#34240=CARTESIAN_POINT('Ctrl Pts',(170.703690383165,3.82029474133155,1.37568455761573));
#34241=CARTESIAN_POINT('Ctrl Pts',(170.861537399063,0.939010542792494,3.95036950984758));
#34242=CARTESIAN_POINT('Ctrl Pts',(171.019384414962,-2.79264285646855,2.94759284198226));
#34243=CARTESIAN_POINT('Ctrl Pts',(171.17723143086,-3.99527482932224,-0.724528374886929));
#34244=CARTESIAN_POINT('Ctrl Pts',(171.335078446758,-1.57977770992274,-3.74051656323585));
#34245=CARTESIAN_POINT('Ctrl Pts',(171.492925462657,2.26636594667525,-3.36908436220139));
#34246=CARTESIAN_POINT('Ctrl Pts',(171.650772478555,4.06009049502634,0.0533918753788966));
#34247=CARTESIAN_POINT('Ctrl Pts',(171.808619494454,2.17697856253166,3.42752542365741));
#34248=CARTESIAN_POINT('Ctrl Pts',(171.966466510352,-1.67758537992403,3.69766775849278));
#34249=CARTESIAN_POINT('Ctrl Pts',(172.12431352625,-4.0129725985565,0.619232975460156));
#34250=CARTESIAN_POINT('Ctrl Pts',(172.282160542149,-2.7141091122044,-3.02005521015814));
#34251=CARTESIAN_POINT('Ctrl Pts',(172.440007558047,1.04246242519302,-3.9242247633699));
#34252=CARTESIAN_POINT('Ctrl Pts',(172.597854573946,3.85536981515549,-1.27491584316685));
#34253=CARTESIAN_POINT('Ctrl Pts',(172.755701589844,3.17605635463602,2.52957777651284));
#34254=CARTESIAN_POINT('Ctrl Pts',(172.913548605743,-0.377899477148265,
4.04203024535818));
#34255=CARTESIAN_POINT('Ctrl Pts',(173.071395621641,-3.59286760329576,1.89655655093627));
#34256=CARTESIAN_POINT('Ctrl Pts',(173.22924263754,-3.54749742974178,-1.97171790003568));
#34257=CARTESIAN_POINT('Ctrl Pts',(173.334473981472,-1.38531872496892,-3.35008700244825));
#34258=CARTESIAN_POINT('Ctrl Pts',(173.387089653438,-0.25042991768545,-3.43287763491915));
#34259=CARTESIAN_POINT('Ctrl Pts',(172.148679545343,-3.44468745739532,0.00260595186748766));
#34260=CARTESIAN_POINT('Ctrl Pts',(172.193173210945,-3.43659168049753,-0.9575193993669));
#34261=CARTESIAN_POINT('Ctrl Pts',(172.237666876547,-3.01700009266596,-1.92385078687646));
#34262=CARTESIAN_POINT('Ctrl Pts',(172.282160542149,-2.30449110369684,-2.56420210475706));
#34263=CARTESIAN_POINT('Ctrl Pts',(172.334776214115,-1.46191859973859,-3.32144506122872));
#34264=CARTESIAN_POINT('Ctrl Pts',(172.387391886081,-0.20972808727278,-3.62283491229931));
#34265=CARTESIAN_POINT('Ctrl Pts',(172.440007558047,0.885185067287182,-3.3319783511341));
#34266=CARTESIAN_POINT('Ctrl Pts',(172.492623230014,1.98009822184718,-3.04112178996889));
#34267=CARTESIAN_POINT('Ctrl Pts',(172.54523890198,2.91773401850134,-2.15801881656787));
#34268=CARTESIAN_POINT('Ctrl Pts',(172.597854573946,3.27333300674184,-1.08238505992073));
#34269=CARTESIAN_POINT('Ctrl Pts',(172.650470245912,3.62893199498233,-0.00675130327361259));
#34270=CARTESIAN_POINT('Ctrl Pts',(172.703085917878,3.40249417480918,1.2614132366196));
#34271=CARTESIAN_POINT('Ctrl Pts',(172.755701589844,2.69694929275856,2.14757091804043));
#34272=CARTESIAN_POINT('Ctrl Pts',(172.80831726181,1.99140441070795,3.03372859946126));
#34273=CARTESIAN_POINT('Ctrl Pts',(172.860932933777,0.80675246677985,3.53787942240972));
#34274=CARTESIAN_POINT('Ctrl Pts',(172.913548605743,-0.321401526208764,
3.43237588481364));
#34275=CARTESIAN_POINT('Ctrl Pts',(172.961699070495,-1.35381519774084,3.33582586124758));
#34276=CARTESIAN_POINT('Ctrl Pts',(173.009849535248,-2.33891337062945,2.72870687739777));
#34277=CARTESIAN_POINT('Ctrl Pts',(173.058,-2.9035416885497,1.85819928779561));
#34278=CARTESIAN_POINT('',(156.971,-1.66746714335626,-2.33836210323109));
#34279=CARTESIAN_POINT('Ctrl Pts',(156.971,-1.67108163325028,-2.34115360979857));
#34280=CARTESIAN_POINT('Ctrl Pts',(156.971,-1.74156582682502,-2.30101299952705));
#34281=CARTESIAN_POINT('Ctrl Pts',(156.971,-1.81009195136928,-2.25780466502739));
#34282=CARTESIAN_POINT('Ctrl Pts',(156.971,-1.87643000725441,-2.2115735151457));
#34283=CARTESIAN_POINT('Ctrl Pts',(156.971,-1.95407697057863,-2.15746116060946));
#34284=CARTESIAN_POINT('Ctrl Pts',(156.971,-2.0287275990739,-2.0992089256144));
#34285=CARTESIAN_POINT('Ctrl Pts',(156.971,-2.10029440757325,-2.03719493253877));
#34286=CARTESIAN_POINT('Ctrl Pts',(156.971,-2.14317936038372,-2.00003430986464));
#34287=CARTESIAN_POINT('Ctrl Pts',(156.971,-2.18495660149505,-1.96152195550082));
#34288=CARTESIAN_POINT('Ctrl Pts',(156.971,-2.22560317199605,-1.92173149895334));
#34289=CARTESIAN_POINT('Ctrl Pts',(156.971,-2.23928658627073,-1.90833629009791));
#34290=CARTESIAN_POINT('Ctrl Pts',(156.971,-2.25284183387164,-1.89479619102025));
#34291=CARTESIAN_POINT('Ctrl Pts',(156.971,-2.26626794759505,-1.88111388128463));
#34292=CARTESIAN_POINT('Ctrl Pts',(156.971,-2.27898720160856,-1.86815191949852));
#34293=CARTESIAN_POINT('Ctrl Pts',(156.971,-2.29158455101912,-1.85506841721476));
#34294=CARTESIAN_POINT('Ctrl Pts',(156.971,-2.30405686724598,-1.8418688091367));
#34295=CARTESIAN_POINT('Ctrl Pts',(156.971,-2.3741795820906,-1.7676570639818));
#34296=CARTESIAN_POINT('Ctrl Pts',(156.971,-2.44037916018597,-1.68975253852306));
#34297=CARTESIAN_POINT('Ctrl Pts',(156.971,-2.50254990372574,-1.60861131636701));
#34298=CARTESIAN_POINT('Ctrl Pts',(156.971,-2.55694930432303,-1.53761274698046));
#34299=CARTESIAN_POINT('Ctrl Pts',(156.971,-2.60826396461782,-1.46413480075326));
#34300=CARTESIAN_POINT('Ctrl Pts',(156.971,-2.65640196169989,-1.3884517272919));
#34301=CARTESIAN_POINT('Ctrl Pts',(156.971,-2.68077979569537,-1.35012463615922));
#34302=CARTESIAN_POINT('Ctrl Pts',(156.971,-2.70434261126781,-1.31123160616743));
#34303=CARTESIAN_POINT('Ctrl Pts',(156.971,-2.72707617605973,-1.27180597383338));
#34304=CARTESIAN_POINT('Ctrl Pts',(156.971,-2.73546680340987,-1.25725454769381));
#34305=CARTESIAN_POINT('Ctrl Pts',(156.971,-2.74374453865664,-1.24263023968055));
#34306=CARTESIAN_POINT('Ctrl Pts',(156.971,-2.75190137317708,-1.22794817412566));
#34307=CARTESIAN_POINT('Ctrl Pts',(156.971,-2.80132721807123,-1.13898308687001));
#34308=CARTESIAN_POINT('Ctrl Pts',(156.971,-2.84638527771199,-1.04778307946572));
#34309=CARTESIAN_POINT('Ctrl Pts',(156.971,-2.88697808172597,-0.95476457681926));
#34310=CARTESIAN_POINT('Ctrl Pts',(156.971,-2.92819643846301,-0.860312618686309));
#34311=CARTESIAN_POINT('Ctrl Pts',(156.971,-2.96481143066595,-0.763984967763502));
#34312=CARTESIAN_POINT('Ctrl Pts',(156.971,-2.9966850422333,-0.666177951518305));
#34313=CARTESIAN_POINT('Ctrl Pts',(156.971,-3.02841101938765,-0.568823964619975));
#34314=CARTESIAN_POINT('Ctrl Pts',(156.971,-3.05543990645514,-0.470003430106361));
#34315=CARTESIAN_POINT('Ctrl Pts',(156.971,-3.07759256720278,-0.37008023699904));
#34316=CARTESIAN_POINT('Ctrl Pts',(156.971,-3.09152323719072,-0.30724367559562));
#34317=CARTESIAN_POINT('Ctrl Pts',(156.971,-3.10352472126607,-0.243970573036485));
#34318=CARTESIAN_POINT('Ctrl Pts',(156.971,-3.11354240097713,-0.180348235662287));
#34319=CARTESIAN_POINT('Ctrl Pts',(156.971,-3.11596207334912,-0.164980883498373));
#34320=CARTESIAN_POINT('Ctrl Pts',(156.971,-3.11826596901285,-0.149593149423556));
#34321=CARTESIAN_POINT('Ctrl Pts',(156.971,-3.12045324378791,-0.134186252698088));
#34322=CARTESIAN_POINT('Ctrl Pts',(156.971,-3.1225086104187,-0.119708500851479));
#34323=CARTESIAN_POINT('Ctrl Pts',(156.971,-3.12445959438249,-0.105223701268543));
#34324=CARTESIAN_POINT('Ctrl Pts',(156.971,-3.12630586019491,-0.0907332361958907));
#34325=CARTESIAN_POINT('Ctrl Pts',(156.971,-3.13964539671036,0.0139624618244236));
#34326=CARTESIAN_POINT('Ctrl Pts',(156.971,-3.14752256490358,0.118955963700162));
#34327=CARTESIAN_POINT('Ctrl Pts',(156.971,-3.14979998981073,0.223838097043022));
#34328=CARTESIAN_POINT('Ctrl Pts',(156.971,-3.15103815096673,0.280859069745446));
#34329=CARTESIAN_POINT('Ctrl Pts',(156.971,-3.15062042229049,0.337847632866582));
#34330=CARTESIAN_POINT('Ctrl Pts',(156.971,-3.14851887087268,0.394740793443));
#34331=CARTESIAN_POINT('Ctrl Pts',(156.971,-3.14477596423555,0.496068691739228));
#34332=CARTESIAN_POINT('Ctrl Pts',(156.971,-3.13569517353071,0.597093830712654));
#34333=CARTESIAN_POINT('Ctrl Pts',(156.971,-3.1215328967269,0.697540099410437));
#34334=CARTESIAN_POINT('Ctrl Pts',(156.971,-3.10710264617045,0.799886978012563));
#34335=CARTESIAN_POINT('Ctrl Pts',(156.971,-3.08739665071869,0.90163358834031));
#34336=CARTESIAN_POINT('Ctrl Pts',(156.971,-3.06263213549149,1.00248789881405));
#34337=CARTESIAN_POINT('Ctrl Pts',(156.971,-3.05639992686936,1.02786877534427));
#34338=CARTESIAN_POINT('Ctrl Pts',(156.971,-3.04984709488345,1.05319311007923));
#34339=CARTESIAN_POINT('Ctrl Pts',(156.971,-3.04297659426579,1.07845616335264));
#34340=CARTESIAN_POINT('Ctrl Pts',(156.971,-3.03886751101771,1.09356539552918));
#34341=CARTESIAN_POINT('Ctrl Pts',(156.971,-3.03464709377404,1.10864418789391));
#34342=CARTESIAN_POINT('Ctrl Pts',(156.971,-3.0303173931493,1.12368807181908));
#34343=CARTESIAN_POINT('Ctrl Pts',(156.971,-3.00104329645236,1.22540321355577));
#34344=CARTESIAN_POINT('Ctrl Pts',(156.971,-2.96676399966351,1.32557352761962));
#34345=CARTESIAN_POINT('Ctrl Pts',(156.971,-2.92778796706529,1.42390018595887));
#34346=CARTESIAN_POINT('Ctrl Pts',(156.971,-2.88830860897673,1.52349660702726));
#34347=CARTESIAN_POINT('Ctrl Pts',(156.971,-2.84401017748247,1.62120220936028));
#34348=CARTESIAN_POINT('Ctrl Pts',(156.971,-2.79515759563137,1.7167066642448));
#34349=CARTESIAN_POINT('Ctrl Pts',(156.971,-2.74593458387645,1.81293529182803));
#34350=CARTESIAN_POINT('Ctrl Pts',(156.971,-2.69208777854597,1.90693009151836));
#34351=CARTESIAN_POINT('Ctrl Pts',(156.971,-2.63383640916819,1.99836181408463));
#34352=CARTESIAN_POINT('Ctrl Pts',(156.971,-2.59840301290045,2.05397829987267));
#34353=CARTESIAN_POINT('Ctrl Pts',(156.971,-2.56133889987228,2.10864614082127));
#34354=CARTESIAN_POINT('Ctrl Pts',(156.971,-2.52268492979926,2.16228709920977));
#34355=CARTESIAN_POINT('Ctrl Pts',(156.971,-2.51023398438858,2.17956554805759));
#34356=CARTESIAN_POINT('Ctrl Pts',(156.971,-2.49761803355936,2.19673742063913));
#34357=CARTESIAN_POINT('Ctrl Pts',(156.971,-2.48483831170471,2.2138000097301));
#34358=CARTESIAN_POINT('Ctrl Pts',(156.971,-2.475084819656,2.22682218884494));
#34359=CARTESIAN_POINT('Ctrl Pts',(156.971,-2.46524087000302,2.23977408134567));
#34360=CARTESIAN_POINT('Ctrl Pts',(156.971,-2.45531045458567,2.25265065830578));
#34361=CARTESIAN_POINT('Ctrl Pts',(156.971,-2.38739538388514,2.34071481251011));
#34362=CARTESIAN_POINT('Ctrl Pts',(156.971,-2.31539519512402,2.42531743730386));
#34363=CARTESIAN_POINT('Ctrl Pts',(156.971,-2.23958992023872,2.50613621189154));
#34364=CARTESIAN_POINT('Ctrl Pts',(156.971,-2.16373640953125,2.58700641245246));
#34365=CARTESIAN_POINT('Ctrl Pts',(156.971,-2.0840725443841,2.66408878647399));
#34366=CARTESIAN_POINT('Ctrl Pts',(156.971,-2.00083019937915,2.73704166286336));
#34367=CARTESIAN_POINT('Ctrl Pts',(156.971,-1.91931149938911,2.80848395156199));
#34368=CARTESIAN_POINT('Ctrl Pts',(156.971,-1.83436044394798,2.87596668131474));
#34369=CARTESIAN_POINT('Ctrl Pts',(156.971,-1.74615546237234,2.93913980004792));
#34370=CARTESIAN_POINT('Ctrl Pts',(156.971,-1.67008718098456,2.99362051628523));
#34371=CARTESIAN_POINT('Ctrl Pts',(156.971,-1.59159806355185,3.04489584580896));
#34372=CARTESIAN_POINT('Ctrl Pts',(156.971,-1.51078263890252,3.09271722244222));
#34373=CARTESIAN_POINT('Ctrl Pts',(156.971,-1.67108163325026,-2.34115360979858));
#34374=CARTESIAN_POINT('Ctrl Pts',(157.019150464752,-0.963356763333181,
-2.83982097002305));
#34375=CARTESIAN_POINT('Ctrl Pts',(157.119916601471,1.02786046454763,-3.18314302195819));
#34376=CARTESIAN_POINT('Ctrl Pts',(157.273298410156,3.24548551852033,-0.972003967714269));
#34377=CARTESIAN_POINT('Ctrl Pts',(157.431145426054,2.58940221207372,2.18521955033239));
#34378=CARTESIAN_POINT('Ctrl Pts',(157.588992441952,-0.412068725742385,
3.36277947991426));
#34379=CARTESIAN_POINT('Ctrl Pts',(157.71847393057,-2.56788618045525,1.83093969563411));
#34380=CARTESIAN_POINT('Ctrl Pts',(157.79533974722,-2.86840235184534,0.439819957054708));
#34381=CARTESIAN_POINT('Ctrl Pts',(157.819589891905,-2.86758689937222,0.000602879185874344));
#34382=CARTESIAN_POINT('Origin',(156.971,-8.10351388986772E-16,-1.22178682300763E-16));
#34383=CARTESIAN_POINT('',(156.971,-3.442,-4.21523428266519E-16));
#34384=CARTESIAN_POINT('Origin',(156.971,0.,0.));
#34385=CARTESIAN_POINT('Origin',(156.971,0.,0.));
#34386=CARTESIAN_POINT('',(156.971,1.66746714335746,-2.33836210323023));
#34387=CARTESIAN_POINT('Ctrl Pts',(156.971,1.51450577336034,3.09672906731566));
#34388=CARTESIAN_POINT('Ctrl Pts',(156.971,1.5976122133282,3.04813379956916));
#34389=CARTESIAN_POINT('Ctrl Pts',(156.971,1.67839168866948,2.99593162634641));
#34390=CARTESIAN_POINT('Ctrl Pts',(156.971,1.75657288137401,2.94011204420089));
#34391=CARTESIAN_POINT('Ctrl Pts',(156.971,1.84626732484938,2.87607226452533));
#34392=CARTESIAN_POINT('Ctrl Pts',(156.971,1.93254295618487,2.80727123920175));
#34393=CARTESIAN_POINT('Ctrl Pts',(156.971,2.0152189467617,2.73410403576512));
#34394=CARTESIAN_POINT('Ctrl Pts',(156.971,2.06094021411052,2.69364129384751));
#34395=CARTESIAN_POINT('Ctrl Pts',(156.971,2.10555989642535,2.65184263331913));
#34396=CARTESIAN_POINT('Ctrl Pts',(156.971,2.14904172716354,2.60877124230549));
#34397=CARTESIAN_POINT('Ctrl Pts',(156.971,2.16594615215952,2.59202638390138));
#34398=CARTESIAN_POINT('Ctrl Pts',(156.971,2.18267855444771,2.57508914036822));
#34399=CARTESIAN_POINT('Ctrl Pts',(156.971,2.19923662551325,2.55796314915767));
#34400=CARTESIAN_POINT('Ctrl Pts',(156.971,2.21227815538319,2.54447431189873));
#34401=CARTESIAN_POINT('Ctrl Pts',(156.971,2.22521082737741,2.53086901431116));
#34402=CARTESIAN_POINT('Ctrl Pts',(156.971,2.23802494129898,2.51715852867729));
#34403=CARTESIAN_POINT('Ctrl Pts',(156.971,2.3130983252954,2.43683361826452));
#34404=CARTESIAN_POINT('Ctrl Pts',(156.971,2.38418748200277,2.35281708657033));
#34405=CARTESIAN_POINT('Ctrl Pts',(156.971,2.45111847796041,2.26550571111247));
#34406=CARTESIAN_POINT('Ctrl Pts',(156.971,2.50946613003779,2.1893912937977));
#34407=CARTESIAN_POINT('Ctrl Pts',(156.971,2.56465324413205,2.11077199669919));
#34408=CARTESIAN_POINT('Ctrl Pts',(156.971,2.61653549626154,2.02989655843326));
#34409=CARTESIAN_POINT('Ctrl Pts',(156.971,2.6392339815682,1.99451355419192));
#34410=CARTESIAN_POINT('Ctrl Pts',(156.971,2.66129952851454,1.95869858631448));
#34411=CARTESIAN_POINT('Ctrl Pts',(156.971,2.68271827828137,1.92247205653849));
#34412=CARTESIAN_POINT('Ctrl Pts',(156.971,2.69702185774087,1.89827974593054));
#34413=CARTESIAN_POINT('Ctrl Pts',(156.971,2.71103696537232,1.87390388858616));
#34414=CARTESIAN_POINT('Ctrl Pts',(156.971,2.72475919182257,1.84935053082851));
#34415=CARTESIAN_POINT('Ctrl Pts',(156.971,2.73246069787352,1.83557012616698));
#34416=CARTESIAN_POINT('Ctrl Pts',(156.971,2.74006809732495,1.82173703740762));
#34417=CARTESIAN_POINT('Ctrl Pts',(156.971,2.7475769083573,1.80785967126201));
#34418=CARTESIAN_POINT('Ctrl Pts',(156.971,2.79902208258213,1.71278156687673));
#34419=CARTESIAN_POINT('Ctrl Pts',(156.971,2.84589995525172,1.61552594512813));
#34420=CARTESIAN_POINT('Ctrl Pts',(156.971,2.88804364556441,1.51646223851979));
#34421=CARTESIAN_POINT('Ctrl Pts',(156.971,2.92990919612424,1.41805233215221));
#34422=CARTESIAN_POINT('Ctrl Pts',(156.971,2.96710310392466,1.31785723800263));
#34423=CARTESIAN_POINT('Ctrl Pts',(156.971,2.99941240513831,1.21622594408559));
#34424=CARTESIAN_POINT('Ctrl Pts',(156.971,3.03075374377295,1.1176394479721));
#34425=CARTESIAN_POINT('Ctrl Pts',(156.971,3.05749880022788,1.01770075724612));
#34426=CARTESIAN_POINT('Ctrl Pts',(156.971,3.07940480525096,0.916728058706169));
#34427=CARTESIAN_POINT('Ctrl Pts',(156.971,3.09348952736189,0.851806481347487));
#34428=CARTESIAN_POINT('Ctrl Pts',(156.971,3.10557281263683,0.786457470967977));
#34429=CARTESIAN_POINT('Ctrl Pts',(156.971,3.1155789372591,0.720767651007633));
#34430=CARTESIAN_POINT('Ctrl Pts',(156.971,3.11874731606386,0.699967367070817));
#34431=CARTESIAN_POINT('Ctrl Pts',(156.971,3.12170736344965,0.679132930743779));
#34432=CARTESIAN_POINT('Ctrl Pts',(156.971,3.1244564832137,0.658267149344455));
#34433=CARTESIAN_POINT('Ctrl Pts',(156.971,3.12656936527807,0.6422304033816));
#34434=CARTESIAN_POINT('Ctrl Pts',(156.971,3.12855665844618,0.626182400243434));
#34435=CARTESIAN_POINT('Ctrl Pts',(156.971,3.1304167981429,0.610131368191127));
#34436=CARTESIAN_POINT('Ctrl Pts',(156.971,3.14217399496676,0.508679233495234));
#34437=CARTESIAN_POINT('Ctrl Pts',(156.971,3.14886713191197,0.407018714846757));
#34438=CARTESIAN_POINT('Ctrl Pts',(156.971,3.15030637585759,0.305461515249309));
#34439=CARTESIAN_POINT('Ctrl Pts',(156.971,3.15115016476314,0.245921338922451));
#34440=CARTESIAN_POINT('Ctrl Pts',(156.971,3.15018716918967,0.186416637507053));
#34441=CARTESIAN_POINT('Ctrl Pts',(156.971,3.14737077987805,0.127010997247052));
#34442=CARTESIAN_POINT('Ctrl Pts',(156.971,3.14248054125356,0.023861991776158));
#34443=CARTESIAN_POINT('Ctrl Pts',(156.971,3.13200499774187,-0.0789895992824285));
#34444=CARTESIAN_POINT('Ctrl Pts',(156.971,3.11615067386057,-0.181195593903271));
#34445=CARTESIAN_POINT('Ctrl Pts',(156.971,3.10022872402003,-0.283837543944141));
#34446=CARTESIAN_POINT('Ctrl Pts',(156.971,3.0788814745367,-0.385829206510234));
#34447=CARTESIAN_POINT('Ctrl Pts',(156.971,3.05227309403315,-0.486791749188485));
#34448=CARTESIAN_POINT('Ctrl Pts',(156.971,3.04731684429539,-0.505597688001841));
#34449=CARTESIAN_POINT('Ctrl Pts',(156.971,3.04217794647225,-0.524367828260039));
#34450=CARTESIAN_POINT('Ctrl Pts',(156.971,3.03685731319712,-0.543099585892552));
#34451=CARTESIAN_POINT('Ctrl Pts',(156.971,3.03263009161328,-0.557981891451461));
#34452=CARTESIAN_POINT('Ctrl Pts',(156.971,3.0282903986042,-0.572831979422245));
#34453=CARTESIAN_POINT('Ctrl Pts',(156.971,3.02384043003072,-0.587644229154542));
#34454=CARTESIAN_POINT('Ctrl Pts',(156.971,2.99455675703092,-0.685118418104316));
#34455=CARTESIAN_POINT('Ctrl Pts',(156.971,2.96048389838246,-0.781018415258394));
#34456=CARTESIAN_POINT('Ctrl Pts',(156.971,2.92185171768902,-0.875024422665997));
#34457=CARTESIAN_POINT('Ctrl Pts',(156.971,2.88316491075989,-0.969163355376433));
#34458=CARTESIAN_POINT('Ctrl Pts',(156.971,2.83990529823815,-1.06140371995399));
#34459=CARTESIAN_POINT('Ctrl Pts',(156.971,2.79225847108116,-1.15139825807016));
#34460=CARTESIAN_POINT('Ctrl Pts',(156.971,2.74521780506821,-1.24024788905535));
#34461=CARTESIAN_POINT('Ctrl Pts',(156.971,2.69390022278398,-1.32690912442467));
#34462=CARTESIAN_POINT('Ctrl Pts',(156.971,2.63844931031572,-1.41101183192941));
#34463=CARTESIAN_POINT('Ctrl Pts',(156.971,2.60730719276541,-1.45824525491251));
#34464=CARTESIAN_POINT('Ctrl Pts',(156.971,2.57486079116401,-1.50467098225265));
#34465=CARTESIAN_POINT('Ctrl Pts',(156.971,2.54113168514896,-1.55021721735793));
#34466=CARTESIAN_POINT('Ctrl Pts',(156.971,2.53163696619057,-1.56303844961189));
#34467=CARTESIAN_POINT('Ctrl Pts',(156.971,2.5220405886108,-1.57578995917095));
#34468=CARTESIAN_POINT('Ctrl Pts',(156.971,2.51234300050255,-1.58847007178006));
#34469=CARTESIAN_POINT('Ctrl Pts',(156.971,2.50309786488165,-1.60055857868));
#34470=CARTESIAN_POINT('Ctrl Pts',(156.971,2.49376578236826,-1.61257556802877));
#34471=CARTESIAN_POINT('Ctrl Pts',(156.971,2.48435028538722,-1.62451626608972));
#34472=CARTESIAN_POINT('Ctrl Pts',(156.971,2.42322328666443,-1.70203729727816));
#34473=CARTESIAN_POINT('Ctrl Pts',(156.971,2.35854536219489,-1.77639557833669));
#34474=CARTESIAN_POINT('Ctrl Pts',(156.971,2.29048943148814,-1.84727574318768));
#34475=CARTESIAN_POINT('Ctrl Pts',(156.971,2.22340718132701,-1.91714182099481));
#34476=CARTESIAN_POINT('Ctrl Pts',(156.971,2.15304229743094,-1.98362914136461));
#34477=CARTESIAN_POINT('Ctrl Pts',(156.971,2.07953071995107,-2.0463957114678));
#34478=CARTESIAN_POINT('Ctrl Pts',(156.971,2.00832220888232,-2.10719584874094));
#34479=CARTESIAN_POINT('Ctrl Pts',(156.971,1.93416053444636,-2.16450503885106));
#34480=CARTESIAN_POINT('Ctrl Pts',(156.971,1.85714962127244,-2.21796859445852));
#34481=CARTESIAN_POINT('Ctrl Pts',(156.971,1.79571995702034,-2.26061512512972));
#34482=CARTESIAN_POINT('Ctrl Pts',(156.971,1.73247691508609,-2.30081400188467));
#34483=CARTESIAN_POINT('Ctrl Pts',(156.971,1.66746714335763,-2.33836210323011));
#34484=CARTESIAN_POINT('Origin',(156.971,0.,0.));
#34485=CARTESIAN_POINT('Origin',(155.122410108095,0.,0.));
#34486=CARTESIAN_POINT('Ctrl Pts',(156.971,1.66746714335746,-2.33836210323023));
#34487=CARTESIAN_POINT('Ctrl Pts',(157.023615671966,2.44051566432356,-1.78710744205035));
#34488=CARTESIAN_POINT('Ctrl Pts',(157.128847015899,3.38388779517831,0.133215779263953));
#34489=CARTESIAN_POINT('Ctrl Pts',(157.286694031797,1.73842129201381,2.91023290985255));
#34490=CARTESIAN_POINT('Ctrl Pts',(157.444541047695,-1.48379950765357,3.04509876769309));
#34491=CARTESIAN_POINT('Ctrl Pts',(157.556446406461,-2.81469700920609,1.18796503211997));
#34492=CARTESIAN_POINT('Ctrl Pts',(157.615736093261,-2.87579990686974,0.122127760897206));
#34493=CARTESIAN_POINT('Ctrl Pts',(157.622410108095,-2.87487623080957,0.00203977944324927));
#34494=CARTESIAN_POINT('Ctrl Pts',(156.641910346562,1.99840595662821,-2.80245207497164));
#34495=CARTESIAN_POINT('Ctrl Pts',(156.694526018528,2.92487984561336,-2.14179102212308));
#34496=CARTESIAN_POINT('Ctrl Pts',(156.79975736246,4.0554811250013,0.159654844089943));
#34497=CARTESIAN_POINT('Ctrl Pts',(156.957604378359,2.08344223088848,3.48782091772715));
#34498=CARTESIAN_POINT('Ctrl Pts',(157.115451394257,-1.77828617874074,3.64945332813361));
#34499=CARTESIAN_POINT('Ctrl Pts',(157.273298410156,-4.02815155478086,0.509992261095901));
#34500=CARTESIAN_POINT('Ctrl Pts',(157.431145426054,-2.63083191649386,-3.09321993275373));
#34501=CARTESIAN_POINT('Ctrl Pts',(157.588992441953,1.14932790535007,-3.89426644772928));
#34502=CARTESIAN_POINT('Ctrl Pts',(157.746839457851,3.8884790677076,-1.16912401597452));
#34503=CARTESIAN_POINT('Ctrl Pts',(157.90468647375,3.1063037483826,2.61500941800772));
#34504=CARTESIAN_POINT('Ctrl Pts',(158.062533489648,-0.488988477053649,
4.03087189984344));
#34505=CARTESIAN_POINT('Ctrl Pts',(158.220380505547,-3.64143065256987,1.79642633305765));
#34506=CARTESIAN_POINT('Ctrl Pts',(158.378227521445,-3.49619755012992,-2.06489389097847));
#34507=CARTESIAN_POINT('Ctrl Pts',(158.536074537343,-0.184796791687261,
-4.05622887980389));
#34508=CARTESIAN_POINT('Ctrl Pts',(158.693921553242,3.29395367989886,-2.37424292862959));
#34509=CARTESIAN_POINT('Ctrl Pts',(158.85176856914,3.78969536832349,1.45786484210508));
#34510=CARTESIAN_POINT('Ctrl Pts',(159.009615585039,0.853481851318687,3.96972605671494));
#34511=CARTESIAN_POINT('Ctrl Pts',(159.167462600937,-2.85564597043241,2.88659742752771));
#34512=CARTESIAN_POINT('Ctrl Pts',(159.325309616835,-3.97869609633737,-0.810639154257264));
#34513=CARTESIAN_POINT('Ctrl Pts',(159.483156632734,-1.49863219029163,-3.77375933554359));
#34514=CARTESIAN_POINT('Ctrl Pts',(159.641003648632,2.33859553970342,-3.31935674108112));
#34515=CARTESIAN_POINT('Ctrl Pts',(159.798850664531,4.057987188022,0.1410610164337));
#34516=CARTESIAN_POINT('Ctrl Pts',(159.956697680429,2.10245872402191,3.47373365282519));
#34517=CARTESIAN_POINT('Ctrl Pts',(160.114544696328,-1.75705993367321,3.66058719404933));
#34518=CARTESIAN_POINT('Ctrl Pts',(160.272391712226,-4.02538212767037,0.532406737005837));
#34519=CARTESIAN_POINT('Ctrl Pts',(160.430238728124,-2.64831141563203,-3.07792216409928));
#34520=CARTESIAN_POINT('Ctrl Pts',(160.588085744023,1.12707462054498,-3.90087951709366));
#34521=CARTESIAN_POINT('Ctrl Pts',(160.745932759921,3.8817799626603,-1.1911937404532));
#34522=CARTESIAN_POINT('Ctrl Pts',(160.90377977582,3.12113876473172,2.59723911426476));
#34523=CARTESIAN_POINT('Ctrl Pts',(161.061626791718,-0.46601100979089,4.03360780749621));
#34524=CARTESIAN_POINT('Ctrl Pts',(161.219473807617,-3.63114042085755,1.81713440607874));
#34525=CARTESIAN_POINT('Ctrl Pts',(161.377320823515,-3.50790288757611,-2.04493900570317));
#34526=CARTESIAN_POINT('Ctrl Pts',(161.535167839414,-0.207902529827338,
-4.05511217401782));
#34527=CARTESIAN_POINT('Ctrl Pts',(161.693014855312,3.28037471273009,-2.39296885684481));
#34528=CARTESIAN_POINT('Ctrl Pts',(161.850861871211,3.79793903314098,1.43625112925684));
#34529=CARTESIAN_POINT('Ctrl Pts',(162.008708887109,0.876083302092013,3.96479964860146));
#34530=CARTESIAN_POINT('Ctrl Pts',(162.166555903007,-2.83915495818497,2.902818859172));
#34531=CARTESIAN_POINT('Ctrl Pts',(162.324402918906,-3.98324965686799,-0.787959628922847));
#34532=CARTESIAN_POINT('Ctrl Pts',(162.482249934804,-1.52010668789534,-3.76516053617476));
#34533=CARTESIAN_POINT('Ctrl Pts',(162.640096950703,2.31964748443918,-3.33262565459826));
#34534=CARTESIAN_POINT('Ctrl Pts',(162.797943966601,4.05872494746307,0.117940690995252));
#34535=CARTESIAN_POINT('Ctrl Pts',(162.9557909825,2.12221419123008,3.46169974612087));
#34536=CARTESIAN_POINT('Ctrl Pts',(163.113637998398,-1.73617734800614,3.67053762029787));
#34537=CARTESIAN_POINT('Ctrl Pts',(163.271485014297,-4.02228372639134,0.555330379286925));
#34538=CARTESIAN_POINT('Ctrl Pts',(163.429332030195,-2.66580311733514,-3.06278499822593));
#34539=CARTESIAN_POINT('Ctrl Pts',(163.587179046093,1.10483333124399,-3.90723706932711));
#34540=CARTESIAN_POINT('Ctrl Pts',(163.745026061992,3.87493083492589,-1.21328860140205));
#34541=CARTESIAN_POINT('Ctrl Pts',(163.90287307789,3.13588438043163,2.57941608863644));
#34542=CARTESIAN_POINT('Ctrl Pts',(164.060720093789,-0.443024305394836,
4.03619717934853));
#34543=CARTESIAN_POINT('Ctrl Pts',(164.218567109687,-3.62072942635015,1.83779123594432));
#34544=CARTESIAN_POINT('Ctrl Pts',(164.376414125586,-3.51949581731641,-2.02492157814664));
#34545=CARTESIAN_POINT('Ctrl Pts',(164.534261141484,-0.231000806906372,
-4.05386196520801));
#34546=CARTESIAN_POINT('Ctrl Pts',(164.692108157383,3.26668892733796,-2.41161805801814));
#34547=CARTESIAN_POINT('Ctrl Pts',(164.849955173281,3.80605960997831,1.41459126642409));
#34548=CARTESIAN_POINT('Ctrl Pts',(165.00780218918,0.898656232954932,3.95974433274711));
#34549=CARTESIAN_POINT('Ctrl Pts',(165.165649205078,-2.82257175789836,2.91894619293781));
#34550=CARTESIAN_POINT('Ctrl Pts',(165.323496220976,-3.98767396155753,-0.765254586440123));
#34551=CARTESIAN_POINT('Ctrl Pts',(165.481343236875,-1.54153183970511,-3.75643951008491));
#34552=CARTESIAN_POINT('Ctrl Pts',(165.639190252773,2.30062413944776,-3.34578642096919));
#34553=CARTESIAN_POINT('Ctrl Pts',(165.797037268672,4.05933098288678,0.0948165445851432));
#34554=CARTESIAN_POINT('Ctrl Pts',(165.95488428457,2.14190078035788,3.44955348601147));
#34555=CARTESIAN_POINT('Ctrl Pts',(166.112731300469,-1.71523841378955,3.68036892031387));
#34556=CARTESIAN_POINT('Ctrl Pts',(166.270578316367,-4.01905478154481,0.578235997403664));
#34557=CARTESIAN_POINT('Ctrl Pts',(166.428425332266,-2.68320829980646,-3.04754842875405));
#34558=CARTESIAN_POINT('Ctrl Pts',(166.586272348164,1.08255618431966,-3.91346781174227));
#34559=CARTESIAN_POINT('Ctrl Pts',(166.744119364062,3.86795594571282,-1.23534408477008));
#34560=CARTESIAN_POINT('Ctrl Pts',(166.901966379961,3.15052822047051,2.56150934758601));
#34561=CARTESIAN_POINT('Ctrl Pts',(167.059813395859,-0.420023222562997,
4.03865555578329));
#34562=CARTESIAN_POINT('Ctrl Pts',(167.217660411758,-3.61020092047943,1.85838841998152));
#34563=CARTESIAN_POINT('Ctrl Pts',(167.375507427656,-3.53097452123983,-2.00483843142192));
#34564=CARTESIAN_POINT('Ctrl Pts',(167.533354443555,-0.254091586817575,
-4.05248018764552));
#34565=CARTESIAN_POINT('Ctrl Pts',(167.691201459453,3.25289712102133,-2.43018898973018));
#34566=CARTESIAN_POINT('Ctrl Pts',(167.849048475351,3.81405666052524,1.3928854927992));
#34567=CARTESIAN_POINT('Ctrl Pts',(168.00689549125,0.921199997783791,3.95456050274001));
#34568=CARTESIAN_POINT('Ctrl Pts',(168.164742507148,-2.80589695058484,2.93497879182709));
#34569=CARTESIAN_POINT('Ctrl Pts',(168.322589523047,-3.99196884562836,-0.74252470749716));
#34570=CARTESIAN_POINT('Ctrl Pts',(168.480436538945,-1.56290696085737,-3.74759656812794));
#34571=CARTESIAN_POINT('Ctrl Pts',(168.638283554844,2.28152612734524,-3.35883859930508));
#34572=CARTESIAN_POINT('Ctrl Pts',(168.796130570742,4.05980527201056,0.0716893209138078));
#34573=CARTESIAN_POINT('Ctrl Pts',(168.953977586641,2.16151785383815,3.43729527002625));
#34574=CARTESIAN_POINT('Ctrl Pts',(169.111824602539,-1.69424381141843,3.69008077345576));
#34575=CARTESIAN_POINT('Ctrl Pts',(169.269671618438,-4.01569539723208,0.601122848567297));
#34576=CARTESIAN_POINT('Ctrl Pts',(169.427518634336,-2.70052639908684,-3.03221295017554));
#34577=CARTESIAN_POINT('Ctrl Pts',(169.585365650234,1.0602439044225,-3.91957154277003));
#34578=CARTESIAN_POINT('Ctrl Pts',(169.743212666133,3.86085551819054,-1.25735947311964));
#34579=CARTESIAN_POINT('Ctrl Pts',(169.901059682031,3.16506981599229,2.54351946884677));
#34580=CARTESIAN_POINT('Ctrl Pts',(170.05890669793,-0.397008520727738,4.0409828640259));
#34581=CARTESIAN_POINT('Ctrl Pts',(170.216753713828,-3.59955521883953,1.87892527549814));
#34582=CARTESIAN_POINT('Ctrl Pts',(170.374600729727,-3.54233867955676,-1.98469018860405));
#34583=CARTESIAN_POINT('Ctrl Pts',(170.532447745625,-0.27717401355112,-4.050966944233));
#34584=CARTESIAN_POINT('Ctrl Pts',(170.690294761523,3.23899952600311,-2.44868093193939));
#34585=CARTESIAN_POINT('Ctrl Pts',(170.848141777422,3.82193036047487,1.37113427578011));
#34586=CARTESIAN_POINT('Ctrl Pts',(171.00598879332,0.943712985438493,3.94924880585936));
#34587=CARTESIAN_POINT('Ctrl Pts',(171.163835809219,-2.78912930028193,2.950915167517));
#34588=CARTESIAN_POINT('Ctrl Pts',(171.321682825117,-3.99613776073605,-0.719768773811534));
#34589=CARTESIAN_POINT('Ctrl Pts',(171.479529841016,-1.58422410125613,-3.73863594972519));
#34590=CARTESIAN_POINT('Ctrl Pts',(171.637376856914,2.26233940515993,-3.37177377940741));
#34591=CARTESIAN_POINT('Ctrl Pts',(171.795223872812,4.06017742829736,0.0485436322247005));
#34592=CARTESIAN_POINT('Ctrl Pts',(171.953070888711,2.1810049044929,3.42495810650385));
#34593=CARTESIAN_POINT('Ctrl Pts',(172.110917904609,-1.67307324287401,3.69960696884215));
#34594=CARTESIAN_POINT('Ctrl Pts',(172.268764920508,-4.01245014574975,0.624123347664986));
#34595=CARTESIAN_POINT('Ctrl Pts',(172.426611936406,-2.71726283523924,-3.01704818305721));
#34596=CARTESIAN_POINT('Ctrl Pts',(172.584458952305,1.03689846178847,-3.92500355511514));
#34597=CARTESIAN_POINT('Ctrl Pts',(172.742305968203,3.85565576660502,-1.28044714573858));
#34598=CARTESIAN_POINT('Ctrl Pts',(172.900152984102,3.17531601965564,2.52780240521317));
#34599=CARTESIAN_POINT('Ctrl Pts',(173.005384328034,0.81604732941719,3.53217463467951));
#34600=CARTESIAN_POINT('Ctrl Pts',(173.058,-0.317020535431506,3.42736954239176));
#34601=CARTESIAN_POINT('Ctrl Pts',(156.751606897708,1.8880930188713,-2.64775541772451));
#34602=CARTESIAN_POINT('Ctrl Pts',(156.804222569674,2.76342511851676,-2.02356316209884));
#34603=CARTESIAN_POINT('Ctrl Pts',(156.909453913606,3.83161668172697,0.150841822481279));
#34604=CARTESIAN_POINT('Ctrl Pts',(157.067300929505,1.96843525126359,3.29529158176895));
#34605=CARTESIAN_POINT('Ctrl Pts',(157.225147945403,-1.68012395504502,3.44800180798677));
#34606=CARTESIAN_POINT('Ctrl Pts',(157.382994961302,-3.80579571648674,0.481840451215513));
#34607=CARTESIAN_POINT('Ctrl Pts',(157.5408419772,-2.48560877177163,-2.92247275459476));
#34608=CARTESIAN_POINT('Ctrl Pts',(157.698688993099,1.08588447071426,-3.67930112958036));
#34609=CARTESIAN_POINT('Ctrl Pts',(157.856536008997,3.67383321562612,-1.10458782683006));
#34610=CARTESIAN_POINT('Ctrl Pts',(158.014383024896,2.93483433751894,2.47065968255699));
#34611=CARTESIAN_POINT('Ctrl Pts',(158.172230040794,-0.461996085815962,
3.80836589723732));
#34612=CARTESIAN_POINT('Ctrl Pts',(158.330077056692,-3.44042198784348,1.69726276441122));
#34613=CARTESIAN_POINT('Ctrl Pts',(158.487924072591,-3.30320582016923,-1.95091078833877));
#34614=CARTESIAN_POINT('Ctrl Pts',(158.645771088489,-0.174595922884049,
-3.83232316011687));
#34615=CARTESIAN_POINT('Ctrl Pts',(158.803618104388,3.11212590558719,-2.24318361531184));
#34616=CARTESIAN_POINT('Ctrl Pts',(158.961465120286,3.58050242236722,1.37739002513823));
#34617=CARTESIAN_POINT('Ctrl Pts',(159.119312136185,0.806369256388234,3.75059533307292));
#34618=CARTESIAN_POINT('Ctrl Pts',(159.277159152083,-2.6980129854289,2.72725590770484));
#34619=CARTESIAN_POINT('Ctrl Pts',(159.435006167981,-3.7590702223385,-0.765891496119899));
#34620=CARTESIAN_POINT('Ctrl Pts',(159.59285318388,-1.4159069967543,-3.56544606600458));
#34621=CARTESIAN_POINT('Ctrl Pts',(159.750700199778,2.20950397882498,-3.13612670598366));
#34622=CARTESIAN_POINT('Ctrl Pts',(159.908547215677,3.83398440890398,0.13327438275493));
#34623=CARTESIAN_POINT('Ctrl Pts',(160.066394231575,1.98640202513631,3.28198194043799));
#34624=CARTESIAN_POINT('Ctrl Pts',(160.224241247473,-1.66006940857215,3.45852107932842));
#34625=CARTESIAN_POINT('Ctrl Pts',(160.382088263372,-3.8031791630401,0.503017637635941));
#34626=CARTESIAN_POINT('Ctrl Pts',(160.53993527927,-2.50212339443211,-2.90801942988115));
#34627=CARTESIAN_POINT('Ctrl Pts',(160.697782295169,1.06485957757476,-3.68554915444177));
#34628=CARTESIAN_POINT('Ctrl Pts',(160.855629311067,3.66750390429149,-1.1254392922585));
#34629=CARTESIAN_POINT('Ctrl Pts',(161.013476326966,2.94885045406958,2.45387030784109));
#34630=CARTESIAN_POINT('Ctrl Pts',(161.171323342864,-0.440286985427089,
3.81095078151588));
#34631=CARTESIAN_POINT('Ctrl Pts',(161.329170358763,-3.43069978170505,1.71682774217548));
#34632=CARTESIAN_POINT('Ctrl Pts',(161.487017374661,-3.31426501754721,-1.93205742200662));
#34633=CARTESIAN_POINT('Ctrl Pts',(161.64486439056,-0.196426213538184,-3.83126809700928));
#34634=CARTESIAN_POINT('Ctrl Pts',(161.802711406458,3.09929650371827,-2.26087586358491));
#34635=CARTESIAN_POINT('Ctrl Pts',(161.960558422357,3.58829103305475,1.35696939928626));
#34636=CARTESIAN_POINT('Ctrl Pts',(162.118405438255,0.827723096572676,3.74594086497732));
#34637=CARTESIAN_POINT('Ctrl Pts',(162.276252454153,-2.68243228472329,2.7425819087819));
#34638=CARTESIAN_POINT('Ctrl Pts',(162.434099470052,-3.76337242421112,-0.74446389112643));
#34639=CARTESIAN_POINT('Ctrl Pts',(162.59194648595,-1.43619609210796,-3.55732192435803));
#34640=CARTESIAN_POINT('Ctrl Pts',(162.749793501849,2.19160186501925,-3.14866316930665));
#34641=CARTESIAN_POINT('Ctrl Pts',(162.907640517747,3.83468144368097,0.111430310028073));
#34642=CARTESIAN_POINT('Ctrl Pts',(163.065487533646,2.00506698137134,3.27061231097766));
#34643=CARTESIAN_POINT('Ctrl Pts',(163.223334549544,-1.64033955134109,3.46792223742261));
#34644=CARTESIAN_POINT('Ctrl Pts',(163.381181565443,-3.80025179495196,0.524675884207151));
#34645=CARTESIAN_POINT('Ctrl Pts',(163.539028581341,-2.51864954607026,-2.89371784260046));
#34646=CARTESIAN_POINT('Ctrl Pts',(163.69687559724,1.04384601778196,-3.69155576683664));
#34647=CARTESIAN_POINT('Ctrl Pts',(163.854722613138,3.66103285159181,-1.14631450661227));
#34648=CARTESIAN_POINT('Ctrl Pts',(164.012569629036,2.96278210492842,2.43703112151242));
#34649=CARTESIAN_POINT('Ctrl Pts',(164.170416644935,-0.418569157798979,
3.81339721883829));
#34650=CARTESIAN_POINT('Ctrl Pts',(164.328263660833,-3.42086347893396,1.73634430543023));
#34651=CARTESIAN_POINT('Ctrl Pts',(164.486110676732,-3.32521801217691,-1.91314496575622));
#34652=CARTESIAN_POINT('Ctrl Pts',(164.64395769263,-0.218249454985314,-3.83008690030693));
#34653=CARTESIAN_POINT('Ctrl Pts',(164.801804708529,3.08636618004157,-2.27849562018446));
#34654=CARTESIAN_POINT('Ctrl Pts',(164.959651724427,3.59596335027584,1.33650517095037));
#34655=CARTESIAN_POINT('Ctrl Pts',(165.117498740325,0.849049991159028,3.74116460490808));
#34656=CARTESIAN_POINT('Ctrl Pts',(165.275345756224,-2.66676448480114,2.75781900622711));
#34657=CARTESIAN_POINT('Ctrl Pts',(165.433192772122,-3.76755250522518,-0.723012177543099));
#34658=CARTESIAN_POINT('Ctrl Pts',(165.591039788021,-1.45643856557843,-3.54908230296227));
#34659=CARTESIAN_POINT('Ctrl Pts',(165.748886803919,2.17362861751428,-3.16109745525618));
#34660=CARTESIAN_POINT('Ctrl Pts',(165.906733819818,3.83525402566757,0.0895826272489707));
#34661=CARTESIAN_POINT('Ctrl Pts',(166.064580835716,2.02366686162806,3.25913653007244));
#34662=CARTESIAN_POINT('Ctrl Pts',(166.222427851615,-1.62055645602664,3.47721084510769));
#34663=CARTESIAN_POINT('Ctrl Pts',(166.380274867513,-3.79720108936192,0.546317101556261));
#34664=CARTESIAN_POINT('Ctrl Pts',(166.538121883412,-2.53509395437843,-2.87932233884608));
#34665=CARTESIAN_POINT('Ctrl Pts',(166.69596889931,1.0227985797233,-3.69744256937415));
#34666=CARTESIAN_POINT('Ctrl Pts',(166.853815915209,3.65444297950556,-1.16715251704597));
#34667=CARTESIAN_POINT('Ctrl Pts',(167.011662931107,2.97661759819002,2.42011284089185));
#34668=CARTESIAN_POINT('Ctrl Pts',(167.169509947005,-0.396837745431416,
3.81571989175109));
#34669=CARTESIAN_POINT('Ctrl Pts',(167.327356962904,-3.41091615148145,1.75580451533406));
#34670=CARTESIAN_POINT('Ctrl Pts',(167.485203978802,-3.33606308630793,-1.89417041806629));
#34671=CARTESIAN_POINT('Ctrl Pts',(167.643050994701,-0.240065613111764,
-3.8287813975082));
#34672=CARTESIAN_POINT('Ctrl Pts',(167.800898010599,3.07333568784469,-2.29604142783338));
#34673=CARTESIAN_POINT('Ctrl Pts',(167.958745026498,3.60351895991518,1.31599756611942));
#34674=CARTESIAN_POINT('Ctrl Pts',(168.116592042396,0.870349329689956,3.73626692472705));
#34675=CARTESIAN_POINT('Ctrl Pts',(168.274439058294,-2.65101013460254,2.77296659820502));
#34676=CARTESIAN_POINT('Ctrl Pts',(168.432286074193,-3.77161030969884,-0.701536998483682));
#34677=CARTESIAN_POINT('Ctrl Pts',(168.590133090091,-1.47663377010695,-3.54072749551193));
#34678=CARTESIAN_POINT('Ctrl Pts',(168.74798010599,2.15558482455746,-3.17342914728068));
#34679=CARTESIAN_POINT('Ctrl Pts',(168.905827121888,3.83570213381125,0.0677320370748901));
#34680=CARTESIAN_POINT('Ctrl Pts',(169.063674137787,2.04220106353329,3.24755497330779));
#34681=CARTESIAN_POINT('Ctrl Pts',(169.221521153685,-1.60072076546566,3.48638659944164));
#34682=CARTESIAN_POINT('Ctrl Pts',(169.379368169583,-3.79402714462485,0.567940587896798));
#34683=CARTESIAN_POINT('Ctrl Pts',(169.537215185482,-2.55145608652828,-2.86483338581374));
#34684=CARTESIAN_POINT('Ctrl Pts',(169.69506220138,1.00171794804823,-3.70320937161189));
#34685=CARTESIAN_POINT('Ctrl Pts',(169.852909217279,3.64773449888311,-1.18795264572487));
#34686=CARTESIAN_POINT('Ctrl Pts',(170.010756233177,2.99035649087939,2.40311601182154));
#34687=CARTESIAN_POINT('Ctrl Pts',(170.168603249076,-0.375093465835755,
3.81791873149687));
#34688=CARTESIAN_POINT('Ctrl Pts',(170.326450264974,-3.40085809752068,1.77520772687968));
#34689=CARTESIAN_POINT('Ctrl Pts',(170.484297280873,-3.34679993780318,-1.87513436761779));
#34690=CARTESIAN_POINT('Ctrl Pts',(170.642144296771,-0.26187387915984,-3.82735168583548));
#34691=CARTESIAN_POINT('Ctrl Pts',(170.79999131267,3.06020524653171,-2.31351260623673));
#34692=CARTESIAN_POINT('Ctrl Pts',(170.957838328568,3.61095802796753,1.29544702639075));
#34693=CARTESIAN_POINT('Ctrl Pts',(171.115685344466,0.891619589961043,3.73124843598334));
#34694=CARTESIAN_POINT('Ctrl Pts',(171.273532360365,-2.63516806639073,2.78802327854887));
#34695=CARTESIAN_POINT('Ctrl Pts',(171.431379376263,-3.77554909875469,-0.680037202915507));
#34696=CARTESIAN_POINT('Ctrl Pts',(171.589226392161,-1.49677419444651,-3.53226150741033));
#34697=CARTESIAN_POINT('Ctrl Pts',(171.74707340806,2.13745721835565,-3.18565029942849));
#34698=CARTESIAN_POINT('Ctrl Pts',(171.904920423959,3.83605374689803,0.0458640011606042));
#34699=CARTESIAN_POINT('Ctrl Pts',(172.062767439857,2.06061241993342,3.2358988269467));
#34700=CARTESIAN_POINT('Ctrl Pts',(172.220614455755,-1.58071882214594,3.49538694441449));
#34701=CARTESIAN_POINT('Ctrl Pts',(172.378461471654,-3.79096103253289,0.589671448752604));
#34702=CARTESIAN_POINT('Ctrl Pts',(172.536308487552,-2.5672686636252,-2.85050572088963));
#34703=CARTESIAN_POINT('Ctrl Pts',(172.694155503451,0.979661184699643,-3.7083415343505));
#34704=CARTESIAN_POINT('Ctrl Pts',(172.852002519349,3.64282177600219,-1.20976586808304));
#34705=CARTESIAN_POINT('Ctrl Pts',(173.009849535247,3.00003709933762,2.38826653740653));
#34706=CARTESIAN_POINT('Ctrl Pts',(173.11508087918,0.77100113749699,3.33719695292788));
#34707=CARTESIAN_POINT('Ctrl Pts',(173.167696551146,-0.29952085450997,3.23817715045265));
#34708=CARTESIAN_POINT('Ctrl Pts',(156.861303448854,1.77778008111438,-2.49305876047737));
#34709=CARTESIAN_POINT('Ctrl Pts',(156.91391912082,2.60197039142016,-1.90533530207459));
#34710=CARTESIAN_POINT('Ctrl Pts',(157.019150464753,3.60775223845264,0.142028800872616));
#34711=CARTESIAN_POINT('Ctrl Pts',(157.176997480651,1.8534282716387,3.10276224581075));
#34712=CARTESIAN_POINT('Ctrl Pts',(157.334844496549,-1.5819617313493,3.24655028783993));
#34713=CARTESIAN_POINT('Ctrl Pts',(157.492691512448,-3.58343987819263,0.453688641335127));
#34714=CARTESIAN_POINT('Ctrl Pts',(157.650538528346,-2.34038562704942,-2.7517255764358));
#34715=CARTESIAN_POINT('Ctrl Pts',(157.808385544245,1.02244103607846,-3.46433581143144));
#34716=CARTESIAN_POINT('Ctrl Pts',(157.966232560143,3.45918736354465,-1.0400516376856));
#34717=CARTESIAN_POINT('Ctrl Pts',(158.124079576042,2.76336492665527,2.32630994710626));
#34718=CARTESIAN_POINT('Ctrl Pts',(158.28192659194,-0.435003694578273,3.5858598946312));
#34719=CARTESIAN_POINT('Ctrl Pts',(158.439773607838,-3.23941332311708,1.59809919576479));
#34720=CARTESIAN_POINT('Ctrl Pts',(158.597620623737,-3.11021409020853,-1.83692768569907));
#34721=CARTESIAN_POINT('Ctrl Pts',(158.755467639635,-0.164395054080841,
-3.60841744042984));
#34722=CARTESIAN_POINT('Ctrl Pts',(158.913314655534,2.93029813127553,-2.1121243019941));
#34723=CARTESIAN_POINT('Ctrl Pts',(159.071161671432,3.37130947641095,1.29691520817138));
#34724=CARTESIAN_POINT('Ctrl Pts',(159.229008687331,0.759256661457781,3.5314646094309));
#34725=CARTESIAN_POINT('Ctrl Pts',(159.386855703229,-2.54038000042538,2.56791438788198));
#34726=CARTESIAN_POINT('Ctrl Pts',(159.544702719127,-3.53944434833963,-0.721143837982535));
#34727=CARTESIAN_POINT('Ctrl Pts',(159.702549735026,-1.33318180321698,-3.35713279646557));
#34728=CARTESIAN_POINT('Ctrl Pts',(159.860396750924,2.08041241794654,-2.9528966708862));
#34729=CARTESIAN_POINT('Ctrl Pts',(160.018243766823,3.60998162978598,0.125487749076156));
#34730=CARTESIAN_POINT('Ctrl Pts',(160.176090782721,1.87034532625072,3.09023022805079));
#34731=CARTESIAN_POINT('Ctrl Pts',(160.33393779862,-1.56307888347109,3.2564549646075));
#34732=CARTESIAN_POINT('Ctrl Pts',(160.491784814518,-3.58097619840984,0.473628538266046));
#34733=CARTESIAN_POINT('Ctrl Pts',(160.649631830416,-2.35593537323219,-2.73811669566301));
#34734=CARTESIAN_POINT('Ctrl Pts',(160.807478846315,1.00264453460455,-3.47021879178988));
#34735=CARTESIAN_POINT('Ctrl Pts',(160.965325862213,3.45322784592268,-1.05968484406379));
#34736=CARTESIAN_POINT('Ctrl Pts',(161.123172878112,2.77656214340745,2.31050150141743));
#34737=CARTESIAN_POINT('Ctrl Pts',(161.28101989401,-0.414562961063291,3.58829375553555));
#34738=CARTESIAN_POINT('Ctrl Pts',(161.438866909909,-3.23025914255255,1.61652107827222));
#34739=CARTESIAN_POINT('Ctrl Pts',(161.596713925807,-3.1206271475183,-1.81917583831006));
#34740=CARTESIAN_POINT('Ctrl Pts',(161.754560941706,-0.184949897249031,
-3.60742402000075));
#34741=CARTESIAN_POINT('Ctrl Pts',(161.912407957604,2.91821829470645,-2.12878287032501));
#34742=CARTESIAN_POINT('Ctrl Pts',(162.070254973503,3.37864303296851,1.27768766931568));
#34743=CARTESIAN_POINT('Ctrl Pts',(162.228101989401,0.77936289105334,3.52708208135319));
#34744=CARTESIAN_POINT('Ctrl Pts',(162.3859490053,-2.52570961126161,2.5823449583918));
#34745=CARTESIAN_POINT('Ctrl Pts',(162.543796021198,-3.54349519155426,-0.700968153330012));
#34746=CARTESIAN_POINT('Ctrl Pts',(162.701643037096,-1.35228549632057,-3.3494833125413));
#34747=CARTESIAN_POINT('Ctrl Pts',(162.859490052995,2.06355624559932,-2.96470068401505));
#34748=CARTESIAN_POINT('Ctrl Pts',(163.017337068893,3.61063793989887,0.104919929060897));
#34749=CARTESIAN_POINT('Ctrl Pts',(163.175184084792,1.88791977151261,3.07952487583444));
#34750=CARTESIAN_POINT('Ctrl Pts',(163.33303110069,-1.54450175467604,3.26530685454736));
#34751=CARTESIAN_POINT('Ctrl Pts',(163.490878116589,-3.57821986351258,0.494021389127376));
#34752=CARTESIAN_POINT('Ctrl Pts',(163.648725132487,-2.37149597480538,-2.72465068697498));
#34753=CARTESIAN_POINT('Ctrl Pts',(163.806572148385,0.982858704319936,-3.47587446434618));
#34754=CARTESIAN_POINT('Ctrl Pts',(163.964419164284,3.44713486825773,-1.07934041182248));
#34755=CARTESIAN_POINT('Ctrl Pts',(164.122266180182,2.78967982942521,2.29464615438841));
#34756=CARTESIAN_POINT('Ctrl Pts',(164.280113196081,-0.394114010203119,
3.59059725832805));
#34757=CARTESIAN_POINT('Ctrl Pts',(164.437960211979,-3.22099753151778,1.63489737491615));
#34758=CARTESIAN_POINT('Ctrl Pts',(164.595807227878,-3.13094020703742,-1.80136835336581));
#34759=CARTESIAN_POINT('Ctrl Pts',(164.753654243776,-0.205498103064254,
-3.60631183540585));
#34760=CARTESIAN_POINT('Ctrl Pts',(164.911501259675,2.90604343274518,-2.14537318235079));
#34761=CARTESIAN_POINT('Ctrl Pts',(165.069348275573,3.38586709057337,1.25841907547666));
#34762=CARTESIAN_POINT('Ctrl Pts',(165.227195291471,0.799443749363122,3.52258487706905));
#34763=CARTESIAN_POINT('Ctrl Pts',(165.38504230737,-2.51095721170392,2.59669181951641));
#34764=CARTESIAN_POINT('Ctrl Pts',(165.542889323268,-3.54743104889283,-0.680769768646074));
#34765=CARTESIAN_POINT('Ctrl Pts',(165.700736339167,-1.37134529145175,-3.34172509583964));
#34766=CARTESIAN_POINT('Ctrl Pts',(165.858583355065,2.04663309558081,-2.97640848954317));
#34767=CARTESIAN_POINT('Ctrl Pts',(166.016430370964,3.61117706844838,0.0843487099127957));
#34768=CARTESIAN_POINT('Ctrl Pts',(166.174277386862,1.90543294289823,3.06871957413341));
#34769=CARTESIAN_POINT('Ctrl Pts',(166.332124402761,-1.52587449826372,3.27405276990151));
#34770=CARTESIAN_POINT('Ctrl Pts',(166.489971418659,-3.57534739717903,0.514398205708856));
#34771=CARTESIAN_POINT('Ctrl Pts',(166.647818434558,-2.3869796089504,-2.71109624893811));
#34772=CARTESIAN_POINT('Ctrl Pts',(166.805665450456,0.963040975126942,-3.48141732700604));
#34773=CARTESIAN_POINT('Ctrl Pts',(166.963512466355,3.44093001329829,-1.09896094932186));
#34774=CARTESIAN_POINT('Ctrl Pts',(167.121359482253,2.80270697590953,2.27871633419769));
#34775=CARTESIAN_POINT('Ctrl Pts',(167.279206498151,-0.373652268299834,
3.5927842277189));
#34776=CARTESIAN_POINT('Ctrl Pts',(167.43705351405,-3.21163138248347,1.6532206106866));
#34777=CARTESIAN_POINT('Ctrl Pts',(167.594900529948,-3.14115165137603,-1.78350240471065));
#34778=CARTESIAN_POINT('Ctrl Pts',(167.752747545847,-0.226039639405949,
-3.60508260737089));
#34779=CARTESIAN_POINT('Ctrl Pts',(167.910594561745,2.89377425466804,-2.16189386593658));
#34780=CARTESIAN_POINT('Ctrl Pts',(168.068441577644,3.39298125930512,1.23910963943965));
#34781=CARTESIAN_POINT('Ctrl Pts',(168.226288593542,0.819498661596119,3.5179733467141));
#34782=CARTESIAN_POINT('Ctrl Pts',(168.38413560944,-2.49612331862024,2.61095440458294));
#34783=CARTESIAN_POINT('Ctrl Pts',(168.541982625339,-3.55125177376932,-0.660549289470204));
#34784=CARTESIAN_POINT('Ctrl Pts',(168.699829641237,-1.39036057935652,-3.33385842289593));
#34785=CARTESIAN_POINT('Ctrl Pts',(168.857676657136,2.02964352176968,-2.98801969525627));
#34786=CARTESIAN_POINT('Ctrl Pts',(169.015523673034,3.61159899561195,0.0637747532359756));
#34787=CARTESIAN_POINT('Ctrl Pts',(169.173370688933,1.92288427322844,3.05781467658932));
#34788=CARTESIAN_POINT('Ctrl Pts',(169.331217704831,-1.50719771951289,3.28269242542751));
#34789=CARTESIAN_POINT('Ctrl Pts',(169.48906472073,-3.57235889201762,0.5347583272263));
#34790=CARTESIAN_POINT('Ctrl Pts',(169.646911736628,-2.40238577396973,-2.69745382145195));
#34791=CARTESIAN_POINT('Ctrl Pts',(169.804758752526,0.943191991673975,-3.48684720045375));
#34792=CARTESIAN_POINT('Ctrl Pts',(169.962605768425,3.43461347957567,-1.1185458183301));
#34793=CARTESIAN_POINT('Ctrl Pts',(170.120452784323,2.8156431657665,2.26271255479631));
#34794=CARTESIAN_POINT('Ctrl Pts',(170.278299800222,-0.353178410943777,
3.59485459896784));
#34795=CARTESIAN_POINT('Ctrl Pts',(170.43614681612,-3.20216097620183,1.67149017826124));
#34796=CARTESIAN_POINT('Ctrl Pts',(170.593993832019,-3.15126119604961,-1.76557854663153));
#34797=CARTESIAN_POINT('Ctrl Pts',(170.751840847917,-0.24657374476856,-3.60373642743796));
#34798=CARTESIAN_POINT('Ctrl Pts',(170.909687863816,2.88141096706031,-2.17834428053408));
#34799=CARTESIAN_POINT('Ctrl Pts',(171.067534879714,3.3999856954602,1.2197597770014));
#34800=CARTESIAN_POINT('Ctrl Pts',(171.225381895613,0.839526194483593,3.51324806610732));
#34801=CARTESIAN_POINT('Ctrl Pts',(171.383228911511,-2.48120683249953,2.62513138958075));
#34802=CARTESIAN_POINT('Ctrl Pts',(171.541075927409,-3.55496043677332,-0.640305632019483));
#34803=CARTESIAN_POINT('Ctrl Pts',(171.698922943308,-1.40932428763688,-3.32588706509546));
#34804=CARTESIAN_POINT('Ctrl Pts',(171.856769959206,2.01257503155137,-2.99952681944957));
#34805=CARTESIAN_POINT('Ctrl Pts',(172.014616975104,3.61193006549869,0.0431843700965086));
#34806=CARTESIAN_POINT('Ctrl Pts',(172.172463991003,1.94021993537395,3.04683954738956));
#34807=CARTESIAN_POINT('Ctrl Pts',(172.330311006901,-1.48836440141788,3.29116691998682));
#34808=CARTESIAN_POINT('Ctrl Pts',(172.4881580228,-3.56947191931603,0.555219549840223));
#34809=CARTESIAN_POINT('Ctrl Pts',(172.646005038698,-2.41727449201117,-2.68396325872204));
#34810=CARTESIAN_POINT('Ctrl Pts',(172.803852054597,0.922423907610818,-3.49167951358586));
#34811=CARTESIAN_POINT('Ctrl Pts',(172.961699070495,3.42998778539936,-1.13908459042749));
#34812=CARTESIAN_POINT('Ctrl Pts',(173.119546086394,2.82475817901961,2.2487306695999));
#34813=CARTESIAN_POINT('Ctrl Pts',(173.224777430326,0.725954945576791,3.14221927117626));
#34814=CARTESIAN_POINT('Ctrl Pts',(173.277393102292,-0.282021173588434,
3.04898475851353));
#34815=CARTESIAN_POINT('Ctrl Pts',(156.971,1.66746714335746,-2.33836210323023));
#34816=CARTESIAN_POINT('Ctrl Pts',(157.023615671966,2.44051566432356,-1.78710744205035));
#34817=CARTESIAN_POINT('Ctrl Pts',(157.128847015899,3.38388779517831,0.133215779263953));
#34818=CARTESIAN_POINT('Ctrl Pts',(157.286694031797,1.73842129201381,2.91023290985255));
#34819=CARTESIAN_POINT('Ctrl Pts',(157.444541047695,-1.48379950765357,3.04509876769309));
#34820=CARTESIAN_POINT('Ctrl Pts',(157.602388063594,-3.36108403989851,0.425536831454739));
#34821=CARTESIAN_POINT('Ctrl Pts',(157.760235079492,-2.19516248232719,-2.58097839827683));
#34822=CARTESIAN_POINT('Ctrl Pts',(157.918082095391,0.958997601442651,-3.24937049328252));
#34823=CARTESIAN_POINT('Ctrl Pts',(158.075929111289,3.24454151146318,-0.97551544854114));
#34824=CARTESIAN_POINT('Ctrl Pts',(158.233776127188,2.5918955157916,2.18196021165553));
#34825=CARTESIAN_POINT('Ctrl Pts',(158.391623143086,-0.408011303340585,
3.36335389202508));
#34826=CARTESIAN_POINT('Ctrl Pts',(158.549470158985,-3.03840465839069,1.49893562711835));
#34827=CARTESIAN_POINT('Ctrl Pts',(158.707317174883,-2.91722236024783,-1.72294458305937));
#34828=CARTESIAN_POINT('Ctrl Pts',(158.865164190781,-0.154194185277631,
-3.38451172074282));
#34829=CARTESIAN_POINT('Ctrl Pts',(159.02301120668,2.74847035696387,-1.98106498867635));
#34830=CARTESIAN_POINT('Ctrl Pts',(159.180858222578,3.16211653045467,1.21644039120453));
#34831=CARTESIAN_POINT('Ctrl Pts',(159.338705238477,0.71214406652733,3.31233388578888));
#34832=CARTESIAN_POINT('Ctrl Pts',(159.496552254375,-2.38274701542186,2.40857286805911));
#34833=CARTESIAN_POINT('Ctrl Pts',(159.654399270273,-3.31981847434075,-0.676396179845171));
#34834=CARTESIAN_POINT('Ctrl Pts',(159.812246286172,-1.25045660967965,-3.14881952692657));
#34835=CARTESIAN_POINT('Ctrl Pts',(159.97009330207,1.9513208570681,-2.76966663578875));
#34836=CARTESIAN_POINT('Ctrl Pts',(160.127940317969,3.38597885066797,0.117701115397386));
#34837=CARTESIAN_POINT('Ctrl Pts',(160.285787333867,1.75428862736512,2.89847851566358));
#34838=CARTESIAN_POINT('Ctrl Pts',(160.443634349766,-1.46608835837003,3.05438884988658));
#34839=CARTESIAN_POINT('Ctrl Pts',(160.601481365664,-3.35877323377958,0.444239438896151));
#34840=CARTESIAN_POINT('Ctrl Pts',(160.759328381563,-2.20974735203226,-2.56821396144488));
#34841=CARTESIAN_POINT('Ctrl Pts',(160.917175397461,0.940429491634335,-3.25488842913799));
#34842=CARTESIAN_POINT('Ctrl Pts',(161.075022413359,3.23895178755388,-0.993930395869087));
#34843=CARTESIAN_POINT('Ctrl Pts',(161.232869429258,2.60427383274531,2.16713269499377));
#34844=CARTESIAN_POINT('Ctrl Pts',(161.390716445156,-0.388838936699488,
3.36563672955522));
#34845=CARTESIAN_POINT('Ctrl Pts',(161.548563461055,-3.02981850340005,1.51621441436896));
#34846=CARTESIAN_POINT('Ctrl Pts',(161.706410476953,-2.9269892774894,-1.70629425461351));
#34847=CARTESIAN_POINT('Ctrl Pts',(161.864257492852,-0.173473580959878,
-3.38357994299221));
#34848=CARTESIAN_POINT('Ctrl Pts',(162.02210450875,2.73714008569463,-1.99668987706511));
#34849=CARTESIAN_POINT('Ctrl Pts',(162.179951524649,3.16899503288228,1.1984059393451));
#34850=CARTESIAN_POINT('Ctrl Pts',(162.337798540547,0.731002685534005,3.30822329772906));
#34851=CARTESIAN_POINT('Ctrl Pts',(162.495645556446,-2.36898693779993,2.4221080080017));
#34852=CARTESIAN_POINT('Ctrl Pts',(162.653492572344,-3.32361795889739,-0.657472415533592));
#34853=CARTESIAN_POINT('Ctrl Pts',(162.811339588242,-1.26837490053319,-3.14164470072457));
#34854=CARTESIAN_POINT('Ctrl Pts',(162.969186604141,1.9355106261794,-2.78073819872344));
#34855=CARTESIAN_POINT('Ctrl Pts',(163.127033620039,3.38659443611677,0.0984095480937175));
#34856=CARTESIAN_POINT('Ctrl Pts',(163.284880635938,1.77077256165387,2.88843744069124));
#34857=CARTESIAN_POINT('Ctrl Pts',(163.442727651836,-1.44866395801099,3.0626914716721));
#34858=CARTESIAN_POINT('Ctrl Pts',(163.600574667735,-3.3561879320732,0.463366894047598));
#34859=CARTESIAN_POINT('Ctrl Pts',(163.758421683633,-2.22434240354049,-2.55558353134951));
#34860=CARTESIAN_POINT('Ctrl Pts',(163.916268699531,0.921871390857911,-3.26019316185573));
#34861=CARTESIAN_POINT('Ctrl Pts',(164.07411571543,3.23323688492365,-1.01236631703268));
#34862=CARTESIAN_POINT('Ctrl Pts',(164.231962731328,2.61657755392199,2.15226118726438));
#34863=CARTESIAN_POINT('Ctrl Pts',(164.389809747227,-0.369658862607259,
3.36779729781782));
#34864=CARTESIAN_POINT('Ctrl Pts',(164.547656763125,-3.0211315841016,1.53345044440206));
#34865=CARTESIAN_POINT('Ctrl Pts',(164.705503779024,-2.93666240189792,-1.6895917409754));
#34866=CARTESIAN_POINT('Ctrl Pts',(164.863350794922,-0.192746751143198,
-3.38253677050477));
#34867=CARTESIAN_POINT('Ctrl Pts',(165.021197810821,2.72572068544879,-2.01225074451711));
#34868=CARTESIAN_POINT('Ctrl Pts',(165.179044826719,3.1757708308709,1.18033298000295));
#34869=CARTESIAN_POINT('Ctrl Pts',(165.336891842617,0.749837507567218,3.30400514923002));
#34870=CARTESIAN_POINT('Ctrl Pts',(165.494738858516,-2.35514993860669,2.43556463280571));
#34871=CARTESIAN_POINT('Ctrl Pts',(165.652585874414,-3.32730959256048,-0.638527359749053));
#34872=CARTESIAN_POINT('Ctrl Pts',(165.810432890313,-1.28625201732507,-3.13436788871701));
#34873=CARTESIAN_POINT('Ctrl Pts',(165.968279906211,1.91963757364734,-2.79171952383016));
#34874=CARTESIAN_POINT('Ctrl Pts',(166.12612692211,3.38710011122917,0.0791147925766244));
#34875=CARTESIAN_POINT('Ctrl Pts',(166.283973938008,1.78719902416841,2.87830261819438));
#34876=CARTESIAN_POINT('Ctrl Pts',(166.441820953907,-1.43119254050081,3.07089469469534));
#34877=CARTESIAN_POINT('Ctrl Pts',(166.599667969805,-3.35349370499614,0.482479309861451));
#34878=CARTESIAN_POINT('Ctrl Pts',(166.757514985703,-2.23886526352237,-2.54287015903015));
#34879=CARTESIAN_POINT('Ctrl Pts',(166.915362001602,0.903283370530585,-3.26539208463793));
#34880=CARTESIAN_POINT('Ctrl Pts',(167.0732090175,3.22741704709102,-1.03076938159775));
#34881=CARTESIAN_POINT('Ctrl Pts',(167.231056033399,2.62879635362904,2.13731982750353));
#34882=CARTESIAN_POINT('Ctrl Pts',(167.388903049297,-0.350466791168255,
3.36984856368669));
#34883=CARTESIAN_POINT('Ctrl Pts',(167.546750065196,-3.01234661348548,1.55063670603914));
#34884=CARTESIAN_POINT('Ctrl Pts',(167.704597081094,-2.94624021644413,-1.67283439135501));
#34885=CARTESIAN_POINT('Ctrl Pts',(167.862444096993,-0.212013665700137,
-3.38138381723357));
#34886=CARTESIAN_POINT('Ctrl Pts',(168.020291112891,2.7142128214914,-2.02774630403978));
#34887=CARTESIAN_POINT('Ctrl Pts',(168.17813812879,3.18244355869507,1.16222171275988));
#34888=CARTESIAN_POINT('Ctrl Pts',(168.335985144688,0.76864799350228,3.29967976870115));
#34889=CARTESIAN_POINT('Ctrl Pts',(168.493832160587,-2.34123650263794,2.44894221096086));
#34890=CARTESIAN_POINT('Ctrl Pts',(168.651679176485,-3.3308932378398,-0.619561580456727));
#34891=CARTESIAN_POINT('Ctrl Pts',(168.809526192383,-1.30408738860609,-3.12698935027992));
#34892=CARTESIAN_POINT('Ctrl Pts',(168.967373208282,1.9037022189819,-2.80261024323187));
#34893=CARTESIAN_POINT('Ctrl Pts',(169.12522022418,3.38749585741264,0.0598174693970574));
#34894=CARTESIAN_POINT('Ctrl Pts',(169.283067240079,1.80356748292359,2.86807437987086));
#34895=CARTESIAN_POINT('Ctrl Pts',(169.440914255977,-1.41367467356012,3.07899825141338));
#34896=CARTESIAN_POINT('Ctrl Pts',(169.598761271876,-3.35069063941039,0.5015760665558));
#34897=CARTESIAN_POINT('Ctrl Pts',(169.756608287774,-2.25331546141117,-2.53007425709015));
#34898=CARTESIAN_POINT('Ctrl Pts',(169.914455303673,0.884666035299711,-3.27048502929561));
#34899=CARTESIAN_POINT('Ctrl Pts',(170.072302319571,3.22149246026824,-1.04913899093533));
#34900=CARTESIAN_POINT('Ctrl Pts',(170.230149335469,2.64092984065361,2.12230909777109));
#34901=CARTESIAN_POINT('Ctrl Pts',(170.387996351368,-0.331263356051794,
3.37179046643881));
#34902=CARTESIAN_POINT('Ctrl Pts',(170.545843367266,-3.00346385488298,1.56777262964278));
#34903=CARTESIAN_POINT('Ctrl Pts',(170.703690383165,-2.95572245429602,-1.65602272564527));
#34904=CARTESIAN_POINT('Ctrl Pts',(170.861537399063,-0.231273610377281,
-3.38012116904044));
#34905=CARTESIAN_POINT('Ctrl Pts',(171.019384414961,2.70261668758891,-2.04317595483142));
#34906=CARTESIAN_POINT('Ctrl Pts',(171.17723143086,3.18901336295286,1.14407252761205));
#34907=CARTESIAN_POINT('Ctrl Pts',(171.335078446758,0.787432799006144,3.2952476962313));
#34908=CARTESIAN_POINT('Ctrl Pts',(171.492925462657,-2.32724559860833,2.46223950061263));
#34909=CARTESIAN_POINT('Ctrl Pts',(171.650772478555,-3.33437177479195,-0.600574061123454));
#34910=CARTESIAN_POINT('Ctrl Pts',(171.808619494454,-1.32187438082726,-3.1195126227806));
#34911=CARTESIAN_POINT('Ctrl Pts',(171.966466510352,1.88769284474709,-2.81340333947064));
#34912=CARTESIAN_POINT('Ctrl Pts',(172.124313526251,3.38780638409936,0.0405047390324093));
#34913=CARTESIAN_POINT('Ctrl Pts',(172.282160542149,1.81982745081448,2.85778026783241));
#34914=CARTESIAN_POINT('Ctrl Pts',(172.440007558048,-1.39600998068982,3.08694689555915));
#34915=CARTESIAN_POINT('Ctrl Pts',(172.597854573946,-3.34798280609916,0.520767650927842));
#34916=CARTESIAN_POINT('Ctrl Pts',(172.755701589844,-2.26728032039713,-2.51742079655446));
#34917=CARTESIAN_POINT('Ctrl Pts',(172.913548605743,0.865186630521988,-3.27501749282122));
#34918=CARTESIAN_POINT('Ctrl Pts',(173.071395621641,3.21715379479654,-1.06840331277194));
#34919=CARTESIAN_POINT('Ctrl Pts',(173.22924263754,2.64947925870158,2.10919480179326));
#34920=CARTESIAN_POINT('Ctrl Pts',(173.334473981472,0.680908753656591,2.94724158942463));
#34921=CARTESIAN_POINT('Ctrl Pts',(173.387089653438,-0.264521492666898,
2.85979236657441));
#34922=CARTESIAN_POINT('Ctrl Pts',(173.058,-0.317020535431409,3.42736954239177));
#34923=CARTESIAN_POINT('Ctrl Pts',(173.005384328034,0.816047329417257,3.53217463467948));
#34924=CARTESIAN_POINT('Ctrl Pts',(172.952768656068,1.99568167453643,3.02998851994632));
#34925=CARTESIAN_POINT('Ctrl Pts',(172.900152984102,2.69888880492091,2.14418720408781));
#34926=CARTESIAN_POINT('Ctrl Pts',(172.847537312136,3.40209593530543,1.25838588822926));
#34927=CARTESIAN_POINT('Ctrl Pts',(172.794921640169,3.62887585095523,-0.0110306287547288));
#34928=CARTESIAN_POINT('Ctrl Pts',(172.742305968203,3.27247292464401,-1.08649828880944));
#34929=CARTESIAN_POINT('Ctrl Pts',(172.689690296237,2.9160699983328,-2.16196594886414));
#34930=CARTESIAN_POINT('Ctrl Pts',(172.637074624271,1.97648423006066,-3.04348475198962));
#34931=CARTESIAN_POINT('Ctrl Pts',(172.584458952305,0.880997796419955,-3.33291825820939));
#34932=CARTESIAN_POINT('Ctrl Pts',(172.531843280339,-0.214488637220761,
-3.62235176442917));
#34933=CARTESIAN_POINT('Ctrl Pts',(172.479227608372,-1.46587573623001,-3.31969997374319));
#34934=CARTESIAN_POINT('Ctrl Pts',(172.426611936406,-2.30743383748638,-2.56151215661316));
#34935=CARTESIAN_POINT('Ctrl Pts',(172.38218144249,-3.01807461619349,-1.92127213044367));
#34936=CARTESIAN_POINT('Ctrl Pts',(172.337750948573,-3.43647871595114,-0.956203123797524));
#34937=CARTESIAN_POINT('Ctrl Pts',(172.293320454657,-3.44466766225695,0.00262740410212479));
#34938=CARTESIAN_POINT('Origin',(36.8,37.284736894758,-9.99041514095732));
#34939=CARTESIAN_POINT('Ctrl Pts',(36.8,31.4347259190859,-4.53355051147316));
#34940=CARTESIAN_POINT('Ctrl Pts',(36.8,31.1968691126063,-6.18280168905533));
#34941=CARTESIAN_POINT('Ctrl Pts',(36.8,30.8293258095436,-7.81258162569767));
#34942=CARTESIAN_POINT('Ctrl Pts',(36.8,30.0846548283827,-10.2137688485759));
#34943=CARTESIAN_POINT('Ctrl Pts',(36.8,29.8028301128151,-11.0089139056503));
#34944=CARTESIAN_POINT('Ctrl Pts',(36.8,29.4900464626661,-11.7911930472673));
#34945=CARTESIAN_POINT('Ctrl Pts',(37.5,32.4,0.));
#34946=CARTESIAN_POINT('Ctrl Pts',(37.5,32.4,32.4));
#34947=CARTESIAN_POINT('Ctrl Pts',(37.5,0.,32.4));
#34948=CARTESIAN_POINT('Ctrl Pts',(37.5,-32.4,32.4));
#34949=CARTESIAN_POINT('Ctrl Pts',(37.5,-32.4,0.));
#34950=CARTESIAN_POINT('Ctrl Pts',(37.5,-32.4,-32.4));
#34951=CARTESIAN_POINT('Ctrl Pts',(37.5,0.,-32.4));
#34952=CARTESIAN_POINT('Ctrl Pts',(37.5,32.4,-32.4));
#34953=CARTESIAN_POINT('Ctrl Pts',(37.5,32.4,0.));
#34954=CARTESIAN_POINT('Ctrl Pts',(37.3389083940589,32.2580145365138,0.));
#34955=CARTESIAN_POINT('Ctrl Pts',(37.3389083940589,32.2580145365137,32.2580145365137));
#34956=CARTESIAN_POINT('Ctrl Pts',(37.3389083940589,0.,32.2580145365138));
#34957=CARTESIAN_POINT('Ctrl Pts',(37.3389083940589,-32.2580145365137,32.2580145365137));
#34958=CARTESIAN_POINT('Ctrl Pts',(37.3389083940589,-32.2580145365138,0.));
#34959=CARTESIAN_POINT('Ctrl Pts',(37.3389083940589,-32.2580145365137,-32.2580145365137));
#34960=CARTESIAN_POINT('Ctrl Pts',(37.3389083940589,0.,-32.2580145365138));
#34961=CARTESIAN_POINT('Ctrl Pts',(37.3389083940589,32.2580145365137,-32.2580145365137));
#34962=CARTESIAN_POINT('Ctrl Pts',(37.3389083940589,32.2580145365138,0.));
#34963=CARTESIAN_POINT('Ctrl Pts',(37.0144855040189,31.9658168899962,0.));
#34964=CARTESIAN_POINT('Ctrl Pts',(37.0144855040189,31.9658168899962,31.9658168899962));
#34965=CARTESIAN_POINT('Ctrl Pts',(37.0144855040189,0.,31.9658168899962));
#34966=CARTESIAN_POINT('Ctrl Pts',(37.0144855040189,-31.9658168899962,31.9658168899962));
#34967=CARTESIAN_POINT('Ctrl Pts',(37.0144855040189,-31.9658168899962,0.));
#34968=CARTESIAN_POINT('Ctrl Pts',(37.0144855040189,-31.9658168899962,-31.9658168899962));
#34969=CARTESIAN_POINT('Ctrl Pts',(37.0144855040189,0.,-31.9658168899962));
#34970=CARTESIAN_POINT('Ctrl Pts',(37.0144855040189,31.9658168899962,-31.9658168899962));
#34971=CARTESIAN_POINT('Ctrl Pts',(37.0144855040189,31.9658168899962,0.));
#34972=CARTESIAN_POINT('Ctrl Pts',(36.5211322358012,31.5028400616267,0.));
#34973=CARTESIAN_POINT('Ctrl Pts',(36.5211322358012,31.5028400616266,31.5028400616266));
#34974=CARTESIAN_POINT('Ctrl Pts',(36.5211322358012,0.,31.5028400616267));
#34975=CARTESIAN_POINT('Ctrl Pts',(36.5211322358012,-31.5028400616266,31.5028400616266));
#34976=CARTESIAN_POINT('Ctrl Pts',(36.5211322358012,-31.5028400616267,0.));
#34977=CARTESIAN_POINT('Ctrl Pts',(36.5211322358012,-31.5028400616266,-31.5028400616266));
#34978=CARTESIAN_POINT('Ctrl Pts',(36.5211322358012,0.,-31.5028400616267));
#34979=CARTESIAN_POINT('Ctrl Pts',(36.5211322358012,31.5028400616266,-31.5028400616266));
#34980=CARTESIAN_POINT('Ctrl Pts',(36.5211322358012,31.5028400616267,0.));
#34981=CARTESIAN_POINT('Ctrl Pts',(35.849854090057,30.8360498427659,0.));
#34982=CARTESIAN_POINT('Ctrl Pts',(35.849854090057,30.8360498427659,30.8360498427659));
#34983=CARTESIAN_POINT('Ctrl Pts',(35.849854090057,0.,30.8360498427659));
#34984=CARTESIAN_POINT('Ctrl Pts',(35.849854090057,-30.8360498427659,30.8360498427659));
#34985=CARTESIAN_POINT('Ctrl Pts',(35.849854090057,-30.8360498427659,0.));
#34986=CARTESIAN_POINT('Ctrl Pts',(35.849854090057,-30.8360498427659,-30.8360498427659));
#34987=CARTESIAN_POINT('Ctrl Pts',(35.849854090057,0.,-30.8360498427659));
#34988=CARTESIAN_POINT('Ctrl Pts',(35.849854090057,30.8360498427659,-30.8360498427659));
#34989=CARTESIAN_POINT('Ctrl Pts',(35.849854090057,30.8360498427659,0.));
#34990=CARTESIAN_POINT('Ctrl Pts',(34.987601126175,29.9204750609072,0.));
#34991=CARTESIAN_POINT('Ctrl Pts',(34.987601126175,29.9204750609072,29.9204750609072));
#34992=CARTESIAN_POINT('Ctrl Pts',(34.987601126175,0.,29.9204750609072));
#34993=CARTESIAN_POINT('Ctrl Pts',(34.987601126175,-29.9204750609072,29.9204750609072));
#34994=CARTESIAN_POINT('Ctrl Pts',(34.987601126175,-29.9204750609072,0.));
#34995=CARTESIAN_POINT('Ctrl Pts',(34.987601126175,-29.9204750609072,-29.9204750609072));
#34996=CARTESIAN_POINT('Ctrl Pts',(34.987601126175,0.,-29.9204750609072));
#34997=CARTESIAN_POINT('Ctrl Pts',(34.987601126175,29.9204750609072,-29.9204750609072));
#34998=CARTESIAN_POINT('Ctrl Pts',(34.987601126175,29.9204750609072,0.));
#34999=CARTESIAN_POINT('Ctrl Pts',(34.1004337719427,28.9253475198501,0.));
#35000=CARTESIAN_POINT('Ctrl Pts',(34.1004337719427,28.9253475198501,28.9253475198501));
#35001=CARTESIAN_POINT('Ctrl Pts',(34.1004337719427,0.,28.9253475198501));
#35002=CARTESIAN_POINT('Ctrl Pts',(34.1004337719427,-28.9253475198501,28.9253475198501));
#35003=CARTESIAN_POINT('Ctrl Pts',(34.1004337719427,-28.9253475198501,0.));
#35004=CARTESIAN_POINT('Ctrl Pts',(34.1004337719427,-28.9253475198501,-28.9253475198501));
#35005=CARTESIAN_POINT('Ctrl Pts',(34.1004337719427,0.,-28.9253475198501));
#35006=CARTESIAN_POINT('Ctrl Pts',(34.1004337719427,28.9253475198501,-28.9253475198501));
#35007=CARTESIAN_POINT('Ctrl Pts',(34.1004337719427,28.9253475198501,0.));
#35008=CARTESIAN_POINT('Ctrl Pts',(33.1851263782876,27.8567138854442,0.));
#35009=CARTESIAN_POINT('Ctrl Pts',(33.1851263782876,27.8567138854442,27.8567138854442));
#35010=CARTESIAN_POINT('Ctrl Pts',(33.1851263782876,0.,27.8567138854442));
#35011=CARTESIAN_POINT('Ctrl Pts',(33.1851263782876,-27.8567138854442,27.8567138854442));
#35012=CARTESIAN_POINT('Ctrl Pts',(33.1851263782876,-27.8567138854442,0.));
#35013=CARTESIAN_POINT('Ctrl Pts',(33.1851263782876,-27.8567138854442,-27.8567138854442));
#35014=CARTESIAN_POINT('Ctrl Pts',(33.1851263782876,0.,-27.8567138854442));
#35015=CARTESIAN_POINT('Ctrl Pts',(33.1851263782876,27.8567138854442,-27.8567138854442));
#35016=CARTESIAN_POINT('Ctrl Pts',(33.1851263782876,27.8567138854442,0.));
#35017=CARTESIAN_POINT('Ctrl Pts',(32.2364640041498,26.7258152226803,0.));
#35018=CARTESIAN_POINT('Ctrl Pts',(32.2364640041498,26.7258152226803,26.7258152226803));
#35019=CARTESIAN_POINT('Ctrl Pts',(32.2364640041498,0.,26.7258152226803));
#35020=CARTESIAN_POINT('Ctrl Pts',(32.2364640041498,-26.7258152226803,26.7258152226803));
#35021=CARTESIAN_POINT('Ctrl Pts',(32.2364640041498,-26.7258152226803,0.));
#35022=CARTESIAN_POINT('Ctrl Pts',(32.2364640041498,-26.7258152226803,-26.7258152226803));
#35023=CARTESIAN_POINT('Ctrl Pts',(32.2364640041498,0.,-26.7258152226803));
#35024=CARTESIAN_POINT('Ctrl Pts',(32.2364640041498,26.7258152226803,-26.7258152226803));
#35025=CARTESIAN_POINT('Ctrl Pts',(32.2364640041498,26.7258152226803,0.));
#35026=CARTESIAN_POINT('Ctrl Pts',(31.2480536381088,25.5477500100038,0.));
#35027=CARTESIAN_POINT('Ctrl Pts',(31.2480536381088,25.5477500100038,25.5477500100038));
#35028=CARTESIAN_POINT('Ctrl Pts',(31.2480536381088,0.,25.5477500100038));
#35029=CARTESIAN_POINT('Ctrl Pts',(31.2480536381087,-25.5477500100038,25.5477500100038));
#35030=CARTESIAN_POINT('Ctrl Pts',(31.2480536381087,-25.5477500100038,0.));
#35031=CARTESIAN_POINT('Ctrl Pts',(31.2480536381087,-25.5477500100038,-25.5477500100038));
#35032=CARTESIAN_POINT('Ctrl Pts',(31.2480536381088,0.,-25.5477500100038));
#35033=CARTESIAN_POINT('Ctrl Pts',(31.2480536381088,25.5477500100038,-25.5477500100038));
#35034=CARTESIAN_POINT('Ctrl Pts',(31.2480536381088,25.5477500100038,0.));
#35035=CARTESIAN_POINT('Ctrl Pts',(30.2132710279087,24.339870673897,0.));
#35036=CARTESIAN_POINT('Ctrl Pts',(30.2132710279087,24.339870673897,24.339870673897));
#35037=CARTESIAN_POINT('Ctrl Pts',(30.2132710279087,0.,24.339870673897));
#35038=CARTESIAN_POINT('Ctrl Pts',(30.2132710279087,-24.339870673897,24.339870673897));
#35039=CARTESIAN_POINT('Ctrl Pts',(30.2132710279087,-24.339870673897,0.));
#35040=CARTESIAN_POINT('Ctrl Pts',(30.2132710279087,-24.339870673897,-24.339870673897));
#35041=CARTESIAN_POINT('Ctrl Pts',(30.2132710279087,0.,-24.339870673897));
#35042=CARTESIAN_POINT('Ctrl Pts',(30.2132710279087,24.339870673897,-24.339870673897));
#35043=CARTESIAN_POINT('Ctrl Pts',(30.2132710279087,24.339870673897,0.));
#35044=CARTESIAN_POINT('Ctrl Pts',(29.1261855002599,23.1203063432132,0.));
#35045=CARTESIAN_POINT('Ctrl Pts',(29.1261855002599,23.1203063432132,23.1203063432132));
#35046=CARTESIAN_POINT('Ctrl Pts',(29.1261855002599,0.,23.1203063432132));
#35047=CARTESIAN_POINT('Ctrl Pts',(29.1261855002599,-23.1203063432132,23.1203063432132));
#35048=CARTESIAN_POINT('Ctrl Pts',(29.1261855002599,-23.1203063432132,0.));
#35049=CARTESIAN_POINT('Ctrl Pts',(29.1261855002599,-23.1203063432132,-23.1203063432132));
#35050=CARTESIAN_POINT('Ctrl Pts',(29.1261855002599,0.,-23.1203063432132));
#35051=CARTESIAN_POINT('Ctrl Pts',(29.1261855002599,23.1203063432132,-23.1203063432132));
#35052=CARTESIAN_POINT('Ctrl Pts',(29.1261855002599,23.1203063432132,0.));
#35053=CARTESIAN_POINT('Ctrl Pts',(27.9824847998069,21.9065059385018,0.));
#35054=CARTESIAN_POINT('Ctrl Pts',(27.9824847998069,21.9065059385018,21.9065059385018));
#35055=CARTESIAN_POINT('Ctrl Pts',(27.9824847998069,0.,21.9065059385018));
#35056=CARTESIAN_POINT('Ctrl Pts',(27.9824847998069,-21.9065059385018,21.9065059385018));
#35057=CARTESIAN_POINT('Ctrl Pts',(27.9824847998069,-21.9065059385018,0.));
#35058=CARTESIAN_POINT('Ctrl Pts',(27.9824847998069,-21.9065059385018,-21.9065059385018));
#35059=CARTESIAN_POINT('Ctrl Pts',(27.9824847998069,0.,-21.9065059385018));
#35060=CARTESIAN_POINT('Ctrl Pts',(27.9824847998069,21.9065059385018,-21.9065059385018));
#35061=CARTESIAN_POINT('Ctrl Pts',(27.9824847998069,21.9065059385018,0.));
#35062=CARTESIAN_POINT('Ctrl Pts',(26.780529153894,20.7136594976185,0.));
#35063=CARTESIAN_POINT('Ctrl Pts',(26.780529153894,20.7136594976185,20.7136594976185));
#35064=CARTESIAN_POINT('Ctrl Pts',(26.780529153894,0.,20.7136594976185));
#35065=CARTESIAN_POINT('Ctrl Pts',(26.780529153894,-20.7136594976185,20.7136594976185));
#35066=CARTESIAN_POINT('Ctrl Pts',(26.780529153894,-20.7136594976185,0.));
#35067=CARTESIAN_POINT('Ctrl Pts',(26.780529153894,-20.7136594976185,-20.7136594976185));
#35068=CARTESIAN_POINT('Ctrl Pts',(26.780529153894,0.,-20.7136594976185));
#35069=CARTESIAN_POINT('Ctrl Pts',(26.780529153894,20.7136594976185,-20.7136594976185));
#35070=CARTESIAN_POINT('Ctrl Pts',(26.780529153894,20.7136594976185,0.));
#35071=CARTESIAN_POINT('Ctrl Pts',(25.5210824112439,19.5548484421686,0.));
#35072=CARTESIAN_POINT('Ctrl Pts',(25.5210824112439,19.5548484421686,19.5548484421686));
#35073=CARTESIAN_POINT('Ctrl Pts',(25.5210824112439,0.,19.5548484421686));
#35074=CARTESIAN_POINT('Ctrl Pts',(25.5210824112439,-19.5548484421686,19.5548484421686));
#35075=CARTESIAN_POINT('Ctrl Pts',(25.5210824112439,-19.5548484421686,0.));
#35076=CARTESIAN_POINT('Ctrl Pts',(25.5210824112439,-19.5548484421686,-19.5548484421686));
#35077=CARTESIAN_POINT('Ctrl Pts',(25.5210824112439,0.,-19.5548484421686));
#35078=CARTESIAN_POINT('Ctrl Pts',(25.5210824112439,19.5548484421686,-19.5548484421686));
#35079=CARTESIAN_POINT('Ctrl Pts',(25.5210824112439,19.5548484421686,0.));
#35080=CARTESIAN_POINT('Ctrl Pts',(24.2069345847179,18.4413554671298,0.));
#35081=CARTESIAN_POINT('Ctrl Pts',(24.2069345847179,18.4413554671298,18.4413554671298));
#35082=CARTESIAN_POINT('Ctrl Pts',(24.2069345847179,0.,18.4413554671298));
#35083=CARTESIAN_POINT('Ctrl Pts',(24.2069345847179,-18.4413554671298,18.4413554671298));
#35084=CARTESIAN_POINT('Ctrl Pts',(24.2069345847179,-18.4413554671298,0.));
#35085=CARTESIAN_POINT('Ctrl Pts',(24.2069345847179,-18.4413554671298,-18.4413554671298));
#35086=CARTESIAN_POINT('Ctrl Pts',(24.2069345847179,0.,-18.4413554671298));
#35087=CARTESIAN_POINT('Ctrl Pts',(24.2069345847179,18.4413554671298,-18.4413554671298));
#35088=CARTESIAN_POINT('Ctrl Pts',(24.2069345847179,18.4413554671298,0.));
#35089=CARTESIAN_POINT('Ctrl Pts',(22.8426190791586,17.3828861014748,0.));
#35090=CARTESIAN_POINT('Ctrl Pts',(22.8426190791586,17.3828861014748,17.3828861014748));
#35091=CARTESIAN_POINT('Ctrl Pts',(22.8426190791586,0.,17.3828861014748));
#35092=CARTESIAN_POINT('Ctrl Pts',(22.8426190791586,-17.3828861014748,17.3828861014748));
#35093=CARTESIAN_POINT('Ctrl Pts',(22.8426190791586,-17.3828861014748,0.));
#35094=CARTESIAN_POINT('Ctrl Pts',(22.8426190791586,-17.3828861014748,-17.3828861014748));
#35095=CARTESIAN_POINT('Ctrl Pts',(22.8426190791586,0.,-17.3828861014748));
#35096=CARTESIAN_POINT('Ctrl Pts',(22.8426190791586,17.3828861014748,-17.3828861014748));
#35097=CARTESIAN_POINT('Ctrl Pts',(22.8426190791586,17.3828861014748,0.));
#35098=CARTESIAN_POINT('Ctrl Pts',(21.4341168715413,16.3877853586665,0.));
#35099=CARTESIAN_POINT('Ctrl Pts',(21.4341168715413,16.3877853586665,16.3877853586665));
#35100=CARTESIAN_POINT('Ctrl Pts',(21.4341168715413,0.,16.3877853586665));
#35101=CARTESIAN_POINT('Ctrl Pts',(21.4341168715413,-16.3877853586665,16.3877853586665));
#35102=CARTESIAN_POINT('Ctrl Pts',(21.4341168715413,-16.3877853586665,0.));
#35103=CARTESIAN_POINT('Ctrl Pts',(21.4341168715413,-16.3877853586665,-16.3877853586665));
#35104=CARTESIAN_POINT('Ctrl Pts',(21.4341168715413,0.,-16.3877853586665));
#35105=CARTESIAN_POINT('Ctrl Pts',(21.4341168715413,16.3877853586665,-16.3877853586665));
#35106=CARTESIAN_POINT('Ctrl Pts',(21.4341168715413,16.3877853586665,0.));
#35107=CARTESIAN_POINT('Ctrl Pts',(19.9886520715334,15.4632288398589,0.));
#35108=CARTESIAN_POINT('Ctrl Pts',(19.9886520715334,15.4632288398589,15.4632288398589));
#35109=CARTESIAN_POINT('Ctrl Pts',(19.9886520715334,0.,15.4632288398589));
#35110=CARTESIAN_POINT('Ctrl Pts',(19.9886520715334,-15.4632288398589,15.4632288398589));
#35111=CARTESIAN_POINT('Ctrl Pts',(19.9886520715334,-15.4632288398589,0.));
#35112=CARTESIAN_POINT('Ctrl Pts',(19.9886520715334,-15.4632288398589,-15.4632288398589));
#35113=CARTESIAN_POINT('Ctrl Pts',(19.9886520715334,0.,-15.4632288398589));
#35114=CARTESIAN_POINT('Ctrl Pts',(19.9886520715334,15.4632288398589,-15.4632288398589));
#35115=CARTESIAN_POINT('Ctrl Pts',(19.9886520715334,15.4632288398589,0.));
#35116=CARTESIAN_POINT('Ctrl Pts',(18.514323186272,14.6153405598521,0.));
#35117=CARTESIAN_POINT('Ctrl Pts',(18.514323186272,14.6153405598521,14.6153405598521));
#35118=CARTESIAN_POINT('Ctrl Pts',(18.514323186272,0.,14.6153405598521));
#35119=CARTESIAN_POINT('Ctrl Pts',(18.514323186272,-14.6153405598521,14.6153405598521));
#35120=CARTESIAN_POINT('Ctrl Pts',(18.514323186272,-14.6153405598521,0.));
#35121=CARTESIAN_POINT('Ctrl Pts',(18.514323186272,-14.6153405598521,-14.6153405598521));
#35122=CARTESIAN_POINT('Ctrl Pts',(18.514323186272,0.,-14.6153405598521));
#35123=CARTESIAN_POINT('Ctrl Pts',(18.514323186272,14.6153405598521,-14.6153405598521));
#35124=CARTESIAN_POINT('Ctrl Pts',(18.514323186272,14.6153405598521,0.));
#35125=CARTESIAN_POINT('Ctrl Pts',(17.0194794456568,13.8492044429491,0.));
#35126=CARTESIAN_POINT('Ctrl Pts',(17.0194794456568,13.8492044429491,13.8492044429491));
#35127=CARTESIAN_POINT('Ctrl Pts',(17.0194794456568,0.,13.8492044429491));
#35128=CARTESIAN_POINT('Ctrl Pts',(17.0194794456568,-13.8492044429491,13.8492044429491));
#35129=CARTESIAN_POINT('Ctrl Pts',(17.0194794456568,-13.8492044429491,0.));
#35130=CARTESIAN_POINT('Ctrl Pts',(17.0194794456568,-13.8492044429491,-13.8492044429491));
#35131=CARTESIAN_POINT('Ctrl Pts',(17.0194794456568,0.,-13.8492044429491));
#35132=CARTESIAN_POINT('Ctrl Pts',(17.0194794456568,13.8492044429491,-13.8492044429491));
#35133=CARTESIAN_POINT('Ctrl Pts',(17.0194794456568,13.8492044429491,0.));
#35134=CARTESIAN_POINT('Ctrl Pts',(15.5121733229441,13.1688616684146,0.));
#35135=CARTESIAN_POINT('Ctrl Pts',(15.5121733229441,13.1688616684146,13.1688616684146));
#35136=CARTESIAN_POINT('Ctrl Pts',(15.5121733229441,0.,13.1688616684146));
#35137=CARTESIAN_POINT('Ctrl Pts',(15.5121733229441,-13.1688616684146,13.1688616684146));
#35138=CARTESIAN_POINT('Ctrl Pts',(15.5121733229441,-13.1688616684146,0.));
#35139=CARTESIAN_POINT('Ctrl Pts',(15.5121733229441,-13.1688616684146,-13.1688616684146));
#35140=CARTESIAN_POINT('Ctrl Pts',(15.5121733229441,0.,-13.1688616684146));
#35141=CARTESIAN_POINT('Ctrl Pts',(15.5121733229441,13.1688616684146,-13.1688616684146));
#35142=CARTESIAN_POINT('Ctrl Pts',(15.5121733229441,13.1688616684146,0.));
#35143=CARTESIAN_POINT('Ctrl Pts',(13.9995910956154,12.5772662595197,0.));
#35144=CARTESIAN_POINT('Ctrl Pts',(13.9995910956154,12.5772662595197,12.5772662595197));
#35145=CARTESIAN_POINT('Ctrl Pts',(13.9995910956154,0.,12.5772662595197));
#35146=CARTESIAN_POINT('Ctrl Pts',(13.9995910956154,-12.5772662595197,12.5772662595197));
#35147=CARTESIAN_POINT('Ctrl Pts',(13.9995910956154,-12.5772662595197,0.));
#35148=CARTESIAN_POINT('Ctrl Pts',(13.9995910956154,-12.5772662595197,-12.5772662595197));
#35149=CARTESIAN_POINT('Ctrl Pts',(13.9995910956154,0.,-12.5772662595197));
#35150=CARTESIAN_POINT('Ctrl Pts',(13.9995910956154,12.5772662595197,-12.5772662595197));
#35151=CARTESIAN_POINT('Ctrl Pts',(13.9995910956154,12.5772662595197,0.));
#35152=CARTESIAN_POINT('Ctrl Pts',(12.4874918670977,12.076207951456,0.));
#35153=CARTESIAN_POINT('Ctrl Pts',(12.4874918670977,12.076207951456,12.076207951456));
#35154=CARTESIAN_POINT('Ctrl Pts',(12.4874918670977,0.,12.076207951456));
#35155=CARTESIAN_POINT('Ctrl Pts',(12.4874918670977,-12.076207951456,12.076207951456));
#35156=CARTESIAN_POINT('Ctrl Pts',(12.4874918670977,-12.076207951456,0.));
#35157=CARTESIAN_POINT('Ctrl Pts',(12.4874918670977,-12.076207951456,-12.076207951456));
#35158=CARTESIAN_POINT('Ctrl Pts',(12.4874918670977,0.,-12.076207951456));
#35159=CARTESIAN_POINT('Ctrl Pts',(12.4874918670977,12.076207951456,-12.076207951456));
#35160=CARTESIAN_POINT('Ctrl Pts',(12.4874918670977,12.076207951456,0.));
#35161=CARTESIAN_POINT('Ctrl Pts',(10.979632440052,11.6661962584503,0.));
#35162=CARTESIAN_POINT('Ctrl Pts',(10.979632440052,11.6661962584503,11.6661962584503));
#35163=CARTESIAN_POINT('Ctrl Pts',(10.979632440052,0.,11.6661962584503));
#35164=CARTESIAN_POINT('Ctrl Pts',(10.979632440052,-11.6661962584503,11.6661962584503));
#35165=CARTESIAN_POINT('Ctrl Pts',(10.979632440052,-11.6661962584503,0.));
#35166=CARTESIAN_POINT('Ctrl Pts',(10.979632440052,-11.6661962584503,-11.6661962584503));
#35167=CARTESIAN_POINT('Ctrl Pts',(10.979632440052,0.,-11.6661962584503));
#35168=CARTESIAN_POINT('Ctrl Pts',(10.979632440052,11.6661962584503,-11.6661962584503));
#35169=CARTESIAN_POINT('Ctrl Pts',(10.979632440052,11.6661962584503,0.));
#35170=CARTESIAN_POINT('Ctrl Pts',(9.4782023240472,11.3469207764071,0.));
#35171=CARTESIAN_POINT('Ctrl Pts',(9.4782023240472,11.3469207764071,11.3469207764071));
#35172=CARTESIAN_POINT('Ctrl Pts',(9.4782023240472,0.,11.3469207764071));
#35173=CARTESIAN_POINT('Ctrl Pts',(9.47820232404719,-11.3469207764071,11.3469207764071));
#35174=CARTESIAN_POINT('Ctrl Pts',(9.47820232404719,-11.3469207764071,0.));
#35175=CARTESIAN_POINT('Ctrl Pts',(9.47820232404719,-11.3469207764071,-11.3469207764071));
#35176=CARTESIAN_POINT('Ctrl Pts',(9.4782023240472,0.,-11.3469207764071));
#35177=CARTESIAN_POINT('Ctrl Pts',(9.4782023240472,11.3469207764071,-11.3469207764071));
#35178=CARTESIAN_POINT('Ctrl Pts',(9.4782023240472,11.3469207764071,0.));
#35179=CARTESIAN_POINT('Ctrl Pts',(8.28303567503975,11.1635245405655,0.));
#35180=CARTESIAN_POINT('Ctrl Pts',(8.28303567503975,11.1635245405655,11.1635245405655));
#35181=CARTESIAN_POINT('Ctrl Pts',(8.28303567503976,0.,11.1635245405655));
#35182=CARTESIAN_POINT('Ctrl Pts',(8.28303567503978,-11.1635245405655,11.1635245405655));
#35183=CARTESIAN_POINT('Ctrl Pts',(8.28303567503978,-11.1635245405655,0.));
#35184=CARTESIAN_POINT('Ctrl Pts',(8.28303567503978,-11.1635245405655,-11.1635245405655));
#35185=CARTESIAN_POINT('Ctrl Pts',(8.28303567503976,0.,-11.1635245405655));
#35186=CARTESIAN_POINT('Ctrl Pts',(8.28303567503975,11.1635245405655,-11.1635245405655));
#35187=CARTESIAN_POINT('Ctrl Pts',(8.28303567503975,11.1635245405655,0.));
#35188=CARTESIAN_POINT('Ctrl Pts',(7.39016039139644,11.0661718180104,0.));
#35189=CARTESIAN_POINT('Ctrl Pts',(7.39016039139644,11.0661718180104,11.0661718180104));
#35190=CARTESIAN_POINT('Ctrl Pts',(7.39016039139642,0.,11.0661718180104));
#35191=CARTESIAN_POINT('Ctrl Pts',(7.3901603913964,-11.0661718180104,11.0661718180104));
#35192=CARTESIAN_POINT('Ctrl Pts',(7.3901603913964,-11.0661718180104,0.));
#35193=CARTESIAN_POINT('Ctrl Pts',(7.3901603913964,-11.0661718180104,-11.0661718180104));
#35194=CARTESIAN_POINT('Ctrl Pts',(7.39016039139642,0.,-11.0661718180104));
#35195=CARTESIAN_POINT('Ctrl Pts',(7.39016039139644,11.0661718180104,-11.0661718180104));
#35196=CARTESIAN_POINT('Ctrl Pts',(7.39016039139644,11.0661718180104,0.));
#35197=CARTESIAN_POINT('Ctrl Pts',(6.79646156908522,11.0190876606754,0.));
#35198=CARTESIAN_POINT('Ctrl Pts',(6.79646156908522,11.0190876606754,11.0190876606754));
#35199=CARTESIAN_POINT('Ctrl Pts',(6.79646156908522,0.,11.0190876606754));
#35200=CARTESIAN_POINT('Ctrl Pts',(6.79646156908521,-11.0190876606754,11.0190876606754));
#35201=CARTESIAN_POINT('Ctrl Pts',(6.79646156908521,-11.0190876606754,0.));
#35202=CARTESIAN_POINT('Ctrl Pts',(6.79646156908521,-11.0190876606754,-11.0190876606754));
#35203=CARTESIAN_POINT('Ctrl Pts',(6.79646156908522,0.,-11.0190876606754));
#35204=CARTESIAN_POINT('Ctrl Pts',(6.79646156908522,11.0190876606754,-11.0190876606754));
#35205=CARTESIAN_POINT('Ctrl Pts',(6.79646156908522,11.0190876606754,0.));
#35206=CARTESIAN_POINT('Ctrl Pts',(6.5,11.,0.));
#35207=CARTESIAN_POINT('Ctrl Pts',(6.5,11.,11.));
#35208=CARTESIAN_POINT('Ctrl Pts',(6.49999999999999,0.,11.));
#35209=CARTESIAN_POINT('Ctrl Pts',(6.49999999999997,-11.,11.));
#35210=CARTESIAN_POINT('Ctrl Pts',(6.49999999999997,-11.,0.));
#35211=CARTESIAN_POINT('Ctrl Pts',(6.49999999999997,-11.,-11.));
#35212=CARTESIAN_POINT('Ctrl Pts',(6.49999999999999,0.,-11.));
#35213=CARTESIAN_POINT('Ctrl Pts',(6.5,11.,-11.));
#35214=CARTESIAN_POINT('Ctrl Pts',(6.5,11.,0.));
#35215=CARTESIAN_POINT('',(37.5,28.7791366260183,-14.8835914705078));
#35216=CARTESIAN_POINT('Origin',(37.5,0.,0.));
#35217=CARTESIAN_POINT('Ctrl Pts',(37.5,28.7791366260183,-14.8835914705078));
#35218=CARTESIAN_POINT('Ctrl Pts',(36.649069632136,28.1289147924197,-14.5081857198467));
#35219=CARTESIAN_POINT('Ctrl Pts',(35.8406537800852,27.4207836130568,-14.09934599282));
#35220=CARTESIAN_POINT('Ctrl Pts',(35.0774452370494,26.7027592162945,-13.6847944140645));
#35221=CARTESIAN_POINT('Ctrl Pts',(34.6958409655315,26.3437470179134,-13.4775186246868));
#35222=CARTESIAN_POINT('Ctrl Pts',(34.325525504156,25.9822790638981,-13.2688250041327));
#35223=CARTESIAN_POINT('Ctrl Pts',(33.9666810635171,25.6244801370594,-13.0622496974066));
#35224=CARTESIAN_POINT('Ctrl Pts',(33.7186145566393,25.3771363861364,-12.9194457162288));
#35225=CARTESIAN_POINT('Ctrl Pts',(33.4671024168736,25.1224476749782,-12.7724011202821));
#35226=CARTESIAN_POINT('Ctrl Pts',(33.240098560953,24.8908093158805,-12.6386646513024));
#35227=CARTESIAN_POINT('Ctrl Pts',(33.1387264796059,24.7873676254901,-12.57894256351));
#35228=CARTESIAN_POINT('Ctrl Pts',(33.0532004124034,24.6997339702839,-12.5283472490867));
#35229=CARTESIAN_POINT('Ctrl Pts',(33.,24.6451817466334,-12.4968515080772));
#35230=CARTESIAN_POINT('Ctrl Pts',(32.9185691495925,24.5616817555094,-12.4486427657244));
#35231=CARTESIAN_POINT('Ctrl Pts',(32.8516820633328,24.4928265642782,-12.409196518007));
#35232=CARTESIAN_POINT('Ctrl Pts',(32.7777321456107,24.4165289206872,-12.3657029367534));
#35233=CARTESIAN_POINT('Ctrl Pts',(32.1788699540342,23.7986543447516,-12.0134826477878));
#35234=CARTESIAN_POINT('Ctrl Pts',(31.5692879871746,23.1567007301737,-11.6640598398951));
#35235=CARTESIAN_POINT('Ctrl Pts',(30.9513498040921,22.5260018679958,-11.3096185478676));
#35236=CARTESIAN_POINT('Ctrl Pts',(30.6423807125509,22.2106524369068,-11.1323979018538));
#35237=CARTESIAN_POINT('Ctrl Pts',(30.3347880607231,21.9015729508235,-10.9558507302175));
#35238=CARTESIAN_POINT('Ctrl Pts',(30.0249306372031,21.5982641082966,-10.7763433330279));
#35239=CARTESIAN_POINT('Ctrl Pts',(29.8700019254431,21.4466096870331,-10.686589634433));
#35240=CARTESIAN_POINT('Ctrl Pts',(29.7145097313607,21.2963965338214,-10.5960927952803));
#35241=CARTESIAN_POINT('Ctrl Pts',(29.5580100720539,21.1475727378965,-10.5043591957328));
#35242=CARTESIAN_POINT('Ctrl Pts',(29.4797602424005,21.073160839934,-10.4584923959591));
#35243=CARTESIAN_POINT('Ctrl Pts',(29.4012586241275,20.9990965425516,-10.4123158264294));
#35244=CARTESIAN_POINT('Ctrl Pts',(29.3224502420548,20.9253755287796,-10.365763682916));
#35245=CARTESIAN_POINT('Ctrl Pts',(29.2736528205758,20.8797281587122,-10.3369390260962));
#35246=CARTESIAN_POINT('Ctrl Pts',(29.224737793648,20.8342124355121,-10.3079703168046));
#35247=CARTESIAN_POINT('Ctrl Pts',(29.1756921968363,20.7888277155615,-10.2788413041483));
#35248=CARTESIAN_POINT('Ctrl Pts',(29.145528605634,20.7609156046197,-10.2609266352074));
#35249=CARTESIAN_POINT('Ctrl Pts',(29.1181490967959,20.7356566759367,-10.244640315201));
#35250=CARTESIAN_POINT('Ctrl Pts',(29.0849408699094,20.7051394327917,-10.2248462834623));
#35251=CARTESIAN_POINT('Ctrl Pts',(29.0475462330933,20.6707750197823,-10.2025569082866));
#35252=CARTESIAN_POINT('Ctrl Pts',(28.9599837407508,20.5905365512908,-10.1505620075807));
#35253=CARTESIAN_POINT('Ctrl Pts',(28.8924081847227,20.5290030523156,-10.1107110564612));
#35254=CARTESIAN_POINT('Ctrl Pts',(28.4410807634675,20.1180296612603,-9.84455228455516));
#35255=CARTESIAN_POINT('Ctrl Pts',(27.9936088567084,19.7235361016838,-9.59004457953207));
#35256=CARTESIAN_POINT('Ctrl Pts',(27.5122543095276,19.323133857666,-9.31395242983164));
#35257=CARTESIAN_POINT('Ctrl Pts',(27.139729410595,19.0132587222617,-9.1002820682123));
#35258=CARTESIAN_POINT('Ctrl Pts',(26.7276341640933,18.6830630721049,-8.8641048839258));
#35259=CARTESIAN_POINT('Ctrl Pts',(26.2530417505368,18.3335669465969,-8.57522710561967));
#35260=CARTESIAN_POINT('Ctrl Pts',(25.8694949138874,18.0511179871724,-8.34176749926539));
#35261=CARTESIAN_POINT('Ctrl Pts',(25.4447383161169,17.7540556187449,-8.07732257196191));
#35262=CARTESIAN_POINT('Ctrl Pts',(24.9635886608471,17.4401876876843,-7.77432947327891));
#35263=CARTESIAN_POINT('Ctrl Pts',(24.6119820459101,17.2108244540856,-7.55291317045008));
#35264=CARTESIAN_POINT('Ctrl Pts',(24.2873626785113,17.0017823418324,-7.34685978855489));
#35265=CARTESIAN_POINT('Ctrl Pts',(23.6426616416151,16.6259529313881,-6.93898570158392));
#35266=CARTESIAN_POINT('Ctrl Pts',(23.5760533210473,16.5871235136936,-6.89684553679212));
#35267=CARTESIAN_POINT('Ctrl Pts',(23.5065967304624,16.546947509807,-6.85292160231549));
#35268=CARTESIAN_POINT('Ctrl Pts',(23.4342591639586,16.5054784159948,-6.80720851268154));
#35269=CARTESIAN_POINT('Ctrl Pts',(22.7443384436259,16.1099662574127,-6.37121917473146));
#35270=CARTESIAN_POINT('Ctrl Pts',(21.7987837593167,15.60840670368,-5.75271743557013));
#35271=CARTESIAN_POINT('Ctrl Pts',(20.5610365528855,15.0432759423309,-4.96573918168373));
#35272=CARTESIAN_POINT('Ctrl Pts',(19.7234582214111,14.660854331766,-4.4331943054991));
#35273=CARTESIAN_POINT('Ctrl Pts',(18.7603809281631,14.261757368588,-3.80221290992202));
#35274=CARTESIAN_POINT('Ctrl Pts',(17.6514222906382,13.8414640697512,-3.1023654549763));
#35275=CARTESIAN_POINT('Ctrl Pts',(16.7565277906389,13.5023006881889,-2.53761072285453));
#35276=CARTESIAN_POINT('Ctrl Pts',(15.7613531057993,13.1550396644396,-1.89251696162035));
#35277=CARTESIAN_POINT('Ctrl Pts',(14.7199456843001,12.8103130578295,-1.24172578532011));
#35278=CARTESIAN_POINT('Ctrl Pts',(14.0653277478803,12.5936214775802,-0.832645181442172));
#35279=CARTESIAN_POINT('Ctrl Pts',(13.4031503824703,12.3831266019898,-0.410460471251366));
#35280=CARTESIAN_POINT('Ctrl Pts',(12.7552064848291,12.1808231353727,-1.04083408558608E-16));
#35281=CARTESIAN_POINT('Origin',(37.75,0.,0.));
#35282=CARTESIAN_POINT('Ctrl Pts',(38.0021093499888,29.2991567049652,-15.1841362142249));
#35283=CARTESIAN_POINT('Ctrl Pts',(37.8357506665067,29.1259188005428,-15.0841362838782));
#35284=CARTESIAN_POINT('Ctrl Pts',(37.6692050584524,28.9524909653522,-14.984024599313));
#35285=CARTESIAN_POINT('Ctrl Pts',(37.5025598114679,28.778970498635,-14.8838564824963));
#35286=CARTESIAN_POINT('Origin',(36.8,27.2943217538007,-27.2943217538008));
#35287=CARTESIAN_POINT('Origin',(36.8,27.2943217538007,-27.2943217538008));
#35288=CARTESIAN_POINT('Origin',(36.8,27.2943217538007,-27.2943217538008));
#35289=CARTESIAN_POINT('Ctrl Pts',(37.5,19.4092743732571,-25.9430157904517));
#35290=CARTESIAN_POINT('Ctrl Pts',(37.5185015343068,19.4038236586252,-25.9748214246283));
#35291=CARTESIAN_POINT('Ctrl Pts',(37.537045458494,19.398593936034,-26.0064935487318));
#35292=CARTESIAN_POINT('Ctrl Pts',(37.599346002575,19.3817798286964,-26.1122358651254));
#35293=CARTESIAN_POINT('Ctrl Pts',(37.6438438231274,19.3710168782448,-26.18666663184));
#35294=CARTESIAN_POINT('Ctrl Pts',(37.6890795305109,19.3613019153151,-26.2612698469762));
#35295=CARTESIAN_POINT('Ctrl Pts',(37.6890795305109,26.2612698469761,-19.3613019153152));
#35296=CARTESIAN_POINT('Ctrl Pts',(37.6438438231274,26.18666663184,-19.3710168782449));
#35297=CARTESIAN_POINT('Ctrl Pts',(37.599346002575,26.1122358651254,-19.3817798286965));
#35298=CARTESIAN_POINT('Ctrl Pts',(37.537045458494,26.0064935487318,-19.3985939360341));
#35299=CARTESIAN_POINT('Ctrl Pts',(37.5185015343068,25.9748214246282,-19.4038236586252));
#35300=CARTESIAN_POINT('Ctrl Pts',(37.5,25.9430157904516,-19.4092743732572));
#35301=CARTESIAN_POINT('Origin',(37.75,0.,0.));
#35302=CARTESIAN_POINT('Ctrl Pts',(38.0020193561147,17.781768196856,-27.7994139997877));
#35303=CARTESIAN_POINT('Ctrl Pts',(37.8356549036389,17.6817410994363,-27.6261918543797));
#35304=CARTESIAN_POINT('Ctrl Pts',(37.6691041509159,17.5816052376133,-27.4527780511187));
#35305=CARTESIAN_POINT('Ctrl Pts',(37.5024547303957,17.4814171457625,-27.2792691849716));
#35306=CARTESIAN_POINT('Origin',(37.75,0.,0.));
#35307=CARTESIAN_POINT('Origin',(36.8,9.9904151409573,-37.284736894758));
#35308=CARTESIAN_POINT('Origin',(36.8,9.99041514095729,-37.284736894758));
#35309=CARTESIAN_POINT('Origin',(36.8,9.99041514095729,-37.284736894758));
#35310=CARTESIAN_POINT('Ctrl Pts',(37.5,3.83741678103716,-32.1719479119405));
#35311=CARTESIAN_POINT('Ctrl Pts',(37.5185015343068,3.81679350660879,-32.196767041805));
#35312=CARTESIAN_POINT('Ctrl Pts',(37.537045458494,3.79642837193836,-32.2215810445749));
#35313=CARTESIAN_POINT('Ctrl Pts',(37.599346002575,3.72899576964523,-32.304749523158));
#35314=CARTESIAN_POINT('Ctrl Pts',(37.6438438231274,3.68245939777719,-32.3638269827301));
#35315=CARTESIAN_POINT('Ctrl Pts',(37.6890795305109,3.63674438551514,-32.4235777807772));
#35316=CARTESIAN_POINT('Ctrl Pts',(37.6890795305109,13.0622758654621,-29.8980142324913));
#35317=CARTESIAN_POINT('Ctrl Pts',(37.6438438231274,12.9928101044853,-29.8691260296172));
#35318=CARTESIAN_POINT('Ctrl Pts',(37.599346002575,12.9229696944615,-29.8412316347707));
#35319=CARTESIAN_POINT('Ctrl Pts',(37.537045458494,12.8229871085408,-29.8029219206701));
#35320=CARTESIAN_POINT('Ctrl Pts',(37.5185015343068,12.7929433831798,-29.791614931237));
#35321=CARTESIAN_POINT('Ctrl Pts',(37.5,12.7626735386834,-29.7804325714888));
#35322=CARTESIAN_POINT('Origin',(37.75,0.,0.));
#35323=CARTESIAN_POINT('Ctrl Pts',(38.0015719566141,1.49985854343196,-32.9658822396213));
#35324=CARTESIAN_POINT('Ctrl Pts',(37.8351948506471,1.49984891222423,-32.7658537908257));
#35325=CARTESIAN_POINT('Ctrl Pts',(37.6686397502842,1.49983991459912,-32.5656049542644));
#35326=CARTESIAN_POINT('Ctrl Pts',(37.5019970368724,1.49983187417044,-32.3652476458237));
#35327=CARTESIAN_POINT('Origin',(37.75,0.,0.));
#35328=CARTESIAN_POINT('Origin',(36.8,-9.99041514095732,-37.284736894758));
#35329=CARTESIAN_POINT('Origin',(36.8,-9.99041514095732,-37.284736894758));
#35330=CARTESIAN_POINT('Origin',(36.8,-9.99041514095732,-37.284736894758));
#35331=CARTESIAN_POINT('Ctrl Pts',(37.5,-12.7626735386834,-29.7804325714888));
#35332=CARTESIAN_POINT('Ctrl Pts',(37.5185015343068,-12.7929433831798,-29.791614931237));
#35333=CARTESIAN_POINT('Ctrl Pts',(37.537045458494,-12.8229871085408,-29.8029219206701));
#35334=CARTESIAN_POINT('Ctrl Pts',(37.599346002575,-12.9229696944615,-29.8412316347707));
#35335=CARTESIAN_POINT('Ctrl Pts',(37.6438438231274,-12.9928101044853,-29.8691260296172));
#35336=CARTESIAN_POINT('Ctrl Pts',(37.6890795305109,-13.0622758654621,-29.8980142324913));
#35337=CARTESIAN_POINT('Ctrl Pts',(37.6890795305109,-3.63674438551516,-32.4235777807772));
#35338=CARTESIAN_POINT('Ctrl Pts',(37.6438438231274,-3.68245939777721,-32.3638269827301));
#35339=CARTESIAN_POINT('Ctrl Pts',(37.599346002575,-3.72899576964525,-32.304749523158));
#35340=CARTESIAN_POINT('Ctrl Pts',(37.537045458494,-3.79642837193839,-32.2215810445749));
#35341=CARTESIAN_POINT('Ctrl Pts',(37.5185015343068,-3.81679350660881,-32.196767041805));
#35342=CARTESIAN_POINT('Ctrl Pts',(37.5,-3.83741678103718,-32.1719479119405));
#35343=CARTESIAN_POINT('Origin',(37.75,0.,0.));
#35344=CARTESIAN_POINT('Ctrl Pts',(38.0021093499887,-15.1841362142249,-29.2991567049651));
#35345=CARTESIAN_POINT('Ctrl Pts',(37.8357506665065,-15.0841362838781,-29.1259188005426));
#35346=CARTESIAN_POINT('Ctrl Pts',(37.6692050584523,-14.9840245993129,-28.952490965352));
#35347=CARTESIAN_POINT('Ctrl Pts',(37.5025598114678,-14.8838564824962,-28.778970498635));
#35348=CARTESIAN_POINT('Origin',(37.75,0.,0.));
#35349=CARTESIAN_POINT('Origin',(36.8,-27.2943217538008,-27.2943217538007));
#35350=CARTESIAN_POINT('Origin',(36.8,-27.2943217538008,-27.2943217538007));
#35351=CARTESIAN_POINT('Origin',(36.8,-27.2943217538008,-27.2943217538007));
#35352=CARTESIAN_POINT('Ctrl Pts',(37.5,-25.9430157904517,-19.4092743732571));
#35353=CARTESIAN_POINT('Ctrl Pts',(37.5185015343068,-25.9748214246283,-19.4038236586252));
#35354=CARTESIAN_POINT('Ctrl Pts',(37.537045458494,-26.0064935487318,-19.398593936034));
#35355=CARTESIAN_POINT('Ctrl Pts',(37.599346002575,-26.1122358651254,-19.3817798286965));
#35356=CARTESIAN_POINT('Ctrl Pts',(37.6438438231274,-26.18666663184,-19.3710168782449));
#35357=CARTESIAN_POINT('Ctrl Pts',(37.6890795305109,-26.2612698469762,-19.3613019153151));
#35358=CARTESIAN_POINT('Ctrl Pts',(37.6890795305109,-19.3613019153151,-26.2612698469761));
#35359=CARTESIAN_POINT('Ctrl Pts',(37.6438438231274,-19.3710168782449,-26.18666663184));
#35360=CARTESIAN_POINT('Ctrl Pts',(37.599346002575,-19.3817798286965,-26.1122358651254));
#35361=CARTESIAN_POINT('Ctrl Pts',(37.537045458494,-19.3985939360341,-26.0064935487318));
#35362=CARTESIAN_POINT('Ctrl Pts',(37.5185015343068,-19.4038236586252,-25.9748214246282));
#35363=CARTESIAN_POINT('Ctrl Pts',(37.5,-19.4092743732572,-25.9430157904516));
#35364=CARTESIAN_POINT('Origin',(37.75,0.,0.));
#35365=CARTESIAN_POINT('Ctrl Pts',(38.0020193561148,-27.7994139997878,-17.7817681968561));
#35366=CARTESIAN_POINT('Ctrl Pts',(37.8356549036392,-27.62619185438,-17.6817410994365));
#35367=CARTESIAN_POINT('Ctrl Pts',(37.6691041509162,-27.452778051119,-17.5816052376135));
#35368=CARTESIAN_POINT('Ctrl Pts',(37.5024547303958,-27.2792691849717,-17.4814171457626));
#35369=CARTESIAN_POINT('Origin',(37.75,0.,0.));
#35370=CARTESIAN_POINT('Origin',(36.8,-37.284736894758,-9.9904151409573));
#35371=CARTESIAN_POINT('Origin',(36.8,-37.284736894758,-9.9904151409573));
#35372=CARTESIAN_POINT('Origin',(36.8,-37.284736894758,-9.9904151409573));
#35373=CARTESIAN_POINT('Ctrl Pts',(37.5,-32.1719479119405,-3.83741678103716));
#35374=CARTESIAN_POINT('Ctrl Pts',(37.5185015343068,-32.196767041805,-3.81679350660879));
#35375=CARTESIAN_POINT('Ctrl Pts',(37.537045458494,-32.2215810445749,-3.79642837193836));
#35376=CARTESIAN_POINT('Ctrl Pts',(37.599346002575,-32.304749523158,-3.72899576964523));
#35377=CARTESIAN_POINT('Ctrl Pts',(37.6438438231274,-32.3638269827301,-3.68245939777719));
#35378=CARTESIAN_POINT('Ctrl Pts',(37.6890795305109,-32.4235777807772,-3.63674438551514));
#35379=CARTESIAN_POINT('Ctrl Pts',(37.6890795305109,-29.8980142324913,-13.062275865462));
#35380=CARTESIAN_POINT('Ctrl Pts',(37.6438438231274,-29.8691260296172,-12.9928101044853));
#35381=CARTESIAN_POINT('Ctrl Pts',(37.599346002575,-29.8412316347707,-12.9229696944615));
#35382=CARTESIAN_POINT('Ctrl Pts',(37.537045458494,-29.8029219206701,-12.8229871085408));
#35383=CARTESIAN_POINT('Ctrl Pts',(37.5185015343068,-29.791614931237,-12.7929433831798));
#35384=CARTESIAN_POINT('Ctrl Pts',(37.5,-29.7804325714888,-12.7626735386834));
#35385=CARTESIAN_POINT('Origin',(37.75,0.,0.));
#35386=CARTESIAN_POINT('Ctrl Pts',(38.0015719566141,-32.9658822396213,-1.49985854343196));
#35387=CARTESIAN_POINT('Ctrl Pts',(37.8351948506461,-32.7658537908245,-1.49984891222423));
#35388=CARTESIAN_POINT('Ctrl Pts',(37.6686397502833,-32.5656049542633,-1.49983991459912));
#35389=CARTESIAN_POINT('Ctrl Pts',(37.5019970368724,-32.3652476458237,-1.49983187417044));
#35390=CARTESIAN_POINT('Origin',(37.75,0.,0.));
#35391=CARTESIAN_POINT('Origin',(36.8,-37.284736894758,9.99041514095732));
#35392=CARTESIAN_POINT('Origin',(36.8,-37.284736894758,9.99041514095732));
#35393=CARTESIAN_POINT('Origin',(36.8,-37.284736894758,9.99041514095732));
#35394=CARTESIAN_POINT('Ctrl Pts',(37.5,-29.7804325714888,12.7626735386834));
#35395=CARTESIAN_POINT('Ctrl Pts',(37.5185015343068,-29.791614931237,12.7929433831798));
#35396=CARTESIAN_POINT('Ctrl Pts',(37.537045458494,-29.8029219206701,12.8229871085408));
#35397=CARTESIAN_POINT('Ctrl Pts',(37.599346002575,-29.8412316347707,12.9229696944615));
#35398=CARTESIAN_POINT('Ctrl Pts',(37.6438438231274,-29.8691260296172,12.9928101044853));
#35399=CARTESIAN_POINT('Ctrl Pts',(37.6890795305109,-29.8980142324913,13.0622758654621));
#35400=CARTESIAN_POINT('Ctrl Pts',(37.6890795305109,-32.4235777807772,3.63674438551516));
#35401=CARTESIAN_POINT('Ctrl Pts',(37.6438438231274,-32.3638269827301,3.68245939777721));
#35402=CARTESIAN_POINT('Ctrl Pts',(37.599346002575,-32.304749523158,3.72899576964525));
#35403=CARTESIAN_POINT('Ctrl Pts',(37.537045458494,-32.2215810445749,3.79642837193838));
#35404=CARTESIAN_POINT('Ctrl Pts',(37.5185015343068,-32.196767041805,3.81679350660881));
#35405=CARTESIAN_POINT('Ctrl Pts',(37.5,-32.1719479119405,3.83741678103718));
#35406=CARTESIAN_POINT('Origin',(37.75,0.,0.));
#35407=CARTESIAN_POINT('Ctrl Pts',(38.0021093499888,-29.2991567049652,15.1841362142249));
#35408=CARTESIAN_POINT('Ctrl Pts',(37.8357506665061,-29.1259188005422,15.0841362838778));
#35409=CARTESIAN_POINT('Ctrl Pts',(37.6692050584519,-28.9524909653516,14.9840245993126));
#35410=CARTESIAN_POINT('Ctrl Pts',(37.5025598114679,-28.778970498635,14.8838564824963));
#35411=CARTESIAN_POINT('Origin',(37.75,0.,0.));
#35412=CARTESIAN_POINT('Origin',(36.8,-27.2943217538007,27.2943217538008));
#35413=CARTESIAN_POINT('Origin',(36.8,-27.2943217538007,27.2943217538008));
#35414=CARTESIAN_POINT('Origin',(36.8,-27.2943217538007,27.2943217538008));
#35415=CARTESIAN_POINT('Ctrl Pts',(37.5,-19.4092743732572,25.9430157904517));
#35416=CARTESIAN_POINT('Ctrl Pts',(37.5185015343068,-19.4038236586252,25.9748214246283));
#35417=CARTESIAN_POINT('Ctrl Pts',(37.537045458494,-19.398593936034,26.0064935487318));
#35418=CARTESIAN_POINT('Ctrl Pts',(37.599346002575,-19.3817798286965,26.1122358651254));
#35419=CARTESIAN_POINT('Ctrl Pts',(37.6438438231274,-19.3710168782449,26.18666663184));
#35420=CARTESIAN_POINT('Ctrl Pts',(37.6890795305109,-19.3613019153151,26.2612698469761));
#35421=CARTESIAN_POINT('Ctrl Pts',(37.6890795305109,-26.2612698469761,19.3613019153151));
#35422=CARTESIAN_POINT('Ctrl Pts',(37.6438438231274,-26.18666663184,19.3710168782449));
#35423=CARTESIAN_POINT('Ctrl Pts',(37.599346002575,-26.1122358651254,19.3817798286965));
#35424=CARTESIAN_POINT('Ctrl Pts',(37.537045458494,-26.0064935487318,19.3985939360341));
#35425=CARTESIAN_POINT('Ctrl Pts',(37.5185015343068,-25.9748214246282,19.4038236586252));
#35426=CARTESIAN_POINT('Ctrl Pts',(37.5,-25.9430157904516,19.4092743732572));
#35427=CARTESIAN_POINT('Origin',(37.75,0.,0.));
#35428=CARTESIAN_POINT('Ctrl Pts',(38.0020193561148,-17.7817681968561,27.7994139997878));
#35429=CARTESIAN_POINT('Ctrl Pts',(37.8356549036384,-17.681741099436,27.6261918543792));
#35430=CARTESIAN_POINT('Ctrl Pts',(37.6691041509155,-17.5816052376131,27.4527780511183));
#35431=CARTESIAN_POINT('Ctrl Pts',(37.5024547303958,-17.4814171457626,27.2792691849717));
#35432=CARTESIAN_POINT('Origin',(37.75,0.,0.));
#35433=CARTESIAN_POINT('Origin',(36.8,-9.9904151409573,37.284736894758));
#35434=CARTESIAN_POINT('Origin',(36.8,-9.9904151409573,37.284736894758));
#35435=CARTESIAN_POINT('Origin',(36.8,-9.9904151409573,37.284736894758));
#35436=CARTESIAN_POINT('Ctrl Pts',(37.5,-3.83741678103716,32.1719479119405));
#35437=CARTESIAN_POINT('Ctrl Pts',(37.5185015343068,-3.81679350660879,32.196767041805));
#35438=CARTESIAN_POINT('Ctrl Pts',(37.537045458494,-3.79642837193837,32.2215810445749));
#35439=CARTESIAN_POINT('Ctrl Pts',(37.599346002575,-3.72899576964524,32.304749523158));
#35440=CARTESIAN_POINT('Ctrl Pts',(37.6438438231274,-3.6824593977772,32.3638269827301));
#35441=CARTESIAN_POINT('Ctrl Pts',(37.6890795305109,-3.63674438551516,32.4235777807772));
#35442=CARTESIAN_POINT('Ctrl Pts',(37.6890795305109,-13.062275865462,29.8980142324913));
#35443=CARTESIAN_POINT('Ctrl Pts',(37.6438438231274,-12.9928101044853,29.8691260296172));
#35444=CARTESIAN_POINT('Ctrl Pts',(37.599346002575,-12.9229696944615,29.8412316347707));
#35445=CARTESIAN_POINT('Ctrl Pts',(37.537045458494,-12.8229871085408,29.8029219206701));
#35446=CARTESIAN_POINT('Ctrl Pts',(37.5185015343068,-12.7929433831798,29.791614931237));
#35447=CARTESIAN_POINT('Ctrl Pts',(37.5,-12.7626735386834,29.7804325714888));
#35448=CARTESIAN_POINT('Origin',(37.75,0.,0.));
#35449=CARTESIAN_POINT('Ctrl Pts',(38.0015568568142,-1.49984972337186,32.9658830225135));
#35450=CARTESIAN_POINT('Ctrl Pts',(37.8351792988183,-1.49983922310652,32.7658546589327));
#35451=CARTESIAN_POINT('Ctrl Pts',(37.6686239963487,-1.4998293398377,32.565605908985));
#35452=CARTESIAN_POINT('Ctrl Pts',(37.5019813987213,-1.49982043004959,32.365248683748));
#35453=CARTESIAN_POINT('Origin',(37.75,0.,0.));
#35454=CARTESIAN_POINT('Origin',(36.8,9.99041514095731,37.284736894758));
#35455=CARTESIAN_POINT('Origin',(36.8,9.99041514095731,37.284736894758));
#35456=CARTESIAN_POINT('Origin',(36.8,9.99041514095731,37.284736894758));
#35457=CARTESIAN_POINT('Ctrl Pts',(37.5,12.7626735386834,29.7804325714888));
#35458=CARTESIAN_POINT('Ctrl Pts',(37.5185015343068,12.7929433831798,29.791614931237));
#35459=CARTESIAN_POINT('Ctrl Pts',(37.537045458494,12.8229871085408,29.8029219206701));
#35460=CARTESIAN_POINT('Ctrl Pts',(37.599346002575,12.9229696944615,29.8412316347707));
#35461=CARTESIAN_POINT('Ctrl Pts',(37.6438438231274,12.9928101044853,29.8691260296172));
#35462=CARTESIAN_POINT('Ctrl Pts',(37.6890795305109,13.062275865462,29.8980142324913));
#35463=CARTESIAN_POINT('Ctrl Pts',(37.6890795305109,3.63674438551516,32.4235777807772));
#35464=CARTESIAN_POINT('Ctrl Pts',(37.6438438231274,3.68245939777721,32.3638269827301));
#35465=CARTESIAN_POINT('Ctrl Pts',(37.599346002575,3.72899576964524,32.304749523158));
#35466=CARTESIAN_POINT('Ctrl Pts',(37.537045458494,3.79642837193838,32.2215810445749));
#35467=CARTESIAN_POINT('Ctrl Pts',(37.5185015343068,3.8167935066088,32.196767041805));
#35468=CARTESIAN_POINT('Ctrl Pts',(37.5,3.83741678103717,32.1719479119405));
#35469=CARTESIAN_POINT('Origin',(37.75,0.,0.));
#35470=CARTESIAN_POINT('Ctrl Pts',(38.0021093499888,15.1841362142249,29.2991567049652));
#35471=CARTESIAN_POINT('Ctrl Pts',(37.8357506665066,15.0841362838781,29.1259188005427));
#35472=CARTESIAN_POINT('Ctrl Pts',(37.6692050584524,14.9840245993129,28.9524909653521));
#35473=CARTESIAN_POINT('Ctrl Pts',(37.5025598114679,14.8838564824963,28.7789704986351));
#35474=CARTESIAN_POINT('Origin',(37.75,0.,0.));
#35475=CARTESIAN_POINT('Origin',(36.8,27.2943217538007,27.2943217538007));
#35476=CARTESIAN_POINT('Origin',(37.75,0.,0.));
#35477=CARTESIAN_POINT('Ctrl Pts',(38.0020193561148,27.7994139997877,17.7817681968561));
#35478=CARTESIAN_POINT('Ctrl Pts',(37.8356549036385,27.6261918543793,17.6817410994361));
#35479=CARTESIAN_POINT('Ctrl Pts',(37.6691041509156,27.4527780511184,17.5816052376131));
#35480=CARTESIAN_POINT('Ctrl Pts',(37.5024547303958,27.2792691849716,17.4814171457626));
#35481=CARTESIAN_POINT('Origin',(37.75,0.,0.));
#35482=CARTESIAN_POINT('Origin',(36.8,37.284736894758,9.9904151409573));
#35483=CARTESIAN_POINT('Origin',(37.75,0.,0.));
#35484=CARTESIAN_POINT('Ctrl Pts',(38.0015719566141,32.9658822396214,1.49985854343197));
#35485=CARTESIAN_POINT('Ctrl Pts',(37.8351948506466,32.7658537908251,1.49984891222424));
#35486=CARTESIAN_POINT('Ctrl Pts',(37.6686397502838,32.5656049542639,1.49983991459913));
#35487=CARTESIAN_POINT('Ctrl Pts',(37.5019970368724,32.3652476458238,1.49983187417045));
#35488=CARTESIAN_POINT('Origin',(37.75,0.,0.));
#35489=CARTESIAN_POINT('Origin',(52.1,0.,0.));
#35490=CARTESIAN_POINT('',(51.6,-8.5,-1.04094977927525E-15));
#35491=CARTESIAN_POINT('Origin',(51.6,0.,0.));
#35492=CARTESIAN_POINT('',(52.6,-8.5,-1.04094977927525E-15));
#35493=CARTESIAN_POINT('',(52.1,-8.5,-1.04094977927525E-15));
#35494=CARTESIAN_POINT('Origin',(52.6,0.,0.));
#35495=CARTESIAN_POINT('Origin',(51.6,9.7,0.));
#35496=CARTESIAN_POINT('Origin',(52.6,8.5,0.));
#35497=CARTESIAN_POINT('',(52.6,-9.2,-1.12667505521557E-15));
#35498=CARTESIAN_POINT('Origin',(52.6,0.,0.));
#35499=CARTESIAN_POINT('Origin',(49.75,0.,0.));
#35500=CARTESIAN_POINT('',(55.1,-9.2,-1.12667505521557E-15));
#35501=CARTESIAN_POINT('Origin',(55.1,0.,0.));
#35502=CARTESIAN_POINT('',(49.75,-9.2,-1.12667505521557E-15));
#35503=CARTESIAN_POINT('Origin',(48.825,0.,0.));
#35504=CARTESIAN_POINT('',(48.825,-7.7,-9.42978035343462E-16));
#35505=CARTESIAN_POINT('Origin',(6.9,25.9807621135332,-15.));
#35506=CARTESIAN_POINT('',(6.9,28.7358750109634,8.61681422303452));
#35507=CARTESIAN_POINT('Ctrl Pts',(6.9,10.3676856018661,3.76156693666918));
#35508=CARTESIAN_POINT('Ctrl Pts',(6.9,14.103554168739,4.66834435251375));
#35509=CARTESIAN_POINT('Ctrl Pts',(6.90000000166257,18.0191477848531,5.70305252110769));
#35510=CARTESIAN_POINT('Ctrl Pts',(6.90000000166257,23.666490663791,7.22296038005705));
#35511=CARTESIAN_POINT('Ctrl Pts',(6.9,26.2182182108371,7.92134750786925));
#35512=CARTESIAN_POINT('Ctrl Pts',(6.9,28.7358750109634,8.61681422303452));
#35513=CARTESIAN_POINT('Origin',(6.9,0.,0.));
#35514=CARTESIAN_POINT('Origin',(40.9,7.79422863405994,-4.5));
#35515=CARTESIAN_POINT('Ctrl Pts',(40.9,30.5996231131986,-15.9346498339374));
#35516=CARTESIAN_POINT('Ctrl Pts',(40.9,30.1661818974695,-15.6844024313584));
#35517=CARTESIAN_POINT('Ctrl Pts',(40.9,29.7327406817405,-15.4341550287793));
#35518=CARTESIAN_POINT('Ctrl Pts',(40.9,29.2992994660114,-15.1839076262003));
#35519=CARTESIAN_POINT('Ctrl Pts',(30.5,29.5001797522422,-18.8345266621011));
#35520=CARTESIAN_POINT('Ctrl Pts',(30.5,29.9204226682664,-18.176307754627));
#35521=CARTESIAN_POINT('Ctrl Pts',(30.5,30.3108891324553,-17.5));
#35522=CARTESIAN_POINT('Ctrl Pts',(30.5,47.8108891324553,12.8108891324553));
#35523=CARTESIAN_POINT('Ctrl Pts',(30.5,17.5,30.3108891324553));
#35524=CARTESIAN_POINT('Ctrl Pts',(30.5,-12.8108891324553,47.8108891324553));
#35525=CARTESIAN_POINT('Ctrl Pts',(30.5,-30.3108891324553,17.5));
#35526=CARTESIAN_POINT('Ctrl Pts',(30.5,-47.8108891324553,-12.8108891324553));
#35527=CARTESIAN_POINT('Ctrl Pts',(30.5,-17.5,-30.3108891324553));
#35528=CARTESIAN_POINT('Ctrl Pts',(30.5,11.4877949884694,-47.0470003722618));
#35529=CARTESIAN_POINT('Ctrl Pts',(30.5,29.5001797522422,-18.8345266621011));
#35530=CARTESIAN_POINT('Ctrl Pts',(30.3311478274255,29.4365936489566,-18.7939298193791));
#35531=CARTESIAN_POINT('Ctrl Pts',(30.3311478274255,29.8559307532302,-18.1371296685291));
#35532=CARTESIAN_POINT('Ctrl Pts',(30.3311478274255,30.245555587262,-17.4622796600955));
#35533=CARTESIAN_POINT('Ctrl Pts',(30.3311478274255,47.7078352473574,12.7832759271664));
#35534=CARTESIAN_POINT('Ctrl Pts',(30.3311478274255,17.4622796600955,30.245555587262));
#35535=CARTESIAN_POINT('Ctrl Pts',(30.3311478274255,-12.7832759271664,47.7078352473574));
#35536=CARTESIAN_POINT('Ctrl Pts',(30.3311478274255,-30.245555587262,17.4622796600955));
#35537=CARTESIAN_POINT('Ctrl Pts',(30.3311478274255,-47.7078352473574,-12.7832759271664));
#35538=CARTESIAN_POINT('Ctrl Pts',(30.3311478274255,-17.4622796600955,-30.245555587262));
#35539=CARTESIAN_POINT('Ctrl Pts',(30.3311478274255,11.4630336437997,-46.9455930096601));
#35540=CARTESIAN_POINT('Ctrl Pts',(30.3311478274255,29.4365936489566,-18.7939298193791));
#35541=CARTESIAN_POINT('Ctrl Pts',(29.9897712690917,29.3077924996107,-18.7116961278613));
#35542=CARTESIAN_POINT('Ctrl Pts',(29.9897712690917,29.7252947753835,-18.0577698358324));
#35543=CARTESIAN_POINT('Ctrl Pts',(29.9897712690917,30.1132147882992,-17.3858726641896));
#35544=CARTESIAN_POINT('Ctrl Pts',(29.9897712690917,47.4990874524888,12.7273421241096));
#35545=CARTESIAN_POINT('Ctrl Pts',(29.9897712690917,17.3858726641896,30.1132147882992));
#35546=CARTESIAN_POINT('Ctrl Pts',(29.9897712690917,-12.7273421241096,47.4990874524888));
#35547=CARTESIAN_POINT('Ctrl Pts',(29.9897712690917,-30.1132147882992,17.3858726641896));
#35548=CARTESIAN_POINT('Ctrl Pts',(29.9897712690917,-47.4990874524888,-12.7273421241096));
#35549=CARTESIAN_POINT('Ctrl Pts',(29.9897712690917,-17.3858726641896,-30.1132147882992));
#35550=CARTESIAN_POINT('Ctrl Pts',(29.9897712690917,11.4128766206768,-46.7401804402414));
#35551=CARTESIAN_POINT('Ctrl Pts',(29.9897712690917,29.3077924996107,-18.7116961278613));
#35552=CARTESIAN_POINT('Ctrl Pts',(29.4666899049319,29.1097034403905,-18.5852252487451));
#35553=CARTESIAN_POINT('Ctrl Pts',(29.4666899049319,29.5243838511923,-17.935718792976));
#35554=CARTESIAN_POINT('Ctrl Pts',(29.4666899049319,29.9096819433198,-17.2683629213518));
#35555=CARTESIAN_POINT('Ctrl Pts',(29.4666899049319,47.1780448646716,12.641319021968));
#35556=CARTESIAN_POINT('Ctrl Pts',(29.4666899049319,17.2683629213518,29.9096819433198));
#35557=CARTESIAN_POINT('Ctrl Pts',(29.4666899049319,-12.641319021968,47.1780448646716));
#35558=CARTESIAN_POINT('Ctrl Pts',(29.4666899049319,-29.9096819433198,17.2683629213518));
#35559=CARTESIAN_POINT('Ctrl Pts',(29.4666899049319,-47.1780448646716,-12.641319021968));
#35560=CARTESIAN_POINT('Ctrl Pts',(29.4666899049319,-17.2683629213518,-29.9096819433198));
#35561=CARTESIAN_POINT('Ctrl Pts',(29.4666899049319,11.3357378872557,-46.4242672450966));
#35562=CARTESIAN_POINT('Ctrl Pts',(29.4666899049319,29.1097034403905,-18.5852252487451));
#35563=CARTESIAN_POINT('Ctrl Pts',(28.7471241621752,28.8357745030392,-18.4103340474916));
#35564=CARTESIAN_POINT('Ctrl Pts',(28.7471241621752,29.246552676757,-17.7669395953572));
#35565=CARTESIAN_POINT('Ctrl Pts',(28.7471241621752,29.6282250261092,-17.105863694435));
#35566=CARTESIAN_POINT('Ctrl Pts',(28.7471241621752,46.7340887205442,12.5223613316742));
#35567=CARTESIAN_POINT('Ctrl Pts',(28.7471241621752,17.105863694435,29.6282250261092));
#35568=CARTESIAN_POINT('Ctrl Pts',(28.7471241621752,-12.5223613316742,46.7340887205442));
#35569=CARTESIAN_POINT('Ctrl Pts',(28.7471241621752,-29.6282250261092,17.105863694435));
#35570=CARTESIAN_POINT('Ctrl Pts',(28.7471241621752,-46.7340887205442,-12.5223613316742));
#35571=CARTESIAN_POINT('Ctrl Pts',(28.7471241621752,-17.105863694435,-29.6282250261092));
#35572=CARTESIAN_POINT('Ctrl Pts',(28.7471241621752,11.2290660127069,-45.9874043199967));
#35573=CARTESIAN_POINT('Ctrl Pts',(28.7471241621752,28.8357745030392,-18.4103340474916));
#35574=CARTESIAN_POINT('Ctrl Pts',(27.8100958442934,28.4776836217162,-18.1817092625453));
#35575=CARTESIAN_POINT('Ctrl Pts',(27.8100958442934,28.8833606347823,-17.5463046664274));
#35576=CARTESIAN_POINT('Ctrl Pts',(27.8100958442934,29.2602932679205,-16.8934381948013));
#35577=CARTESIAN_POINT('Ctrl Pts',(27.8100958442934,46.1537314627218,12.3668550731192));
#35578=CARTESIAN_POINT('Ctrl Pts',(27.8100958442934,16.8934381948013,29.2602932679205));
#35579=CARTESIAN_POINT('Ctrl Pts',(27.8100958442934,-12.3668550731192,46.1537314627218));
#35580=CARTESIAN_POINT('Ctrl Pts',(27.8100958442934,-29.2602932679205,16.8934381948013));
#35581=CARTESIAN_POINT('Ctrl Pts',(27.8100958442934,-46.1537314627218,-12.3668550731192));
#35582=CARTESIAN_POINT('Ctrl Pts',(27.8100958442934,-16.8934381948013,-29.2602932679205));
#35583=CARTESIAN_POINT('Ctrl Pts',(27.8100958442934,11.0896202647003,-45.4163196022628));
#35584=CARTESIAN_POINT('Ctrl Pts',(27.8100958442934,28.4776836217162,-18.1817092625453));
#35585=CARTESIAN_POINT('Ctrl Pts',(26.8343111708818,28.1064299010669,-17.9446806017473));
#35586=CARTESIAN_POINT('Ctrl Pts',(26.8343111708818,28.5068182430991,-17.3175595557791));
#35587=CARTESIAN_POINT('Ctrl Pts',(26.8343111708818,28.8788369357517,-16.6732042787396));
#35588=CARTESIAN_POINT('Ctrl Pts',(26.8343111708818,45.5520412144912,12.2056326570121));
#35589=CARTESIAN_POINT('Ctrl Pts',(26.8343111708818,16.6732042787396,28.8788369357517));
#35590=CARTESIAN_POINT('Ctrl Pts',(26.8343111708818,-12.2056326570121,45.5520412144912));
#35591=CARTESIAN_POINT('Ctrl Pts',(26.8343111708818,-28.8788369357517,16.6732042787396));
#35592=CARTESIAN_POINT('Ctrl Pts',(26.8343111708818,-45.5520412144912,-12.2056326570121));
#35593=CARTESIAN_POINT('Ctrl Pts',(26.8343111708818,-16.6732042787396,-28.8788369357517));
#35594=CARTESIAN_POINT('Ctrl Pts',(26.8343111708818,10.9450487174303,-44.8242427376375));
#35595=CARTESIAN_POINT('Ctrl Pts',(26.8343111708818,28.1064299010669,-17.9446806017473));
#35596=CARTESIAN_POINT('Ctrl Pts',(25.8181479469611,27.7272550606068,-17.7025946652472));
#35597=CARTESIAN_POINT('Ctrl Pts',(25.8181479469611,28.1222418918016,-17.0839339083798));
#35598=CARTESIAN_POINT('Ctrl Pts',(25.8181479469611,28.4892417994668,-16.4482714219305));
#35599=CARTESIAN_POINT('Ctrl Pts',(25.8181479469611,44.9375132213974,12.0409703775363));
#35600=CARTESIAN_POINT('Ctrl Pts',(25.8181479469611,16.4482714219305,28.4892417994668));
#35601=CARTESIAN_POINT('Ctrl Pts',(25.8181479469611,-12.0409703775363,44.9375132213974));
#35602=CARTESIAN_POINT('Ctrl Pts',(25.8181479469611,-28.4892417994668,16.4482714219305));
#35603=CARTESIAN_POINT('Ctrl Pts',(25.8181479469611,-44.9375132213974,-12.0409703775363));
#35604=CARTESIAN_POINT('Ctrl Pts',(25.8181479469611,-16.4482714219305,-28.4892417994668));
#35605=CARTESIAN_POINT('Ctrl Pts',(25.8181479469611,10.7973925719907,-44.2195332406074));
#35606=CARTESIAN_POINT('Ctrl Pts',(25.8181479469611,27.7272550606068,-17.7025946652472));
#35607=CARTESIAN_POINT('Ctrl Pts',(24.7595197917227,27.3496265541183,-17.4614959928472));
#35608=CARTESIAN_POINT('Ctrl Pts',(24.7595197917227,27.739233902677,-16.8512610227058));
#35609=CARTESIAN_POINT('Ctrl Pts',(24.7595197917227,28.1012354927406,-16.2242558762949));
#35610=CARTESIAN_POINT('Ctrl Pts',(24.7595197917227,44.3254913690355,11.8769796164457));
#35611=CARTESIAN_POINT('Ctrl Pts',(24.7595197917227,16.2242558762949,28.1012354927406));
#35612=CARTESIAN_POINT('Ctrl Pts',(24.7595197917227,-11.8769796164457,44.3254913690355));
#35613=CARTESIAN_POINT('Ctrl Pts',(24.7595197917227,-28.1012354927406,16.2242558762949));
#35614=CARTESIAN_POINT('Ctrl Pts',(24.7595197917227,-44.3254913690355,-11.8769796164457));
#35615=CARTESIAN_POINT('Ctrl Pts',(24.7595197917227,-16.2242558762949,-28.1012354927406));
#35616=CARTESIAN_POINT('Ctrl Pts',(24.7595197917227,10.6503385912768,-43.6172898429552));
#35617=CARTESIAN_POINT('Ctrl Pts',(24.7595197917227,27.3496265541183,-17.4614959928472));
#35618=CARTESIAN_POINT('Ctrl Pts',(23.6563574780851,26.9860278023044,-17.229354682426));
#35619=CARTESIAN_POINT('Ctrl Pts',(23.6563574780851,27.370455528196,-16.627232461942));
#35620=CARTESIAN_POINT('Ctrl Pts',(23.6563574780851,27.7276444994825,-16.0085630157705));
#35621=CARTESIAN_POINT('Ctrl Pts',(23.6563574780851,43.736207515253,11.719081483712));
#35622=CARTESIAN_POINT('Ctrl Pts',(23.6563574780851,16.0085630157705,27.7276444994825));
#35623=CARTESIAN_POINT('Ctrl Pts',(23.6563574780851,-11.719081483712,43.736207515253));
#35624=CARTESIAN_POINT('Ctrl Pts',(23.6563574780851,-27.7276444994825,16.0085630157705));
#35625=CARTESIAN_POINT('Ctrl Pts',(23.6563574780851,-43.736207515253,-11.719081483712));
#35626=CARTESIAN_POINT('Ctrl Pts',(23.6563574780851,-16.0085630157705,-27.7276444994825));
#35627=CARTESIAN_POINT('Ctrl Pts',(23.6563574780851,10.5087479991522,-43.0374211521332));
#35628=CARTESIAN_POINT('Ctrl Pts',(23.6563574780851,26.9860278023044,-17.229354682426));
#35629=CARTESIAN_POINT('Ctrl Pts',(22.5073180101405,26.649565639321,-17.0145388530744));
#35630=CARTESIAN_POINT('Ctrl Pts',(22.5073180101405,27.029200315079,-16.419923900654));
#35631=CARTESIAN_POINT('Ctrl Pts',(22.5073180101405,27.3819358493961,-15.8089680335819));
#35632=CARTESIAN_POINT('Ctrl Pts',(22.5073180101405,43.190903882978,11.5729678158142));
#35633=CARTESIAN_POINT('Ctrl Pts',(22.5073180101405,15.8089680335819,27.3819358493961));
#35634=CARTESIAN_POINT('Ctrl Pts',(22.5073180101405,-11.5729678158142,43.190903882978));
#35635=CARTESIAN_POINT('Ctrl Pts',(22.5073180101405,-27.3819358493961,15.8089680335819));
#35636=CARTESIAN_POINT('Ctrl Pts',(22.5073180101405,-43.190903882978,-11.5729678158142));
#35637=CARTESIAN_POINT('Ctrl Pts',(22.5073180101405,-15.8089680335819,-27.3819358493961));
#35638=CARTESIAN_POINT('Ctrl Pts',(22.5073180101405,10.3777247856603,-42.5008299977716));
#35639=CARTESIAN_POINT('Ctrl Pts',(22.5073180101405,26.649565639321,-17.0145388530744));
#35640=CARTESIAN_POINT('Ctrl Pts',(21.3125219557939,26.3518679613905,-16.8244723890963));
#35641=CARTESIAN_POINT('Ctrl Pts',(21.3125219557939,26.727261803997,-16.2364997772301));
#35642=CARTESIAN_POINT('Ctrl Pts',(21.3125219557939,27.0760569908086,-15.632368792237));
#35643=CARTESIAN_POINT('Ctrl Pts',(21.3125219557939,42.7084257830456,11.4436881985716));
#35644=CARTESIAN_POINT('Ctrl Pts',(21.3125219557939,15.632368792237,27.0760569908086));
#35645=CARTESIAN_POINT('Ctrl Pts',(21.3125219557939,-11.4436881985716,42.7084257830456));
#35646=CARTESIAN_POINT('Ctrl Pts',(21.3125219557939,-27.0760569908086,15.632368792237));
#35647=CARTESIAN_POINT('Ctrl Pts',(21.3125219557939,-42.7084257830456,-11.4436881985716));
#35648=CARTESIAN_POINT('Ctrl Pts',(21.3125219557939,-15.632368792237,-27.0760569908086));
#35649=CARTESIAN_POINT('Ctrl Pts',(21.3125219557939,10.2617970211066,-42.0260605935833));
#35650=CARTESIAN_POINT('Ctrl Pts',(21.3125219557939,26.3518679613905,-16.8244723890963));
#35651=CARTESIAN_POINT('Ctrl Pts',(20.0742472323676,26.1010282252799,-16.6643225955233));
#35652=CARTESIAN_POINT('Ctrl Pts',(20.0742472323676,26.4728487465358,-16.0819468125049));
#35653=CARTESIAN_POINT('Ctrl Pts',(20.0742472323676,26.8183238008715,-15.4835664656478));
#35654=CARTESIAN_POINT('Ctrl Pts',(20.0742472323676,42.3018902665193,11.3347573352238));
#35655=CARTESIAN_POINT('Ctrl Pts',(20.0742472323676,15.4835664656478,26.8183238008715));
#35656=CARTESIAN_POINT('Ctrl Pts',(20.0742472323676,-11.3347573352238,42.3018902665193));
#35657=CARTESIAN_POINT('Ctrl Pts',(20.0742472323676,-26.8183238008715,15.4835664656478));
#35658=CARTESIAN_POINT('Ctrl Pts',(20.0742472323676,-42.3018902665193,-11.3347573352238));
#35659=CARTESIAN_POINT('Ctrl Pts',(20.0742472323676,-15.4835664656478,-26.8183238008715));
#35660=CARTESIAN_POINT('Ctrl Pts',(20.0742472323676,10.1641164141543,-41.6260204156154));
#35661=CARTESIAN_POINT('Ctrl Pts',(20.0742472323676,26.1010282252799,-16.6643225955233));
#35662=CARTESIAN_POINT('Ctrl Pts',(18.7979917002302,25.8989065200918,-16.5352770548748));
#35663=CARTESIAN_POINT('Ctrl Pts',(18.7979917002302,26.2678477295776,-15.9574110860028));
#35664=CARTESIAN_POINT('Ctrl Pts',(18.7979917002302,26.6106474867381,-15.3636644897785));
#35665=CARTESIAN_POINT('Ctrl Pts',(18.7979917002302,41.9743119765166,11.2469829969596));
#35666=CARTESIAN_POINT('Ctrl Pts',(18.7979917002302,15.3636644897785,26.6106474867381));
#35667=CARTESIAN_POINT('Ctrl Pts',(18.7979917002302,-11.2469829969596,41.9743119765166));
#35668=CARTESIAN_POINT('Ctrl Pts',(18.7979917002302,-26.6106474867381,15.3636644897785));
#35669=CARTESIAN_POINT('Ctrl Pts',(18.7979917002302,-41.9743119765166,-11.2469829969596));
#35670=CARTESIAN_POINT('Ctrl Pts',(18.7979917002302,-15.3636644897785,-26.6106474867381));
#35671=CARTESIAN_POINT('Ctrl Pts',(18.7979917002302,10.0854073102973,-41.303675941138));
#35672=CARTESIAN_POINT('Ctrl Pts',(18.7979917002302,25.8989065200918,-16.5352770548748));
#35673=CARTESIAN_POINT('Ctrl Pts',(17.4917404060759,25.7420647185138,-16.4351406788133));
#35674=CARTESIAN_POINT('Ctrl Pts',(17.4917404060759,26.1087716481884,-15.8607742221527));
#35675=CARTESIAN_POINT('Ctrl Pts',(17.4917404060759,26.4494954361781,-15.2706233100072));
#35676=CARTESIAN_POINT('Ctrl Pts',(17.4917404060759,41.7201187461852,11.1788721261709));
#35677=CARTESIAN_POINT('Ctrl Pts',(17.4917404060759,15.2706233100072,26.4494954361781));
#35678=CARTESIAN_POINT('Ctrl Pts',(17.4917404060759,-11.1788721261709,41.7201187461852));
#35679=CARTESIAN_POINT('Ctrl Pts',(17.4917404060759,-26.4494954361781,15.2706233100072));
#35680=CARTESIAN_POINT('Ctrl Pts',(17.4917404060759,-41.7201187461852,-11.1788721261709));
#35681=CARTESIAN_POINT('Ctrl Pts',(17.4917404060759,-15.2706233100072,-26.4494954361781));
#35682=CARTESIAN_POINT('Ctrl Pts',(17.4917404060759,10.0243308532288,-41.0535440314616));
#35683=CARTESIAN_POINT('Ctrl Pts',(17.4917404060759,25.7420647185138,-16.4351406788133));
#35684=CARTESIAN_POINT('Ctrl Pts',(16.1647270995715,25.6237637373094,-16.3596108683728));
#35685=CARTESIAN_POINT('Ctrl Pts',(16.1647270995715,25.988785417954,-15.7878839869031));
#35686=CARTESIAN_POINT('Ctrl Pts',(16.1647270995715,26.3279433657953,-15.2004451894512));
#35687=CARTESIAN_POINT('Ctrl Pts',(16.1647270995715,41.5283885552464,11.1274981763441));
#35688=CARTESIAN_POINT('Ctrl Pts',(16.1647270995715,15.2004451894512,26.3279433657953));
#35689=CARTESIAN_POINT('Ctrl Pts',(16.1647270995715,-11.1274981763441,41.5283885552464));
#35690=CARTESIAN_POINT('Ctrl Pts',(16.1647270995715,-26.3279433657953,15.2004451894512));
#35691=CARTESIAN_POINT('Ctrl Pts',(16.1647270995715,-41.5283885552464,-11.1274981763441));
#35692=CARTESIAN_POINT('Ctrl Pts',(16.1647270995715,-15.2004451894512,-26.3279433657953));
#35693=CARTESIAN_POINT('Ctrl Pts',(16.1647270995715,9.97826274685029,-40.8648771706659));
#35694=CARTESIAN_POINT('Ctrl Pts',(16.1647270995715,25.6237637373094,-16.3596108683728));
#35695=CARTESIAN_POINT('Ctrl Pts',(14.8263876417415,25.5355400760542,-16.3032840624315));
#35696=CARTESIAN_POINT('Ctrl Pts',(14.8263876417415,25.8993049721986,-15.7335256598799));
#35697=CARTESIAN_POINT('Ctrl Pts',(14.8263876417415,26.2372951854241,-15.1481094381123));
#35698=CARTESIAN_POINT('Ctrl Pts',(14.8263876417415,41.3854046235364,11.0891857473118));
#35699=CARTESIAN_POINT('Ctrl Pts',(14.8263876417415,15.1481094381123,26.2372951854241));
#35700=CARTESIAN_POINT('Ctrl Pts',(14.8263876417415,-11.0891857473118,41.3854046235364));
#35701=CARTESIAN_POINT('Ctrl Pts',(14.8263876417415,-26.2372951854241,15.1481094381123));
#35702=CARTESIAN_POINT('Ctrl Pts',(14.8263876417415,-41.3854046235364,-11.0891857473118));
#35703=CARTESIAN_POINT('Ctrl Pts',(14.8263876417415,-15.1481094381123,-26.2372951854241));
#35704=CARTESIAN_POINT('Ctrl Pts',(14.8263876417415,9.94390718216752,-40.7241777356532));
#35705=CARTESIAN_POINT('Ctrl Pts',(14.8263876417415,25.5355400760542,-16.3032840624315));
#35706=CARTESIAN_POINT('Ctrl Pts',(13.4853470903953,25.4687774591536,-16.260659159851));
#35707=CARTESIAN_POINT('Ctrl Pts',(13.4853470903953,25.8315912927267,-15.6923903894687));
#35708=CARTESIAN_POINT('Ctrl Pts',(13.4853470903953,26.1686978312363,-15.1085047372063));
#35709=CARTESIAN_POINT('Ctrl Pts',(13.4853470903953,41.2772025684426,11.06019309403));
#35710=CARTESIAN_POINT('Ctrl Pts',(13.4853470903953,15.1085047372063,26.1686978312363));
#35711=CARTESIAN_POINT('Ctrl Pts',(13.4853470903953,-11.06019309403,41.2772025684426));
#35712=CARTESIAN_POINT('Ctrl Pts',(13.4853470903953,-26.1686978312363,15.1085047372063));
#35713=CARTESIAN_POINT('Ctrl Pts',(13.4853470903953,-41.2772025684426,-11.06019309403));
#35714=CARTESIAN_POINT('Ctrl Pts',(13.4853470903953,-15.1085047372063,-26.1686978312363));
#35715=CARTESIAN_POINT('Ctrl Pts',(13.4853470903953,9.91790885733393,-40.617704456895));
#35716=CARTESIAN_POINT('Ctrl Pts',(13.4853470903953,25.4687774591536,-16.260659159851));
#35717=CARTESIAN_POINT('Ctrl Pts',(12.1482076787549,25.4164718226475,-16.2272643834928));
#35718=CARTESIAN_POINT('Ctrl Pts',(12.1482076787549,25.778540539635,-15.660162675793));
#35719=CARTESIAN_POINT('Ctrl Pts',(12.1482076787549,26.1149547570431,-15.0774761588537));
#35720=CARTESIAN_POINT('Ctrl Pts',(12.1482076787549,41.1924309158968,11.0374785981893));
#35721=CARTESIAN_POINT('Ctrl Pts',(12.1482076787549,15.0774761588537,26.1149547570431));
#35722=CARTESIAN_POINT('Ctrl Pts',(12.1482076787549,-11.0374785981893,41.1924309158968));
#35723=CARTESIAN_POINT('Ctrl Pts',(12.1482076787549,-26.1149547570431,15.0774761588537));
#35724=CARTESIAN_POINT('Ctrl Pts',(12.1482076787549,-41.1924309158968,-11.0374785981893));
#35725=CARTESIAN_POINT('Ctrl Pts',(12.1482076787549,-15.0774761588537,-26.1149547570431));
#35726=CARTESIAN_POINT('Ctrl Pts',(12.1482076787549,9.89754028893977,-40.534287226192));
#35727=CARTESIAN_POINT('Ctrl Pts',(12.1482076787549,25.4164718226475,-16.2272643834928));
#35728=CARTESIAN_POINT('Ctrl Pts',(10.8190675759626,25.3740740708084,-16.2001953420791));
#35729=CARTESIAN_POINT('Ctrl Pts',(10.8190675759626,25.7355388133451,-15.6340396286792));
#35730=CARTESIAN_POINT('Ctrl Pts',(10.8190675759626,26.0713918511132,-15.0523251033885));
#35731=CARTESIAN_POINT('Ctrl Pts',(10.8190675759626,41.1237169545017,11.0190667477248));
#35732=CARTESIAN_POINT('Ctrl Pts',(10.8190675759626,15.0523251033885,26.0713918511132));
#35733=CARTESIAN_POINT('Ctrl Pts',(10.8190675759626,-11.0190667477248,41.1237169545017));
#35734=CARTESIAN_POINT('Ctrl Pts',(10.8190675759626,-26.0713918511132,15.0523251033885));
#35735=CARTESIAN_POINT('Ctrl Pts',(10.8190675759626,-41.1237169545017,-11.0190667477248));
#35736=CARTESIAN_POINT('Ctrl Pts',(10.8190675759626,-15.0523251033885,-26.0713918511132));
#35737=CARTESIAN_POINT('Ctrl Pts',(10.8190675759626,9.88102999357242,-40.4666711281441));
#35738=CARTESIAN_POINT('Ctrl Pts',(10.8190675759626,25.3740740708084,-16.2001953420791));
#35739=CARTESIAN_POINT('Ctrl Pts',(9.50027713254189,25.3387651379321,-16.1776521900286));
#35740=CARTESIAN_POINT('Ctrl Pts',(9.50027713254189,25.6997268893331,-15.6122843025816));
#35741=CARTESIAN_POINT('Ctrl Pts',(9.50027713254189,26.0351125755702,-15.0313792538877));
#35742=CARTESIAN_POINT('Ctrl Pts',(9.50027713254189,41.0664918294579,11.0037333216825));
#35743=CARTESIAN_POINT('Ctrl Pts',(9.50027713254189,15.0313792538877,26.0351125755702));
#35744=CARTESIAN_POINT('Ctrl Pts',(9.5002771325419,-11.0037333216825,41.0664918294579));
#35745=CARTESIAN_POINT('Ctrl Pts',(9.5002771325419,-26.0351125755702,15.0313792538877));
#35746=CARTESIAN_POINT('Ctrl Pts',(9.5002771325419,-41.0664918294579,-11.0037333216825));
#35747=CARTESIAN_POINT('Ctrl Pts',(9.50027713254189,-15.0313792538877,-26.0351125755702));
#35748=CARTESIAN_POINT('Ctrl Pts',(9.50027713254189,9.86728018643389,-40.4103603059007));
#35749=CARTESIAN_POINT('Ctrl Pts',(9.50027713254189,25.3387651379321,-16.1776521900286));
#35750=CARTESIAN_POINT('Ctrl Pts',(8.45435372222587,25.3150436214797,-16.1625070777669));
#35751=CARTESIAN_POINT('Ctrl Pts',(8.45435372222587,25.6756674495416,-15.5976684735573));
#35752=CARTESIAN_POINT('Ctrl Pts',(8.45435372222587,26.0107391561104,-15.0173072536015));
#35753=CARTESIAN_POINT('Ctrl Pts',(8.45435372222587,41.0280464097118,10.9934319025089));
#35754=CARTESIAN_POINT('Ctrl Pts',(8.45435372222587,15.0173072536015,26.0107391561104));
#35755=CARTESIAN_POINT('Ctrl Pts',(8.45435372222587,-10.9934319025089,41.0280464097118));
#35756=CARTESIAN_POINT('Ctrl Pts',(8.45435372222587,-26.0107391561104,15.0173072536015));
#35757=CARTESIAN_POINT('Ctrl Pts',(8.45435372222587,-41.0280464097118,-10.9934319025089));
#35758=CARTESIAN_POINT('Ctrl Pts',(8.45435372222587,-15.0173072536015,-26.0107391561104));
#35759=CARTESIAN_POINT('Ctrl Pts',(8.45435372222587,9.85804268618443,-40.3725291400319));
#35760=CARTESIAN_POINT('Ctrl Pts',(8.45435372222587,25.3150436214797,-16.1625070777669));
#35761=CARTESIAN_POINT('Ctrl Pts',(7.67514864245731,25.2995613842179,-16.1526223715399));
#35762=CARTESIAN_POINT('Ctrl Pts',(7.67514864245731,25.6599646610633,-15.5881292127269));
#35763=CARTESIAN_POINT('Ctrl Pts',(7.67514864245731,25.9948314436453,-15.0081229315276));
#35764=CARTESIAN_POINT('Ctrl Pts',(7.67514864245731,41.0029543751729,10.9867085121177));
#35765=CARTESIAN_POINT('Ctrl Pts',(7.67514864245731,15.0081229315276,25.9948314436453));
#35766=CARTESIAN_POINT('Ctrl Pts',(7.67514864245731,-10.9867085121177,41.0029543751729));
#35767=CARTESIAN_POINT('Ctrl Pts',(7.67514864245731,-25.9948314436453,15.0081229315276));
#35768=CARTESIAN_POINT('Ctrl Pts',(7.67514864245731,-41.0029543751729,-10.9867085121177));
#35769=CARTESIAN_POINT('Ctrl Pts',(7.67514864245731,-15.0081229315276,-25.9948314436453));
#35770=CARTESIAN_POINT('Ctrl Pts',(7.67514864245731,9.85201367995056,-40.3478380083732));
#35771=CARTESIAN_POINT('Ctrl Pts',(7.67514864245731,25.2995613842179,-16.1526223715399));
#35772=CARTESIAN_POINT('Ctrl Pts',(7.15799654185577,25.2902623130707,-16.1466853364124));
#35773=CARTESIAN_POINT('Ctrl Pts',(7.15799654185577,25.6505331205953,-15.5823996619098));
#35774=CARTESIAN_POINT('Ctrl Pts',(7.15799654185577,25.9852768200144,-15.0026065670023));
#35775=CARTESIAN_POINT('Ctrl Pts',(7.15799654185577,40.9878833870167,10.9826702530121));
#35776=CARTESIAN_POINT('Ctrl Pts',(7.15799654185577,15.0026065670023,25.9852768200144));
#35777=CARTESIAN_POINT('Ctrl Pts',(7.15799654185577,-10.9826702530121,40.9878833870167));
#35778=CARTESIAN_POINT('Ctrl Pts',(7.15799654185577,-25.9852768200144,15.0026065670023));
#35779=CARTESIAN_POINT('Ctrl Pts',(7.15799654185577,-40.9878833870167,-10.9826702530121));
#35780=CARTESIAN_POINT('Ctrl Pts',(7.15799654185577,-15.0026065670023,-25.9852768200144));
#35781=CARTESIAN_POINT('Ctrl Pts',(7.15799654185577,9.84839248767921,-40.3330078138659));
#35782=CARTESIAN_POINT('Ctrl Pts',(7.15799654185577,25.2902623130707,-16.1466853364124));
#35783=CARTESIAN_POINT('Ctrl Pts',(6.9,25.2858683590648,-16.1438799960867));
#35784=CARTESIAN_POINT('Ctrl Pts',(6.9,25.6460765727998,-15.5796923611089));
#35785=CARTESIAN_POINT('Ctrl Pts',(6.9,25.9807621135332,-15.));
#35786=CARTESIAN_POINT('Ctrl Pts',(6.9,40.9807621135332,10.9807621135331));
#35787=CARTESIAN_POINT('Ctrl Pts',(6.9,15.,25.9807621135332));
#35788=CARTESIAN_POINT('Ctrl Pts',(6.9,-10.9807621135331,40.9807621135332));
#35789=CARTESIAN_POINT('Ctrl Pts',(6.9,-25.9807621135332,15.));
#35790=CARTESIAN_POINT('Ctrl Pts',(6.9,-40.9807621135332,-10.9807621135331));
#35791=CARTESIAN_POINT('Ctrl Pts',(6.9,-15.,-25.9807621135332));
#35792=CARTESIAN_POINT('Ctrl Pts',(6.9,9.84668141868802,-40.3260003190816));
#35793=CARTESIAN_POINT('Ctrl Pts',(6.9,25.2858683590648,-16.1438799960867));
#35794=CARTESIAN_POINT('Ctrl Pts',(6.9,28.7358750109634,8.61681422303452));
#35795=CARTESIAN_POINT('Ctrl Pts',(7.85773098116326,29.3220126177434,6.72950262532882));
#35796=CARTESIAN_POINT('Ctrl Pts',(8.88781981167334,29.7139609348499,4.83176468807715));
#35797=CARTESIAN_POINT('Ctrl Pts',(10.5914578196776,30.0626260759601,1.83991777043966));
#35798=CARTESIAN_POINT('Ctrl Pts',(11.2365058953701,30.1308526921615,0.737334477600518));
#35799=CARTESIAN_POINT('Ctrl Pts',(12.0558885382926,30.1493644860168,-0.564998386426074));
#35800=CARTESIAN_POINT('Ctrl Pts',(12.1875764958397,30.1503477937894,-0.770798830274841));
#35801=CARTESIAN_POINT('Ctrl Pts',(13.194901830313,30.1433772121647,-2.32835059063961));
#35802=CARTESIAN_POINT('Ctrl Pts',(14.2258982134098,30.0606334052373,-3.91692083548089));
#35803=CARTESIAN_POINT('Ctrl Pts',(18.2616480823244,29.4024246647732,-8.94354621773405));
#35804=CARTESIAN_POINT('Ctrl Pts',(21.0496416709525,28.796919295079,-11.660889676038));
#35805=CARTESIAN_POINT('Ctrl Pts',(25.8000196361138,29.3778263502455,-14.7241675584603));
#35806=CARTESIAN_POINT('Ctrl Pts',(26.8976561124457,29.7353019177929,-15.1580512376427));
#35807=CARTESIAN_POINT('Ctrl Pts',(28.0045908801237,30.0977443108623,-15.5447817028247));
#35808=CARTESIAN_POINT('Ctrl Pts',(28.5235971652406,30.2828992744991,-15.6994510084801));
#35809=CARTESIAN_POINT('Ctrl Pts',(29.0834839543824,30.4804113157011,-15.8677990842846));
#35810=CARTESIAN_POINT('Ctrl Pts',(29.1146288039499,30.4913713634453,-15.877207296405));
#35811=CARTESIAN_POINT('Ctrl Pts',(29.5949306848436,30.6609898319163,-16.0210111630069));
#35812=CARTESIAN_POINT('Ctrl Pts',(30.0492939924726,30.8338536064743,-16.1312811324031));
#35813=CARTESIAN_POINT('Ctrl Pts',(30.5,31.0097594187194,-16.229443021655));
#35814=CARTESIAN_POINT('Ctrl Pts',(6.45331003273164,10.2495589536195,4.07387898226151));
#35815=CARTESIAN_POINT('Ctrl Pts',(7.20830533428676,10.4589493929845,3.54117612793134));
#35816=CARTESIAN_POINT('Ctrl Pts',(7.99943720515023,10.6278530262204,3.00808536723907));
#35817=CARTESIAN_POINT('Ctrl Pts',(9.76195392812149,10.8974188156737,1.87226624217412));
#35818=CARTESIAN_POINT('Ctrl Pts',(10.7319699357145,10.978614804603,1.2567580486118));
#35819=CARTESIAN_POINT('Ctrl Pts',(12.6618070777417,11.0581512103982,0.165209663835397));
#35820=CARTESIAN_POINT('Ctrl Pts',(13.6366888866736,11.0460663569154,-0.364704064273055));
#35821=CARTESIAN_POINT('Ctrl Pts',(15.55636942495,10.9884970038505,-1.27025231764747));
#35822=CARTESIAN_POINT('Ctrl Pts',(16.5294822240034,10.9232664847119,-1.69980161462952));
#35823=CARTESIAN_POINT('Ctrl Pts',(18.4405353898674,10.7982950788299,-2.41132585012622));
#35824=CARTESIAN_POINT('Ctrl Pts',(19.4148048972756,10.7128845485963,-2.74047342809724));
#35825=CARTESIAN_POINT('Ctrl Pts',(20.6320159197512,10.6248232626625,-3.07372863623309));
#35826=CARTESIAN_POINT('Ctrl Pts',(21.1045081958649,10.5890632628362,-3.19855905527614));
#35827=CARTESIAN_POINT('Ctrl Pts',(22.0534615876998,10.5175158204589,-3.42883778652051));
#35828=CARTESIAN_POINT('Ctrl Pts',(22.7823820470181,10.4664588970828,-3.58029681662341));
#35829=CARTESIAN_POINT('Ctrl Pts',(23.3297776630266,10.4341170945838,-3.67835397010643));
#35830=CARTESIAN_POINT('Ctrl Pts',(23.4470599317457,10.4271412460567,-3.69902619132824));
#35831=CARTESIAN_POINT('Ctrl Pts',(23.6811266122299,10.4133903945395,-3.73910834650869));
#35832=CARTESIAN_POINT('Ctrl Pts',(24.0941730950848,10.3895545652128,-3.80664723977491));
#35833=CARTESIAN_POINT('Ctrl Pts',(24.6899146335614,10.3570603924451,-3.89464075109997));
#35834=CARTESIAN_POINT('Ctrl Pts',(25.291236117096,10.3283061836387,-3.96994444386566));
#35835=CARTESIAN_POINT('Ctrl Pts',(25.773528518035,10.308597305488,-4.02162740546581));
#35836=CARTESIAN_POINT('Ctrl Pts',(26.0148283477099,10.3000025859217,-4.04448759176678));
#35837=CARTESIAN_POINT('Ctrl Pts',(26.5981242438443,10.2809495486037,-4.0960039723359));
#35838=CARTESIAN_POINT('Ctrl Pts',(27.5413774795629,10.2607319091993,-4.14752077886529));
#35839=CARTESIAN_POINT('Ctrl Pts',(28.5384263877913,10.2503835882543,-4.17105255246826));
#35840=CARTESIAN_POINT('Ctrl Pts',(29.1235503058367,10.244453382669,-4.18584784382924));
#35841=CARTESIAN_POINT('Ctrl Pts',(29.2812719873799,10.2430815653883,-4.18934848102508));
#35842=CARTESIAN_POINT('Ctrl Pts',(29.6033573831698,10.2409825864505,-4.19465178436652));
#35843=CARTESIAN_POINT('Ctrl Pts',(30.1682075695059,10.23904328544,-4.19956029863431));
#35844=CARTESIAN_POINT('Ctrl Pts',(31.3151152846707,10.2404426493561,-4.19601580459663));
#35845=CARTESIAN_POINT('Ctrl Pts',(32.3203773995796,10.2455622764132,-4.18330340731802));
#35846=CARTESIAN_POINT('Ctrl Pts',(33.1677006908682,10.2455713422049,-4.18329188254758));
#35847=CARTESIAN_POINT('Ctrl Pts',(33.494913285099,10.2455724350351,-4.18329063364475));
#35848=CARTESIAN_POINT('Ctrl Pts',(34.1541785734607,10.2455743198855,-4.18328832445806));
#35849=CARTESIAN_POINT('Ctrl Pts',(34.9761291047989,10.2455804319183,-4.18328098024986));
#35850=CARTESIAN_POINT('Ctrl Pts',(35.9637295000903,10.2455829874647,-4.18327789132126));
#35851=CARTESIAN_POINT('Ctrl Pts',(37.9383590406839,10.2455864680815,-4.18327370253669));
#35852=CARTESIAN_POINT('Ctrl Pts',(39.5833333333333,10.2456046429335,-4.18325179103929));
#35853=CARTESIAN_POINT('Ctrl Pts',(40.9,10.2456046429335,-4.18325179103929));
#35854=CARTESIAN_POINT('Ctrl Pts',(6.63336813585096,13.590868440034,4.85602971916216));
#35855=CARTESIAN_POINT('Ctrl Pts',(7.389696336477,13.8391951107513,4.14888858981181));
#35856=CARTESIAN_POINT('Ctrl Pts',(8.18053946683774,14.0346488726453,3.44401143686367));
#35857=CARTESIAN_POINT('Ctrl Pts',(9.9420194768364,14.3333081335907,1.94757748540837));
#35858=CARTESIAN_POINT('Ctrl Pts',(10.9113717350149,14.4104989873604,1.13915583855168));
#35859=CARTESIAN_POINT('Ctrl Pts',(12.834739732217,14.4628660834126,-0.286629408466326));
#35860=CARTESIAN_POINT('Ctrl Pts',(13.8081428716979,14.422640991687,-0.978270473832918));
#35861=CARTESIAN_POINT('Ctrl Pts',(15.7151185916567,14.3061107665235,-2.15221389622411));
#35862=CARTESIAN_POINT('Ctrl Pts',(16.6852254797785,14.2015789338064,-2.70962741922243));
#35863=CARTESIAN_POINT('Ctrl Pts',(18.5768226767694,14.0076819635675,-3.6260862081278));
#35864=CARTESIAN_POINT('Ctrl Pts',(19.5464729449596,13.8818273075211,-4.05120533415427));
#35865=CARTESIAN_POINT('Ctrl Pts',(20.746340681848,13.7535017581768,-4.4779302692017));
#35866=CARTESIAN_POINT('Ctrl Pts',(21.2156214332096,13.70158105669,-4.63869318435442));
#35867=CARTESIAN_POINT('Ctrl Pts',(22.1537708528637,13.5988388255708,-4.93390876526187));
#35868=CARTESIAN_POINT('Ctrl Pts',(22.8728508922896,13.5262523639446,-5.12767073297796));
#35869=CARTESIAN_POINT('Ctrl Pts',(23.4112391022536,13.4803679794399,-5.2528007404175));
#35870=CARTESIAN_POINT('Ctrl Pts',(23.5274006995052,13.4704404449521,-5.27931561824262));
#35871=CARTESIAN_POINT('Ctrl Pts',(23.7586975975698,13.4509289072633,-5.33062970711065));
#35872=CARTESIAN_POINT('Ctrl Pts',(24.1668938536997,13.4171810922988,-5.41708560365393));
#35873=CARTESIAN_POINT('Ctrl Pts',(24.7548128660956,13.3713845002051,-5.5295630582188));
#35874=CARTESIAN_POINT('Ctrl Pts',(25.3473131502195,13.3310219589391,-5.62567073595879));
#35875=CARTESIAN_POINT('Ctrl Pts',(25.8218041556279,13.3034028562424,-5.69154378511349));
#35876=CARTESIAN_POINT('Ctrl Pts',(26.058958766635,13.2913640661323,-5.72065900880544));
#35877=CARTESIAN_POINT('Ctrl Pts',(26.6316948383759,13.2646759506015,-5.7862349204564));
#35878=CARTESIAN_POINT('Ctrl Pts',(27.5576851463964,13.2364409873879,-5.85186367837985));
#35879=CARTESIAN_POINT('Ctrl Pts',(28.5507795710392,13.221915949884,-5.88219883517416));
#35880=CARTESIAN_POINT('Ctrl Pts',(29.1361849357885,13.2135466774644,-5.90128718803099));
#35881=CARTESIAN_POINT('Ctrl Pts',(29.2912521292175,13.2116327381159,-5.90574282943917));
#35882=CARTESIAN_POINT('Ctrl Pts',(29.6100275770337,13.2086893874641,-5.91253309751283));
#35883=CARTESIAN_POINT('Ctrl Pts',(30.1692894984411,13.205972123429,-5.91881362945882));
#35884=CARTESIAN_POINT('Ctrl Pts',(31.3098805820071,13.2079309635127,-5.91428725204098));
#35885=CARTESIAN_POINT('Ctrl Pts',(32.3163182251691,13.215170536538,-5.8978567744948));
#35886=CARTESIAN_POINT('Ctrl Pts',(33.1686695899411,13.2151857432769,-5.8978379745169));
#35887=CARTESIAN_POINT('Ctrl Pts',(33.4952713010557,13.2151875891279,-5.89783593918777));
#35888=CARTESIAN_POINT('Ctrl Pts',(34.1548283685118,13.2151907586342,-5.89783217350438));
#35889=CARTESIAN_POINT('Ctrl Pts',(34.9764778638341,13.2152010495211,-5.89782019909883));
#35890=CARTESIAN_POINT('Ctrl Pts',(35.9641101124161,13.2152053506642,-5.89781516246842));
#35891=CARTESIAN_POINT('Ctrl Pts',(37.9386244259607,13.2152112104218,-5.89780833274505));
#35892=CARTESIAN_POINT('Ctrl Pts',(39.5833333333333,13.2152418049849,-5.89777260594516));
#35893=CARTESIAN_POINT('Ctrl Pts',(40.9,13.2152418049849,-5.89777260594516));
#35894=CARTESIAN_POINT('Ctrl Pts',(6.84649785567288,21.3772113060719,6.71741536412572));
#35895=CARTESIAN_POINT('Ctrl Pts',(7.61279643984166,21.7222003209083,5.5922435141165));
#35896=CARTESIAN_POINT('Ctrl Pts',(8.41290239278215,21.9819683115275,4.47781399151289));
#35897=CARTESIAN_POINT('Ctrl Pts',(10.1883118359637,22.3516942143149,2.12504829883047));
#35898=CARTESIAN_POINT('Ctrl Pts',(11.1645908932198,22.4195115822635,0.860235293933488));
#35899=CARTESIAN_POINT('Ctrl Pts',(13.104616539894,22.4060524143024,-1.36442582505286));
#35900=CARTESIAN_POINT('Ctrl Pts',(14.0814329274866,22.2982732069865,-2.43568052201622));
#35901=CARTESIAN_POINT('Ctrl Pts',(15.9946796213894,22.0394507048972,-4.24582169215594));
#35902=CARTESIAN_POINT('Ctrl Pts',(16.9653275559584,21.84127820419,-5.10151618176832));
#35903=CARTESIAN_POINT('Ctrl Pts',(18.8448710605556,21.4842569534397,-6.49486940232065));
#35904=CARTESIAN_POINT('Ctrl Pts',(19.8101236302158,21.2634255374821,-7.14150804350573));
#35905=CARTESIAN_POINT('Ctrl Pts',(20.9856903475786,21.0426589820634,-7.78021164720297));
#35906=CARTESIAN_POINT('Ctrl Pts',(21.4500377829478,20.9532273635235,-8.02347291078474));
#35907=CARTESIAN_POINT('Ctrl Pts',(22.3710393802636,20.7788884454095,-8.46623345546776));
#35908=CARTESIAN_POINT('Ctrl Pts',(23.071969318899,20.6575298272076,-8.75491470148115));
#35909=CARTESIAN_POINT('Ctrl Pts',(23.5926347936584,20.5813719818059,-8.94023465873166));
#35910=CARTESIAN_POINT('Ctrl Pts',(23.7065892332642,20.5647099449237,-8.98001571960564));
#35911=CARTESIAN_POINT('Ctrl Pts',(23.9323706520525,20.5321468576873,-9.05664995495943));
#35912=CARTESIAN_POINT('Ctrl Pts',(24.3307466212141,20.4759485784749,-9.18574049076623));
#35913=CARTESIAN_POINT('Ctrl Pts',(24.9023508233183,20.4001844372315,-9.35309964749794));
#35914=CARTESIAN_POINT('Ctrl Pts',(25.4757972573109,20.333847241253,-9.49555868076772));
#35915=CARTESIAN_POINT('Ctrl Pts',(25.9330914993693,20.2886464898199,-9.59288697707764));
#35916=CARTESIAN_POINT('Ctrl Pts',(26.160978182331,20.2689918009897,-9.6358170524567));
#35917=CARTESIAN_POINT('Ctrl Pts',(26.7099322414348,20.2254900271806,-9.73235004955929));
#35918=CARTESIAN_POINT('Ctrl Pts',(27.5959509089717,20.1795241403996,-9.82915847887788));
#35919=CARTESIAN_POINT('Ctrl Pts',(28.5797495606368,20.1552722532429,-9.87532060641937));
#35920=CARTESIAN_POINT('Ctrl Pts',(29.1657855350674,20.1412111689924,-9.90441669946586));
#35921=CARTESIAN_POINT('Ctrl Pts',(29.3146731630634,20.1381027603737,-9.91097811975312));
#35922=CARTESIAN_POINT('Ctrl Pts',(29.625730006764,20.1332492263267,-9.92113271524795));
#35923=CARTESIAN_POINT('Ctrl Pts',(30.1719452394074,20.1287785103477,-9.93050366138689));
#35924=CARTESIAN_POINT('Ctrl Pts',(31.297781121968,20.131991612471,-9.92376874726294));
#35925=CARTESIAN_POINT('Ctrl Pts',(32.3069259117669,20.1442225454146,-9.89857089566956));
#35926=CARTESIAN_POINT('Ctrl Pts',(33.1709940314751,20.1442592438602,-9.8985167945155));
#35927=CARTESIAN_POINT('Ctrl Pts',(33.496168048976,20.1442637388651,-9.89851046735385));
#35928=CARTESIAN_POINT('Ctrl Pts',(34.1564024558334,20.1442714128624,-9.89849933968831));
#35929=CARTESIAN_POINT('Ctrl Pts',(34.9773378017947,20.1442963704308,-9.89846345509218));
#35930=CARTESIAN_POINT('Ctrl Pts',(35.965039526566,20.1443067963912,-9.8984484259258));
#35931=CARTESIAN_POINT('Ctrl Pts',(37.9392783163648,20.1443210056783,-9.89842798176079));
#35932=CARTESIAN_POINT('Ctrl Pts',(39.5833333333333,20.1443951831047,-9.89832117405886));
#35933=CARTESIAN_POINT('Ctrl Pts',(40.9,20.1443951831047,-9.89832117405886));
#35934=CARTESIAN_POINT('Ctrl Pts',(6.90857970435318,29.1272609852091,8.71018585725739));
#35935=CARTESIAN_POINT('Ctrl Pts',(7.67983757144493,29.5775536996439,7.16260494418019));
#35936=CARTESIAN_POINT('Ctrl Pts',(8.48457055999566,29.9097225030882,5.63283520142947));
#35937=CARTESIAN_POINT('Ctrl Pts',(10.2689932185249,30.364448769713,2.41146069737716));
#35938=CARTESIAN_POINT('Ctrl Pts',(11.2491988139072,30.4296414097155,0.6836721583184));
#35939=CARTESIAN_POINT('Ctrl Pts',(13.2074449203971,30.3576235761244,-2.36894751212039));
#35940=CARTESIAN_POINT('Ctrl Pts',(14.1878085217557,30.1849659988379,-3.82665309566742));
#35941=CARTESIAN_POINT('Ctrl Pts',(16.1228140255811,29.7814752498472,-6.30658851121943));
#35942=CARTESIAN_POINT('Ctrl Pts',(17.0983171044691,29.4886591763938,-7.46839135173999));
#35943=CARTESIAN_POINT('Ctrl Pts',(18.9977376700381,28.9600828729579,-9.36704911481258));
#35944=CARTESIAN_POINT('Ctrl Pts',(19.9674462816336,28.6415548808292,-10.2409515663327));
#35945=CARTESIAN_POINT('Ctrl Pts',(21.1471060032308,28.3239820751164,-11.1004135437215));
#35946=CARTESIAN_POINT('Ctrl Pts',(21.6116736136673,28.1962714220822,-11.4272945418466));
#35947=CARTESIAN_POINT('Ctrl Pts',(22.5321107331753,27.9485409607958,-12.020283834991));
#35948=CARTESIAN_POINT('Ctrl Pts',(23.2282372947767,27.7781185470826,-12.4035528917692));
#35949=CARTESIAN_POINT('Ctrl Pts',(23.7411423015334,27.6723004799181,-12.6473785079705));
#35950=CARTESIAN_POINT('Ctrl Pts',(23.854105005908,27.6489722597554,-12.7001926206311));
#35951=CARTESIAN_POINT('Ctrl Pts',(24.0772792343327,27.6035767537808,-12.801532363273));
#35952=CARTESIAN_POINT('Ctrl Pts',(24.4706231308704,27.5254067801745,-12.9720321690744));
#35953=CARTESIAN_POINT('Ctrl Pts',(25.0326506601032,27.4207276483817,-13.1919318242547));
#35954=CARTESIAN_POINT('Ctrl Pts',(25.592916616209,27.3299203180181,-13.3777331675808));
#35955=CARTESIAN_POINT('Ctrl Pts',(26.0369869863338,27.2685418387998,-13.5038445845533));
#35956=CARTESIAN_POINT('Ctrl Pts',(26.2572892845278,27.2420133361895,-13.5592118403735));
#35957=CARTESIAN_POINT('Ctrl Pts',(26.7861809172633,27.1835476308025,-13.6833062419415));
#35958=CARTESIAN_POINT('Ctrl Pts',(27.6340630276976,27.1220525704356,-13.8074117592231));
#35959=CARTESIAN_POINT('Ctrl Pts',(28.6084466264572,27.08811764436,-13.8693290201702));
#35960=CARTESIAN_POINT('Ctrl Pts',(29.1951297895237,27.0683644245334,-13.9084309041029));
#35961=CARTESIAN_POINT('Ctrl Pts',(29.3379067795072,27.0642236253564,-13.9168171018366));
#35962=CARTESIAN_POINT('Ctrl Pts',(29.641285245259,27.0575993546199,-13.930094679983));
#35963=CARTESIAN_POINT('Ctrl Pts',(30.17447907441,27.0515191755615,-13.9423073235084));
#35964=CARTESIAN_POINT('Ctrl Pts',(31.2855677213348,27.0558675796334,-13.9335693345849));
#35965=CARTESIAN_POINT('Ctrl Pts',(32.2974599236721,27.0731946134562,-13.8994232817537));
#35966=CARTESIAN_POINT('Ctrl Pts',(33.1732579076351,27.0732696672435,-13.8993047075201));
#35967=CARTESIAN_POINT('Ctrl Pts',(33.4970065888604,27.0732789151667,-13.8992904506871));
#35968=CARTESIAN_POINT('Ctrl Pts',(34.1579215418455,27.0732946436725,-13.8992658208367));
#35969=CARTESIAN_POINT('Ctrl Pts',(34.9781539333148,27.0733458523266,-13.8991859907804));
#35970=CARTESIAN_POINT('Ctrl Pts',(35.9659297143335,27.0733672375488,-13.8991526077107));
#35971=CARTESIAN_POINT('Ctrl Pts',(37.9398993196361,27.0733963900547,-13.8991071452309));
#35972=CARTESIAN_POINT('Ctrl Pts',(39.5833333333333,27.0735485612246,-13.8988697421725));
#35973=CARTESIAN_POINT('Ctrl Pts',(40.9,27.0735485612246,-13.8988697421725));
#35974=CARTESIAN_POINT('Ctrl Pts',(6.93528330520032,33.5512413216408,9.86563481868489));
#35975=CARTESIAN_POINT('Ctrl Pts',(7.70864561497005,34.0623374960229,8.07765806999139));
#35976=CARTESIAN_POINT('Ctrl Pts',(8.51541871352369,34.4367698578613,6.31093086144101));
#35977=CARTESIAN_POINT('Ctrl Pts',(10.3035747340621,34.941954951338,2.59403255178488));
#35978=CARTESIAN_POINT('Ctrl Pts',(11.2855474597114,35.0067705115655,0.601863607331421));
#35979=CARTESIAN_POINT('Ctrl Pts',(13.2510271399958,34.9032893217431,-2.92382891559037));
#35980=CARTESIAN_POINT('Ctrl Pts',(14.2329608248363,34.6945593989858,-4.60257161238984));
#35981=CARTESIAN_POINT('Ctrl Pts',(16.1768697182174,34.2095752766376,-7.46747574760141));
#35982=CARTESIAN_POINT('Ctrl Pts',(17.1545233971705,33.863251175018,-8.8049937479214));
#35983=CARTESIAN_POINT('Ctrl Pts',(19.0635787323924,33.2359528227276,-10.9976618314205));
#35984=CARTESIAN_POINT('Ctrl Pts',(20.0357940514506,32.8613840028833,-12.0029926013878));
#35985=CARTESIAN_POINT('Ctrl Pts',(21.2200273744509,32.4867165469275,-12.9932317593815));
#35986=CARTESIAN_POINT('Ctrl Pts',(21.6852779128343,32.3368305207215,-13.3687144259958));
#35987=CARTESIAN_POINT('Ctrl Pts',(22.6074094382986,32.0460468583649,-14.0501505350055));
#35988=CARTESIAN_POINT('Ctrl Pts',(23.3034045560158,31.8467199720653,-14.48918193341));
#35989=CARTESIAN_POINT('Ctrl Pts',(23.8143672767889,31.7234333079364,-14.7674149360665));
#35990=CARTESIAN_POINT('Ctrl Pts',(23.9270724954073,31.6962311639843,-14.8277950271987));
#35991=CARTESIAN_POINT('Ctrl Pts',(24.1495225469482,31.6433583861173,-14.9435144746796));
#35992=CARTESIAN_POINT('Ctrl Pts',(24.5413305977735,31.5524212197085,-15.1380475804186));
#35993=CARTESIAN_POINT('Ctrl Pts',(25.0999889357198,31.4310156375915,-15.3882930140601));
#35994=CARTESIAN_POINT('Ctrl Pts',(25.654856885479,31.3262265443362,-15.5988027583031));
#35995=CARTESIAN_POINT('Ctrl Pts',(26.0929602492092,31.2557376661539,-15.7410876933159));
#35996=CARTESIAN_POINT('Ctrl Pts',(26.3096479269531,31.2253935968529,-15.8033473177938));
#35997=CARTESIAN_POINT('Ctrl Pts',(26.8287121638339,31.1587088311851,-15.9425694431083));
#35998=CARTESIAN_POINT('Ctrl Pts',(27.6557884297531,31.0890012981154,-16.0810926132798));
#35999=CARTESIAN_POINT('Ctrl Pts',(28.6247091266678,31.0495586097514,-16.1519656805033));
#36000=CARTESIAN_POINT('Ctrl Pts',(29.2117706203406,31.0265558099778,-16.1967753671694));
#36001=CARTESIAN_POINT('Ctrl Pts',(29.3510921954877,31.0218764373727,-16.2061151113189));
#36002=CARTESIAN_POINT('Ctrl Pts',(29.6501043905813,31.0142857961677,-16.2210980111663));
#36003=CARTESIAN_POINT('Ctrl Pts',(30.1758702019788,31.0073340046884,-16.2348498398372));
#36004=CARTESIAN_POINT('Ctrl Pts',(31.2785352103418,31.0122942956315,-16.2250286703998));
#36005=CARTESIAN_POINT('Ctrl Pts',(32.2920164760144,31.0325718136051,-16.1856975481828));
#36006=CARTESIAN_POINT('Ctrl Pts',(33.174523274163,31.0326760798737,-16.1855272745483));
#36007=CARTESIAN_POINT('Ctrl Pts',(33.4974585875215,31.0326890056742,-16.1855064782319));
#36008=CARTESIAN_POINT('Ctrl Pts',(34.158763915549,31.0327109045833,-16.1854709093049));
#36009=CARTESIAN_POINT('Ctrl Pts',(34.9785998474407,31.0327822824582,-16.1853552918984));
#36010=CARTESIAN_POINT('Ctrl Pts',(35.9664200829455,31.0328120805001,-16.1853069853609));
#36011=CARTESIAN_POINT('Ctrl Pts',(37.9402388284556,31.0328527115371,-16.1852411572709));
#36012=CARTESIAN_POINT('Ctrl Pts',(39.5833333333333,31.033064777293,-16.1848974953804));
#36013=CARTESIAN_POINT('Ctrl Pts',(40.9,31.033064777293,-16.1848974953804));
#36014=CARTESIAN_POINT('Origin',(6.9,15.,-25.9807621135332));
#36015=CARTESIAN_POINT('',(6.9,29.194404870986,-6.90555748864274));
#36016=CARTESIAN_POINT('Ctrl Pts',(6.9,10.8594625780008,-1.92623027574191));
#36017=CARTESIAN_POINT('Ctrl Pts',(6.9,14.5482083700348,-3.008872281479));
#36018=CARTESIAN_POINT('Ctrl Pts',(6.90000000166257,18.4565659967827,-4.07058553003039));
#36019=CARTESIAN_POINT('Ctrl Pts',(6.90000000166257,24.1072623232988,-5.5779781522376));
#36020=CARTESIAN_POINT('Ctrl Pts',(6.9,26.6663167664834,-6.24902093139926));
#36021=CARTESIAN_POINT('Ctrl Pts',(6.9,29.194404870986,-6.90555748864274));
#36022=CARTESIAN_POINT('Origin',(6.9,0.,0.));
#36023=CARTESIAN_POINT('Origin',(40.9,4.49999999999999,-7.79422863405995));
#36024=CARTESIAN_POINT('Ctrl Pts',(40.9,18.5327260452907,-29.0996231131986));
#36025=CARTESIAN_POINT('Ctrl Pts',(40.9,18.2824786427117,-28.6661818974695));
#36026=CARTESIAN_POINT('Ctrl Pts',(40.9,18.0322312401326,-28.2327406817405));
#36027=CARTESIAN_POINT('Ctrl Pts',(40.9,17.7819838375536,-27.7992994660114));
#36028=CARTESIAN_POINT('Ctrl Pts',(30.5,16.1306417505985,-31.061268433756));
#36029=CARTESIAN_POINT('Ctrl Pts',(30.5,16.823692245373,-30.7013555966443));
#36030=CARTESIAN_POINT('Ctrl Pts',(30.5,17.5,-30.3108891324554));
#36031=CARTESIAN_POINT('Ctrl Pts',(30.5,47.8108891324553,-12.8108891324554));
#36032=CARTESIAN_POINT('Ctrl Pts',(30.5,30.3108891324554,17.5));
#36033=CARTESIAN_POINT('Ctrl Pts',(30.5,12.8108891324554,47.8108891324553));
#36034=CARTESIAN_POINT('Ctrl Pts',(30.5,-17.5,30.3108891324554));
#36035=CARTESIAN_POINT('Ctrl Pts',(30.5,-47.8108891324553,12.8108891324554));
#36036=CARTESIAN_POINT('Ctrl Pts',(30.5,-30.3108891324554,-17.5));
#36037=CARTESIAN_POINT('Ctrl Pts',(30.5,-13.5747778926489,-46.4877949884694));
#36038=CARTESIAN_POINT('Ctrl Pts',(30.5,16.1306417505985,-31.061268433756));
#36039=CARTESIAN_POINT('Ctrl Pts',(30.3311478274255,16.0958729911865,-30.9943174850025));
#36040=CARTESIAN_POINT('Ctrl Pts',(30.3311478274255,16.7874296516618,-30.6351804212937));
#36041=CARTESIAN_POINT('Ctrl Pts',(30.3311478274255,17.4622796600955,-30.245555587262));
#36042=CARTESIAN_POINT('Ctrl Pts',(30.3311478274255,47.7078352473574,-12.7832759271665));
#36043=CARTESIAN_POINT('Ctrl Pts',(30.3311478274255,30.245555587262,17.4622796600955));
#36044=CARTESIAN_POINT('Ctrl Pts',(30.3311478274255,12.7832759271665,47.7078352473574));
#36045=CARTESIAN_POINT('Ctrl Pts',(30.3311478274255,-17.4622796600955,30.245555587262));
#36046=CARTESIAN_POINT('Ctrl Pts',(30.3311478274255,-47.7078352473574,12.7832759271665));
#36047=CARTESIAN_POINT('Ctrl Pts',(30.3311478274255,-30.245555587262,-17.4622796600955));
#36048=CARTESIAN_POINT('Ctrl Pts',(30.3311478274255,-13.5455181648638,-46.3875929639907));
#36049=CARTESIAN_POINT('Ctrl Pts',(30.3311478274255,16.0958729911865,-30.9943174850025));
#36050=CARTESIAN_POINT('Ctrl Pts',(29.9897712690917,16.0254447695752,-30.8587004444282));
#36051=CARTESIAN_POINT('Ctrl Pts',(29.9897712690917,16.7139754925467,-30.501134801215));
#36052=CARTESIAN_POINT('Ctrl Pts',(29.9897712690917,17.3858726641896,-30.1132147882992));
#36053=CARTESIAN_POINT('Ctrl Pts',(29.9897712690917,47.4990874524888,-12.7273421241097));
#36054=CARTESIAN_POINT('Ctrl Pts',(29.9897712690917,30.1132147882992,17.3858726641896));
#36055=CARTESIAN_POINT('Ctrl Pts',(29.9897712690917,12.7273421241097,47.4990874524888));
#36056=CARTESIAN_POINT('Ctrl Pts',(29.9897712690917,-17.3858726641896,30.1132147882992));
#36057=CARTESIAN_POINT('Ctrl Pts',(29.9897712690917,-47.4990874524888,12.7273421241097));
#36058=CARTESIAN_POINT('Ctrl Pts',(29.9897712690917,-30.1132147882992,-17.3858726641896));
#36059=CARTESIAN_POINT('Ctrl Pts',(29.9897712690917,-13.4862491363571,-46.1846219490559));
#36060=CARTESIAN_POINT('Ctrl Pts',(29.9897712690917,16.0254447695752,-30.8587004444282));
#36061=CARTESIAN_POINT('Ctrl Pts',(29.4666899049319,15.9171300516369,-30.6501289206644));
#36062=CARTESIAN_POINT('Ctrl Pts',(29.4666899049319,16.6010070497276,-30.2949800354474));
#36063=CARTESIAN_POINT('Ctrl Pts',(29.4666899049319,17.2683629213518,-29.9096819433199));
#36064=CARTESIAN_POINT('Ctrl Pts',(29.4666899049319,47.1780448646716,-12.6413190219681));
#36065=CARTESIAN_POINT('Ctrl Pts',(29.4666899049319,29.9096819433199,17.2683629213518));
#36066=CARTESIAN_POINT('Ctrl Pts',(29.4666899049319,12.6413190219681,47.1780448646716));
#36067=CARTESIAN_POINT('Ctrl Pts',(29.4666899049319,-17.2683629213518,29.9096819433199));
#36068=CARTESIAN_POINT('Ctrl Pts',(29.4666899049319,-47.1780448646716,12.6413190219681));
#36069=CARTESIAN_POINT('Ctrl Pts',(29.4666899049319,-29.9096819433199,-17.2683629213518));
#36070=CARTESIAN_POINT('Ctrl Pts',(29.4666899049319,-13.3950966415431,-45.8724637299593));
#36071=CARTESIAN_POINT('Ctrl Pts',(29.4666899049319,15.9171300516369,-30.6501289206644));
#36072=CARTESIAN_POINT('Ctrl Pts',(28.7471241621752,15.7673462336858,-30.3617042288049));
#36073=CARTESIAN_POINT('Ctrl Pts',(28.7471241621752,16.4447877935127,-30.0098973754615));
#36074=CARTESIAN_POINT('Ctrl Pts',(28.7471241621752,17.105863694435,-29.6282250261092));
#36075=CARTESIAN_POINT('Ctrl Pts',(28.7471241621752,46.7340887205442,-12.5223613316743));
#36076=CARTESIAN_POINT('Ctrl Pts',(28.7471241621752,29.6282250261092,17.105863694435));
#36077=CARTESIAN_POINT('Ctrl Pts',(28.7471241621752,12.5223613316743,46.7340887205442));
#36078=CARTESIAN_POINT('Ctrl Pts',(28.7471241621752,-17.105863694435,29.6282250261092));
#36079=CARTESIAN_POINT('Ctrl Pts',(28.7471241621752,-46.7340887205442,12.5223613316743));
#36080=CARTESIAN_POINT('Ctrl Pts',(28.7471241621752,-29.6282250261092,-17.105863694435));
#36081=CARTESIAN_POINT('Ctrl Pts',(28.7471241621752,-13.2690457322218,-45.4407934015768));
#36082=CARTESIAN_POINT('Ctrl Pts',(28.7471241621752,15.7673462336858,-30.3617042288049));
#36083=CARTESIAN_POINT('Ctrl Pts',(27.8100958442934,15.5715428260696,-29.9846639164451));
#36084=CARTESIAN_POINT('Ctrl Pts',(27.8100958442934,16.2405717231752,-29.6372259010587));
#36085=CARTESIAN_POINT('Ctrl Pts',(27.8100958442934,16.8934381948013,-29.2602932679205));
#36086=CARTESIAN_POINT('Ctrl Pts',(27.8100958442934,46.1537314627218,-12.3668550731192));
#36087=CARTESIAN_POINT('Ctrl Pts',(27.8100958442934,29.2602932679205,16.8934381948013));
#36088=CARTESIAN_POINT('Ctrl Pts',(27.8100958442934,12.3668550731192,46.1537314627218));
#36089=CARTESIAN_POINT('Ctrl Pts',(27.8100958442934,-16.8934381948013,29.2602932679205));
#36090=CARTESIAN_POINT('Ctrl Pts',(27.8100958442934,-46.1537314627218,12.3668550731192));
#36091=CARTESIAN_POINT('Ctrl Pts',(27.8100958442934,-29.2602932679205,-16.8934381948013));
#36092=CARTESIAN_POINT('Ctrl Pts',(27.8100958442934,-13.1042669335782,-44.8764966543029));
#36093=CARTESIAN_POINT('Ctrl Pts',(27.8100958442934,15.5715428260696,-29.9846639164451));
#36094=CARTESIAN_POINT('Ctrl Pts',(26.8343111708818,15.3685420031368,-29.5937642144445));
#36095=CARTESIAN_POINT('Ctrl Pts',(26.8343111708818,16.0288490017,-29.2508556284042));
#36096=CARTESIAN_POINT('Ctrl Pts',(26.8343111708818,16.6732042787395,-28.8788369357517));
#36097=CARTESIAN_POINT('Ctrl Pts',(26.8343111708818,45.5520412144912,-12.2056326570122));
#36098=CARTESIAN_POINT('Ctrl Pts',(26.8343111708818,28.8788369357517,16.6732042787395));
#36099=CARTESIAN_POINT('Ctrl Pts',(26.8343111708818,12.2056326570122,45.5520412144912));
#36100=CARTESIAN_POINT('Ctrl Pts',(26.8343111708818,-16.6732042787395,28.8788369357517));
#36101=CARTESIAN_POINT('Ctrl Pts',(26.8343111708818,-45.5520412144912,12.2056326570122));
#36102=CARTESIAN_POINT('Ctrl Pts',(26.8343111708818,-28.8788369357517,-16.6732042787395));
#36103=CARTESIAN_POINT('Ctrl Pts',(26.8343111708818,-12.9334311338659,-44.2914572749094));
#36104=CARTESIAN_POINT('Ctrl Pts',(26.8343111708818,15.3685420031368,-29.5937642144445));
#36105=CARTESIAN_POINT('Ctrl Pts',(25.8181479469611,15.1612099270725,-29.1945242233064));
#36106=CARTESIAN_POINT('Ctrl Pts',(25.8181479469611,15.8126089354813,-28.8562417071321));
#36107=CARTESIAN_POINT('Ctrl Pts',(25.8181479469611,16.4482714219305,-28.4892417994669));
#36108=CARTESIAN_POINT('Ctrl Pts',(25.8181479469611,44.9375132213974,-12.0409703775364));
#36109=CARTESIAN_POINT('Ctrl Pts',(25.8181479469611,28.4892417994669,16.4482714219305));
#36110=CARTESIAN_POINT('Ctrl Pts',(25.8181479469611,12.0409703775364,44.9375132213974));
#36111=CARTESIAN_POINT('Ctrl Pts',(25.8181479469611,-16.4482714219305,28.4892417994669));
#36112=CARTESIAN_POINT('Ctrl Pts',(25.8181479469611,-44.9375132213974,12.0409703775364));
#36113=CARTESIAN_POINT('Ctrl Pts',(25.8181479469611,-28.4892417994669,-16.4482714219305));
#36114=CARTESIAN_POINT('Ctrl Pts',(25.8181479469611,-12.7589503583264,-43.6939354158518));
#36115=CARTESIAN_POINT('Ctrl Pts',(25.8181479469611,15.1612099270725,-29.1945242233064));
#36116=CARTESIAN_POINT('Ctrl Pts',(24.7595197917227,14.9547233834603,-28.796912394945));
#36117=CARTESIAN_POINT('Ctrl Pts',(24.7595197917227,15.5972507298839,-28.4632370828043));
#36118=CARTESIAN_POINT('Ctrl Pts',(24.7595197917227,16.2242558762948,-28.1012354927406));
#36119=CARTESIAN_POINT('Ctrl Pts',(24.7595197917227,44.3254913690355,-11.8769796164458));
#36120=CARTESIAN_POINT('Ctrl Pts',(24.7595197917227,28.1012354927406,16.2242558762948));
#36121=CARTESIAN_POINT('Ctrl Pts',(24.7595197917227,11.8769796164458,44.3254913690355));
#36122=CARTESIAN_POINT('Ctrl Pts',(24.7595197917227,-16.2242558762948,28.1012354927406));
#36123=CARTESIAN_POINT('Ctrl Pts',(24.7595197917227,-44.3254913690355,11.8769796164458));
#36124=CARTESIAN_POINT('Ctrl Pts',(24.7595197917227,-28.1012354927406,-16.2242558762948));
#36125=CARTESIAN_POINT('Ctrl Pts',(24.7595197917227,-12.5851811425261,-43.0988503438666));
#36126=CARTESIAN_POINT('Ctrl Pts',(24.7595197917227,14.9547233834603,-28.796912394945));
#36127=CARTESIAN_POINT('Ctrl Pts',(23.6563574780851,14.7559082828157,-28.4140727469455));
#36128=CARTESIAN_POINT('Ctrl Pts',(23.6563574780851,15.389893569599,-28.084833470769));
#36129=CARTESIAN_POINT('Ctrl Pts',(23.6563574780851,16.0085630157705,-27.7276444994825));
#36130=CARTESIAN_POINT('Ctrl Pts',(23.6563574780851,43.736207515253,-11.7190814837121));
#36131=CARTESIAN_POINT('Ctrl Pts',(23.6563574780851,27.7276444994825,16.0085630157705));
#36132=CARTESIAN_POINT('Ctrl Pts',(23.6563574780851,11.7190814837121,43.736207515253));
#36133=CARTESIAN_POINT('Ctrl Pts',(23.6563574780851,-16.0085630157705,27.7276444994825));
#36134=CARTESIAN_POINT('Ctrl Pts',(23.6563574780851,-43.736207515253,11.7190814837121));
#36135=CARTESIAN_POINT('Ctrl Pts',(23.6563574780851,-27.7276444994825,-16.0085630157705));
#36136=CARTESIAN_POINT('Ctrl Pts',(23.6563574780851,-12.4178678468319,-42.5258740306932));
#36137=CARTESIAN_POINT('Ctrl Pts',(23.6563574780851,14.7559082828157,-28.4140727469455));
#36138=CARTESIAN_POINT('Ctrl Pts',(22.5073180101405,14.5719314169357,-28.0598057001003));
#36139=CARTESIAN_POINT('Ctrl Pts',(22.5073180101405,15.1980121665098,-27.7346713837132));
#36140=CARTESIAN_POINT('Ctrl Pts',(22.5073180101405,15.8089680335819,-27.3819358493961));
#36141=CARTESIAN_POINT('Ctrl Pts',(22.5073180101405,43.190903882978,-11.5729678158142));
#36142=CARTESIAN_POINT('Ctrl Pts',(22.5073180101405,27.3819358493961,15.8089680335819));
#36143=CARTESIAN_POINT('Ctrl Pts',(22.5073180101405,11.5729678158142,43.190903882978));
#36144=CARTESIAN_POINT('Ctrl Pts',(22.5073180101405,-15.8089680335819,27.3819358493961));
#36145=CARTESIAN_POINT('Ctrl Pts',(22.5073180101405,-43.190903882978,11.5729678158142));
#36146=CARTESIAN_POINT('Ctrl Pts',(22.5073180101405,-27.3819358493961,-15.8089680335819));
#36147=CARTESIAN_POINT('Ctrl Pts',(22.5073180101405,-12.2630417010206,-41.9956608528241));
#36148=CARTESIAN_POINT('Ctrl Pts',(22.5073180101405,14.5719314169357,-28.0598057001003));
#36149=CARTESIAN_POINT('Ctrl Pts',(21.3125219557939,14.4091508971892,-27.7463544749225));
#36150=CARTESIAN_POINT('Ctrl Pts',(21.3125219557939,15.0282378072439,-27.4248521776202));
#36151=CARTESIAN_POINT('Ctrl Pts',(21.3125219557939,15.632368792237,-27.0760569908086));
#36152=CARTESIAN_POINT('Ctrl Pts',(21.3125219557939,42.7084257830456,-11.4436881985716));
#36153=CARTESIAN_POINT('Ctrl Pts',(21.3125219557939,27.0760569908086,15.632368792237));
#36154=CARTESIAN_POINT('Ctrl Pts',(21.3125219557939,11.4436881985716,42.7084257830456));
#36155=CARTESIAN_POINT('Ctrl Pts',(21.3125219557939,-15.632368792237,27.0760569908086));
#36156=CARTESIAN_POINT('Ctrl Pts',(21.3125219557939,-42.7084257830456,11.4436881985716));
#36157=CARTESIAN_POINT('Ctrl Pts',(21.3125219557939,-27.0760569908086,-15.632368792237));
#36158=CARTESIAN_POINT('Ctrl Pts',(21.3125219557939,-12.1260533880339,-41.5265346055806));
#36159=CARTESIAN_POINT('Ctrl Pts',(21.3125219557939,14.4091508971892,-27.7463544749225));
#36160=CARTESIAN_POINT('Ctrl Pts',(20.0742472323676,14.2719922102254,-27.4822408172221));
#36161=CARTESIAN_POINT('Ctrl Pts',(20.0742472323676,14.8851861187905,-27.1637988552073));
#36162=CARTESIAN_POINT('Ctrl Pts',(20.0742472323676,15.4835664656477,-26.8183238008716));
#36163=CARTESIAN_POINT('Ctrl Pts',(20.0742472323676,42.3018902665193,-11.3347573352238));
#36164=CARTESIAN_POINT('Ctrl Pts',(20.0742472323676,26.8183238008716,15.4835664656477));
#36165=CARTESIAN_POINT('Ctrl Pts',(20.0742472323676,11.3347573352238,42.3018902665193));
#36166=CARTESIAN_POINT('Ctrl Pts',(20.0742472323676,-15.4835664656477,26.8183238008716));
#36167=CARTESIAN_POINT('Ctrl Pts',(20.0742472323676,-42.3018902665193,11.3347573352238));
#36168=CARTESIAN_POINT('Ctrl Pts',(20.0742472323676,-26.8183238008716,-15.4835664656477));
#36169=CARTESIAN_POINT('Ctrl Pts',(20.0742472323676,-12.0106271861277,-41.1312493454498));
#36170=CARTESIAN_POINT('Ctrl Pts',(20.0742472323676,14.2719922102254,-27.4822408172221));
#36171=CARTESIAN_POINT('Ctrl Pts',(18.7979917002302,14.1614724492005,-27.2694232481814));
#36172=CARTESIAN_POINT('Ctrl Pts',(18.7979917002302,14.7699178935542,-26.9534472438987));
#36173=CARTESIAN_POINT('Ctrl Pts',(18.7979917002302,15.3636644897785,-26.6106474867382));
#36174=CARTESIAN_POINT('Ctrl Pts',(18.7979917002302,41.9743119765166,-11.2469829969597));
#36175=CARTESIAN_POINT('Ctrl Pts',(18.7979917002302,26.6106474867382,15.3636644897785));
#36176=CARTESIAN_POINT('Ctrl Pts',(18.7979917002302,11.2469829969597,41.9743119765166));
#36177=CARTESIAN_POINT('Ctrl Pts',(18.7979917002302,-15.3636644897785,26.6106474867382));
#36178=CARTESIAN_POINT('Ctrl Pts',(18.7979917002302,-41.9743119765166,11.2469829969597));
#36179=CARTESIAN_POINT('Ctrl Pts',(18.7979917002302,-26.6106474867382,-15.3636644897785));
#36180=CARTESIAN_POINT('Ctrl Pts',(18.7979917002302,-11.9176190323383,-40.8127362898543));
#36181=CARTESIAN_POINT('Ctrl Pts',(18.7979917002302,14.1614724492005,-27.2694232481814));
#36182=CARTESIAN_POINT('Ctrl Pts',(17.4917404060759,14.0757116526894,-27.1042817018803));
#36183=CARTESIAN_POINT('Ctrl Pts',(17.4917404060759,14.6804723978617,-26.7902192241678));
#36184=CARTESIAN_POINT('Ctrl Pts',(17.4917404060759,15.2706233100072,-26.4494954361781));
#36185=CARTESIAN_POINT('Ctrl Pts',(17.4917404060759,41.7201187461852,-11.1788721261709));
#36186=CARTESIAN_POINT('Ctrl Pts',(17.4917404060759,26.4494954361781,15.2706233100072));
#36187=CARTESIAN_POINT('Ctrl Pts',(17.4917404060759,11.1788721261709,41.7201187461852));
#36188=CARTESIAN_POINT('Ctrl Pts',(17.4917404060759,-15.2706233100072,26.4494954361781));
#36189=CARTESIAN_POINT('Ctrl Pts',(17.4917404060759,-41.7201187461852,11.1788721261709));
#36190=CARTESIAN_POINT('Ctrl Pts',(17.4917404060759,-26.4494954361781,-15.2706233100072));
#36191=CARTESIAN_POINT('Ctrl Pts',(17.4917404060759,-11.8454468408945,-40.5655774732432));
#36192=CARTESIAN_POINT('Ctrl Pts',(17.4917404060759,14.0757116526894,-27.1042817018803));
#36193=CARTESIAN_POINT('Ctrl Pts',(16.1647270995715,14.011024902894,-26.9797204766935));
#36194=CARTESIAN_POINT('Ctrl Pts',(16.1647270995715,14.6130063919992,-26.6671013136366));
#36195=CARTESIAN_POINT('Ctrl Pts',(16.1647270995715,15.2004451894511,-26.3279433657953));
#36196=CARTESIAN_POINT('Ctrl Pts',(16.1647270995715,41.5283885552464,-11.1274981763442));
#36197=CARTESIAN_POINT('Ctrl Pts',(16.1647270995715,26.3279433657953,15.2004451894511));
#36198=CARTESIAN_POINT('Ctrl Pts',(16.1647270995715,11.1274981763442,41.5283885552464));
#36199=CARTESIAN_POINT('Ctrl Pts',(16.1647270995715,-15.2004451894511,26.3279433657953));
#36200=CARTESIAN_POINT('Ctrl Pts',(16.1647270995715,-41.5283885552464,11.1274981763442));
#36201=CARTESIAN_POINT('Ctrl Pts',(16.1647270995715,-26.3279433657953,-15.2004451894511));
#36202=CARTESIAN_POINT('Ctrl Pts',(16.1647270995715,-11.7910095609247,-40.3791531257526));
#36203=CARTESIAN_POINT('Ctrl Pts',(16.1647270995715,14.011024902894,-26.9797204766935));
#36204=CARTESIAN_POINT('Ctrl Pts',(14.8263876417415,13.9627843740028,-26.8868282012068));
#36205=CARTESIAN_POINT('Ctrl Pts',(14.8263876417415,14.5626932163446,-26.5752853986496));
#36206=CARTESIAN_POINT('Ctrl Pts',(14.8263876417415,15.1481094381123,-26.2372951854241));
#36207=CARTESIAN_POINT('Ctrl Pts',(14.8263876417415,41.3854046235364,-11.0891857473119));
#36208=CARTESIAN_POINT('Ctrl Pts',(14.8263876417415,26.2372951854241,15.1481094381123));
#36209=CARTESIAN_POINT('Ctrl Pts',(14.8263876417415,11.0891857473119,41.3854046235364));
#36210=CARTESIAN_POINT('Ctrl Pts',(14.8263876417415,-15.1481094381123,26.2372951854241));
#36211=CARTESIAN_POINT('Ctrl Pts',(14.8263876417415,-41.3854046235364,11.0891857473119));
#36212=CARTESIAN_POINT('Ctrl Pts',(14.8263876417415,-26.2372951854241,-15.1481094381123));
#36213=CARTESIAN_POINT('Ctrl Pts',(14.8263876417415,-11.750412635195,-40.2401260583921));
#36214=CARTESIAN_POINT('Ctrl Pts',(14.8263876417415,13.9627843740028,-26.8868282012068));
#36215=CARTESIAN_POINT('Ctrl Pts',(13.4853470903953,13.926278703034,-26.8165326442879));
#36216=CARTESIAN_POINT('Ctrl Pts',(13.4853470903953,14.5246190849439,-26.505804369746));
#36217=CARTESIAN_POINT('Ctrl Pts',(13.4853470903953,15.1085047372062,-26.1686978312363));
#36218=CARTESIAN_POINT('Ctrl Pts',(13.4853470903953,41.2772025684426,-11.0601930940301));
#36219=CARTESIAN_POINT('Ctrl Pts',(13.4853470903953,26.1686978312363,15.1085047372062));
#36220=CARTESIAN_POINT('Ctrl Pts',(13.4853470903953,11.0601930940301,41.2772025684426));
#36221=CARTESIAN_POINT('Ctrl Pts',(13.4853470903953,-15.1085047372062,26.1686978312363));
#36222=CARTESIAN_POINT('Ctrl Pts',(13.4853470903953,-41.2772025684426,11.0601930940301));
#36223=CARTESIAN_POINT('Ctrl Pts',(13.4853470903953,-26.1686978312363,-15.1085047372062));
#36224=CARTESIAN_POINT('Ctrl Pts',(13.4853470903953,-11.7196912055777,-40.1349183317465));
#36225=CARTESIAN_POINT('Ctrl Pts',(13.4853470903953,13.926278703034,-26.8165326442879));
#36226=CARTESIAN_POINT('Ctrl Pts',(12.1482076787549,13.8976780812377,-26.7614591013549));
#36227=CARTESIAN_POINT('Ctrl Pts',(12.1482076787549,14.4947896419144,-26.4513689744511));
#36228=CARTESIAN_POINT('Ctrl Pts',(12.1482076787549,15.0774761588537,-26.1149547570431));
#36229=CARTESIAN_POINT('Ctrl Pts',(12.1482076787549,41.1924309158967,-11.0374785981894));
#36230=CARTESIAN_POINT('Ctrl Pts',(12.1482076787549,26.1149547570431,15.0774761588537));
#36231=CARTESIAN_POINT('Ctrl Pts',(12.1482076787549,11.0374785981894,41.1924309158967));
#36232=CARTESIAN_POINT('Ctrl Pts',(12.1482076787549,-15.0774761588537,26.1149547570431));
#36233=CARTESIAN_POINT('Ctrl Pts',(12.1482076787549,-41.1924309158967,11.0374785981894));
#36234=CARTESIAN_POINT('Ctrl Pts',(12.1482076787549,-26.1149547570431,-15.0774761588537));
#36235=CARTESIAN_POINT('Ctrl Pts',(12.1482076787549,-11.6956222878942,-40.0524926066472));
#36236=CARTESIAN_POINT('Ctrl Pts',(12.1482076787549,13.8976780812377,-26.7614591013549));
#36237=CARTESIAN_POINT('Ctrl Pts',(10.8190675759626,13.8744950717886,-26.716817747915));
#36238=CARTESIAN_POINT('Ctrl Pts',(10.8190675759626,14.4706105780977,-26.4072448888814));
#36239=CARTESIAN_POINT('Ctrl Pts',(10.8190675759626,15.0523251033884,-26.0713918511133));
#36240=CARTESIAN_POINT('Ctrl Pts',(10.8190675759626,41.1237169545017,-11.0190667477248));
#36241=CARTESIAN_POINT('Ctrl Pts',(10.8190675759626,26.0713918511133,15.0523251033884));
#36242=CARTESIAN_POINT('Ctrl Pts',(10.8190675759626,11.0190667477248,41.1237169545017));
#36243=CARTESIAN_POINT('Ctrl Pts',(10.8190675759626,-15.0523251033884,26.0713918511133));
#36244=CARTESIAN_POINT('Ctrl Pts',(10.8190675759626,-41.1237169545017,11.0190667477248));
#36245=CARTESIAN_POINT('Ctrl Pts',(10.8190675759626,-26.0713918511133,-15.0523251033884));
#36246=CARTESIAN_POINT('Ctrl Pts',(10.8190675759626,-11.6761125740824,-39.9856802003493));
#36247=CARTESIAN_POINT('Ctrl Pts',(10.8190675759626,13.8744950717886,-26.716817747915));
#36248=CARTESIAN_POINT('Ctrl Pts',(9.50027713254189,13.8551882149624,-26.6796403391198));
#36249=CARTESIAN_POINT('Ctrl Pts',(9.50027713254189,14.4504742051937,-26.3704982618073));
#36250=CARTESIAN_POINT('Ctrl Pts',(9.50027713254189,15.0313792538877,-26.0351125755702));
#36251=CARTESIAN_POINT('Ctrl Pts',(9.50027713254189,41.0664918294579,-11.0037333216826));
#36252=CARTESIAN_POINT('Ctrl Pts',(9.50027713254189,26.0351125755702,15.0313792538877));
#36253=CARTESIAN_POINT('Ctrl Pts',(9.5002771325419,11.0037333216826,41.0664918294579));
#36254=CARTESIAN_POINT('Ctrl Pts',(9.5002771325419,-15.0313792538877,26.0351125755702));
#36255=CARTESIAN_POINT('Ctrl Pts',(9.5002771325419,-41.0664918294579,11.0037333216826));
#36256=CARTESIAN_POINT('Ctrl Pts',(9.50027713254189,-26.0351125755702,-15.0313792538877));
#36257=CARTESIAN_POINT('Ctrl Pts',(9.50027713254189,-11.6598648452398,-39.9300386942093));
#36258=CARTESIAN_POINT('Ctrl Pts',(9.50027713254189,13.8551882149624,-26.6796403391198));
#36259=CARTESIAN_POINT('Ctrl Pts',(8.45435372222587,13.8422173352291,-26.6546635289318));
#36260=CARTESIAN_POINT('Ctrl Pts',(8.45435372222587,14.4369460336456,-26.3458108626791));
#36261=CARTESIAN_POINT('Ctrl Pts',(8.45435372222587,15.0173072536014,-26.0107391561104));
#36262=CARTESIAN_POINT('Ctrl Pts',(8.45435372222587,41.0280464097118,-10.9934319025089));
#36263=CARTESIAN_POINT('Ctrl Pts',(8.45435372222587,26.0107391561104,15.0173072536014));
#36264=CARTESIAN_POINT('Ctrl Pts',(8.45435372222587,10.9934319025089,41.0280464097118));
#36265=CARTESIAN_POINT('Ctrl Pts',(8.45435372222587,-15.0173072536014,26.0107391561104));
#36266=CARTESIAN_POINT('Ctrl Pts',(8.45435372222587,-41.0280464097118,10.9934319025089));
#36267=CARTESIAN_POINT('Ctrl Pts',(8.45435372222587,-26.0107391561104,-15.0173072536014));
#36268=CARTESIAN_POINT('Ctrl Pts',(8.45435372222587,-11.6489491721889,-39.8926571933874));
#36269=CARTESIAN_POINT('Ctrl Pts',(8.45435372222587,13.8422173352291,-26.6546635289318));
#36270=CARTESIAN_POINT('Ctrl Pts',(7.67514864245731,13.8337516775665,-26.6383620035993));
#36271=CARTESIAN_POINT('Ctrl Pts',(7.67514864245731,14.4281166503283,-26.3296982262275));
#36272=CARTESIAN_POINT('Ctrl Pts',(7.67514864245731,15.0081229315276,-25.9948314436454));
#36273=CARTESIAN_POINT('Ctrl Pts',(7.67514864245731,41.0029543751729,-10.9867085121178));
#36274=CARTESIAN_POINT('Ctrl Pts',(7.67514864245731,25.9948314436454,15.0081229315276));
#36275=CARTESIAN_POINT('Ctrl Pts',(7.67514864245731,10.9867085121178,41.0029543751729));
#36276=CARTESIAN_POINT('Ctrl Pts',(7.67514864245731,-15.0081229315276,25.9948314436454));
#36277=CARTESIAN_POINT('Ctrl Pts',(7.67514864245731,-41.0029543751729,10.9867085121178));
#36278=CARTESIAN_POINT('Ctrl Pts',(7.67514864245731,-25.9948314436454,-15.0081229315276));
#36279=CARTESIAN_POINT('Ctrl Pts',(7.67514864245731,-11.6418248789176,-39.8682595430057));
#36280=CARTESIAN_POINT('Ctrl Pts',(7.67514864245731,13.8337516775665,-26.6383620035993));
#36281=CARTESIAN_POINT('Ctrl Pts',(7.15799654185577,13.8286669632852,-26.6285708447822));
#36282=CARTESIAN_POINT('Ctrl Pts',(7.15799654185577,14.4228134720947,-26.3200205194336));
#36283=CARTESIAN_POINT('Ctrl Pts',(7.15799654185577,15.0026065670022,-25.9852768200144));
#36284=CARTESIAN_POINT('Ctrl Pts',(7.15799654185577,40.9878833870167,-10.9826702530122));
#36285=CARTESIAN_POINT('Ctrl Pts',(7.15799654185577,25.9852768200144,15.0026065670022));
#36286=CARTESIAN_POINT('Ctrl Pts',(7.15799654185577,10.9826702530122,40.9878833870167));
#36287=CARTESIAN_POINT('Ctrl Pts',(7.15799654185577,-15.0026065670022,25.9852768200144));
#36288=CARTESIAN_POINT('Ctrl Pts',(7.15799654185577,-40.9878833870167,10.9826702530122));
#36289=CARTESIAN_POINT('Ctrl Pts',(7.15799654185577,-25.9852768200144,-15.0026065670022));
#36290=CARTESIAN_POINT('Ctrl Pts',(7.15799654185577,-11.637545826163,-39.8536056216838));
#36291=CARTESIAN_POINT('Ctrl Pts',(7.15799654185577,13.8286669632852,-26.6285708447822));
#36292=CARTESIAN_POINT('Ctrl Pts',(6.9,13.8262643576559,-26.6239443717909));
#36293=CARTESIAN_POINT('Ctrl Pts',(6.9,14.4203076388911,-26.3154476542665));
#36294=CARTESIAN_POINT('Ctrl Pts',(6.9,15.,-25.9807621135332));
#36295=CARTESIAN_POINT('Ctrl Pts',(6.9,40.9807621135331,-10.9807621135332));
#36296=CARTESIAN_POINT('Ctrl Pts',(6.9,25.9807621135332,15.));
#36297=CARTESIAN_POINT('Ctrl Pts',(6.9,10.9807621135332,40.9807621135331));
#36298=CARTESIAN_POINT('Ctrl Pts',(6.9,-15.,25.9807621135332));
#36299=CARTESIAN_POINT('Ctrl Pts',(6.9,-40.9807621135331,10.9807621135332));
#36300=CARTESIAN_POINT('Ctrl Pts',(6.9,-25.9807621135332,-15.));
#36301=CARTESIAN_POINT('Ctrl Pts',(6.9,-11.6355239079848,-39.846681418688));
#36302=CARTESIAN_POINT('Ctrl Pts',(6.9,13.8262643576559,-26.6239443717909));
#36303=CARTESIAN_POINT('Ctrl Pts',(6.9,29.194404870986,-6.90555748864274));
#36304=CARTESIAN_POINT('Ctrl Pts',(7.85773098116326,28.7583591297181,-8.83308608050288));
#36305=CARTESIAN_POINT('Ctrl Pts',(8.88781981167334,28.148927360677,-10.6725495024415));
#36306=CARTESIAN_POINT('Ctrl Pts',(10.5914578196776,26.9549567714738,-13.4378975079049));
#36307=CARTESIAN_POINT('Ctrl Pts',(11.2365058953701,26.4627511078989,-14.4268759573926));
#36308=CARTESIAN_POINT('Ctrl Pts',(12.0558885382926,25.8276163596339,-15.5639851987506));
#36309=CARTESIAN_POINT('Ctrl Pts',(12.1875764958397,25.7255677072203,-15.7427052651201));
#36310=CARTESIAN_POINT('Ctrl Pts',(13.194901830313,24.9407551262717,-17.0880993664927));
#36311=CARTESIAN_POINT('Ctrl Pts',(14.2258982134098,24.0748117650461,-18.4224696507577));
#36312=CARTESIAN_POINT('Ctrl Pts',(18.2616480823244,20.9914735836847,-22.4465505568645));
#36313=CARTESIAN_POINT('Ctrl Pts',(21.0496416709525,19.1084188222497,-24.4970863377161));
#36314=CARTESIAN_POINT('Ctrl Pts',(25.8000196361138,18.0798601480504,-27.4404163303281));
#36315=CARTESIAN_POINT('Ctrl Pts',(26.8976561124457,18.1725012311874,-27.9949084025612));
#36316=CARTESIAN_POINT('Ctrl Pts',(28.0045908801237,18.293020318403,-28.5110480063609));
#36317=CARTESIAN_POINT('Ctrl Pts',(28.5235971652406,18.3760345677215,-28.7375730360626));
#36318=CARTESIAN_POINT('Ctrl Pts',(29.0834839543824,18.4629109750536,-28.9821227669885));
#36319=CARTESIAN_POINT('Ctrl Pts',(29.1146288039499,18.4676985487665,-28.995750541561));
#36320=CARTESIAN_POINT('Ctrl Pts',(29.5949306848436,18.5426905181124,-29.2050975774362));
#36321=CARTESIAN_POINT('Ctrl Pts',(30.0492939924726,18.6372599535756,-29.3870260594868));
#36322=CARTESIAN_POINT('Ctrl Pts',(30.5,18.7405179110273,-29.559989655385));
#36323=CARTESIAN_POINT('Ctrl Pts',(6.45331003273164,10.9133179225515,-1.5966967862278));
#36324=CARTESIAN_POINT('Ctrl Pts',(7.20830533428676,10.8283039351861,-2.16272621042871));
#36325=CARTESIAN_POINT('Ctrl Pts',(7.9992896214032,10.7080816105349,-2.70879554626308));
#36326=CARTESIAN_POINT('Ctrl Pts',(9.76164489174097,10.3736775708918,-3.82718122480733));
#36327=CARTESIAN_POINT('Ctrl Pts',(10.7316587814816,10.1362456656108,-4.40082635509405));
#36328=CARTESIAN_POINT('Ctrl Pts',(12.6606926111663,9.65961205419966,-5.38563263712134));
#36329=CARTESIAN_POINT('Ctrl Pts',(13.6374431259541,9.3836045062609,-5.83915384029437));
#36330=CARTESIAN_POINT('Ctrl Pts',(14.8679539417017,9.06165302613705,-6.32358226998234));
#36331=CARTESIAN_POINT('Ctrl Pts',(15.8146186835335,8.80867695163279,-6.68453209751777));
#36332=CARTESIAN_POINT('Ctrl Pts',(16.7768279789011,8.55011854625628,-7.00516941257107));
#36333=CARTESIAN_POINT('Ctrl Pts',(18.4426549461008,8.1453397293125,-7.48808598435162));
#36334=CARTESIAN_POINT('Ctrl Pts',(19.4151948753425,7.90738588441818,-7.72973898022664));
#36335=CARTESIAN_POINT('Ctrl Pts',(20.6328868119181,7.66437297695763,-7.97443640583051));
#36336=CARTESIAN_POINT('Ctrl Pts',(21.1054260060183,7.57098863237654,-8.06465516156995));
#36337=CARTESIAN_POINT('Ctrl Pts',(22.0544239964404,7.3938759247956,-8.2283193842106));
#36338=CARTESIAN_POINT('Ctrl Pts',(22.7836594350108,7.27389266543009,-8.33397294082305));
#36339=CARTESIAN_POINT('Ctrl Pts',(23.5025637456199,7.17270583388441,-8.42426711082584));
#36340=CARTESIAN_POINT('Ctrl Pts',(23.9756232708723,7.10861034193422,-8.47952646912202));
#36341=CARTESIAN_POINT('Ctrl Pts',(24.5702383273706,7.0366668150329,-8.53935462310067));
#36342=CARTESIAN_POINT('Ctrl Pts',(25.0506812637274,6.98463603831044,-8.58189400875826));
#36343=CARTESIAN_POINT('Ctrl Pts',(25.4117237717361,6.94891133994683,-8.61093616318041));
#36344=CARTESIAN_POINT('Ctrl Pts',(25.7132331301504,6.92207219011195,-8.63276690479072));
#36345=CARTESIAN_POINT('Ctrl Pts',(25.9243500189533,6.90499555217197,-8.64675417662519));
#36346=CARTESIAN_POINT('Ctrl Pts',(26.04498253513,6.8957416597317,-8.65437719289208));
#36347=CARTESIAN_POINT('Ctrl Pts',(26.1053107047426,6.89128602190947,-8.65806460962785));
#36348=CARTESIAN_POINT('Ctrl Pts',(26.5982868813553,6.85557010312579,-8.68771831234618));
#36349=CARTESIAN_POINT('Ctrl Pts',(27.5414448539111,6.81230249083073,-8.72222386822166));
#36350=CARTESIAN_POINT('Ctrl Pts',(28.5384718269742,6.79157348079194,-8.73742874004834));
#36351=CARTESIAN_POINT('Ctrl Pts',(29.1235718011008,6.77903979219481,-8.7472765876331));
#36352=CARTESIAN_POINT('Ctrl Pts',(29.2812925824006,6.77610142826279,-8.74962231400043));
#36353=CARTESIAN_POINT('Ctrl Pts',(29.6033746665994,6.77163194910156,-8.75316560056394));
#36354=CARTESIAN_POINT('Ctrl Pts',(30.1682156581424,6.76749797708616,-8.75644680260437));
#36355=CARTESIAN_POINT('Ctrl Pts',(31.3151120085297,6.77048174742384,-8.75407681716332));
#36356=CARTESIAN_POINT('Ctrl Pts',(32.3203490755538,6.7812704666075,-8.74562733267071));
#36357=CARTESIAN_POINT('Ctrl Pts',(33.1676615322705,6.78128357449773,-8.74562186943981));
#36358=CARTESIAN_POINT('Ctrl Pts',(33.4948723279892,6.78128505761789,-8.74562133595163));
#36359=CARTESIAN_POINT('Ctrl Pts',(34.1541357431674,6.78128770533515,-8.74562028433962));
#36360=CARTESIAN_POINT('Ctrl Pts',(34.9760826079902,6.78129612595835,-8.74561702798974));
#36361=CARTESIAN_POINT('Ctrl Pts',(35.963684548769,6.78129958330348,-8.74561567977426));
#36362=CARTESIAN_POINT('Ctrl Pts',(37.9383132355671,6.78130435924946,-8.74561382885196));
#36363=CARTESIAN_POINT('Ctrl Pts',(39.5833333333333,6.7813280023926,-8.74560464293356));
#36364=CARTESIAN_POINT('Ctrl Pts',(40.9,6.7813280023926,-8.74560464293356));
#36365=CARTESIAN_POINT('Ctrl Pts',(6.63336813585096,14.1980521881427,-2.58998912169034));
#36366=CARTESIAN_POINT('Ctrl Pts',(7.389696336477,14.0595388287459,-3.32655463912723));
#36367=CARTESIAN_POINT('Ctrl Pts',(8.18035160561763,13.8764440634215,-4.03465273479122));
#36368=CARTESIAN_POINT('Ctrl Pts',(9.94163143861869,13.3869575789582,-5.47986851886094));
#36369=CARTESIAN_POINT('Ctrl Pts',(10.9109664605568,13.0495988183286,-6.21859686207518));
#36370=CARTESIAN_POINT('Ctrl Pts',(12.8334013836927,12.3824387994051,-7.47915893423736));
#36371=CARTESIAN_POINT('Ctrl Pts',(13.8089179831182,12.0008911509523,-8.05904353786121));
#36372=CARTESIAN_POINT('Ctrl Pts',(15.0306778911272,11.5604290689694,-8.67329495695319));
#36373=CARTESIAN_POINT('Ctrl Pts',(15.9745670647921,11.2141745075894,-9.13243737556313));
#36374=CARTESIAN_POINT('Ctrl Pts',(16.9295440841728,10.8635736365945,-9.53704617981301));
#36375=CARTESIAN_POINT('Ctrl Pts',(18.5792362231984,10.3171018918724,-10.1451076803253));
#36376=CARTESIAN_POINT('Ctrl Pts',(19.5469773926754,9.99640408637909,-10.4493242965116));
#36377=CARTESIAN_POINT('Ctrl Pts',(20.7474295734273,9.67172058444851,-10.7549000186159));
#36378=CARTESIAN_POINT('Ctrl Pts',(21.216779417289,9.54637190554464,-10.8681544802445));
#36379=CARTESIAN_POINT('Ctrl Pts',(22.154984393846,9.30976886072804,-11.0724642143301));
#36380=CARTESIAN_POINT('Ctrl Pts',(22.8744776078262,9.1499657882767,-11.2039970972492));
#36381=CARTESIAN_POINT('Ctrl Pts',(23.5816077902756,9.01558422395398,-11.3162019466946));
#36382=CARTESIAN_POINT('Ctrl Pts',(24.0500749276258,8.93008359351409,-11.3851612528791));
#36383=CARTESIAN_POINT('Ctrl Pts',(24.6365533946119,8.83449183240002,-11.459465225808));
#36384=CARTESIAN_POINT('Ctrl Pts',(25.1102835291681,8.76539275960603,-11.5122699159727));
#36385=CARTESIAN_POINT('Ctrl Pts',(25.4658322439322,8.71801358900114,-11.548268841707));
#36386=CARTESIAN_POINT('Ctrl Pts',(25.7624874136677,8.68244638509912,-11.575318037023));
#36387=CARTESIAN_POINT('Ctrl Pts',(25.9700349923404,8.65983585467406,-11.5926401638755));
#36388=CARTESIAN_POINT('Ctrl Pts',(26.0885791323121,8.64758737376027,-11.6020803597249));
#36389=CARTESIAN_POINT('Ctrl Pts',(26.1478525996396,8.64169115913832,-11.6066467500377));
#36390=CARTESIAN_POINT('Ctrl Pts',(26.6319130667255,8.59444428954191,-11.6433645250352));
#36391=CARTESIAN_POINT('Ctrl Pts',(27.5577774489361,8.53717709311563,-11.686082476889));
#36392=CARTESIAN_POINT('Ctrl Pts',(28.5508423746852,8.50942828058708,-11.705090826));
#36393=CARTESIAN_POINT('Ctrl Pts',(29.1362159539418,8.49263545125878,-11.7174369518244));
#36394=CARTESIAN_POINT('Ctrl Pts',(29.2912819508837,8.48875007883402,-11.7203386713974));
#36395=CARTESIAN_POINT('Ctrl Pts',(29.6100529981865,8.48280581727715,-11.7247475094469));
#36396=CARTESIAN_POINT('Ctrl Pts',(30.1693026775043,8.47731190452081,-11.7288279027908));
#36397=CARTESIAN_POINT('Ctrl Pts',(31.3098786008459,8.48127083805319,-11.7258872894479));
#36398=CARTESIAN_POINT('Ctrl Pts',(32.316282704888,8.49575357359979,-11.7152777874897));
#36399=CARTESIAN_POINT('Ctrl Pts',(33.1686195735694,8.49577523975594,-11.7152690782769));
#36400=CARTESIAN_POINT('Ctrl Pts',(33.4952188807556,8.49577770055105,-11.7152682401722));
#36401=CARTESIAN_POINT('Ctrl Pts',(34.154773424404,8.49578208271189,-11.7152665713231));
#36402=CARTESIAN_POINT('Ctrl Pts',(34.9764178792929,8.49579602915739,-11.7152614171756));
#36403=CARTESIAN_POINT('Ctrl Pts',(35.964052055092,8.4958017540615,-11.7152592814564));
#36404=CARTESIAN_POINT('Ctrl Pts',(37.9385651163986,8.49580966365995,-11.7152563511876));
#36405=CARTESIAN_POINT('Ctrl Pts',(39.5833333333333,8.49584881729846,-11.7152418049849));
#36406=CARTESIAN_POINT('Ctrl Pts',(40.9,8.49584881729846,-11.7152418049849));
#36407=CARTESIAN_POINT('Ctrl Pts',(6.84648239176542,21.8719108775553,-4.87117200494631));
#36408=CARTESIAN_POINT('Ctrl Pts',(7.61278097593421,21.6080942034255,-6.01809391809558));
#36409=CARTESIAN_POINT('Ctrl Pts',(8.41274152921386,21.2759544371052,-7.1129769401534));
#36410=CARTESIAN_POINT('Ctrl Pts',(10.1879716557546,20.4198986989574,-9.33526598964861));
#36411=CARTESIAN_POINT('Ctrl Pts',(11.1642573475929,19.8462357742843,-10.4645258845954));
#36412=CARTESIAN_POINT('Ctrl Pts',(13.1034321172788,18.7228640453273,-12.3837514736036));
#36413=CARTESIAN_POINT('Ctrl Pts',(14.0822646095709,18.0925354910949,-13.259092905625));
#36414=CARTESIAN_POINT('Ctrl Pts',(15.3084001581866,17.369341405527,-14.1807147676624));
#36415=CARTESIAN_POINT('Ctrl Pts',(16.2531227144981,16.8032299545451,-14.8695159890907));
#36416=CARTESIAN_POINT('Ctrl Pts',(17.2084375604976,16.2348330754282,-15.4708786153411));
#36417=CARTESIAN_POINT('Ctrl Pts',(18.8473961588576,15.3570672461536,-16.3684102669436));
#36418=CARTESIAN_POINT('Ctrl Pts',(19.8110405035778,14.8437940564495,-16.8164458459156));
#36419=CARTESIAN_POINT('Ctrl Pts',(20.9872655006156,14.3329359049564,-17.2594998647321));
#36420=CARTESIAN_POINT('Ctrl Pts',(21.451734623773,14.1338378277509,-17.4254488483259));
#36421=CARTESIAN_POINT('Ctrl Pts',(22.372798484146,13.7614448137585,-17.7217491293397));
#36422=CARTESIAN_POINT('Ctrl Pts',(23.0743543377555,13.5118529399619,-17.9111527143531));
#36423=CARTESIAN_POINT('Ctrl Pts',(23.7582742987057,13.3034745440376,-18.0719640430557));
#36424=CARTESIAN_POINT('Ctrl Pts',(24.2174386855888,13.1693266480663,-18.1719103336472));
#36425=CARTESIAN_POINT('Ctrl Pts',(24.787021394358,13.0207037868377,-18.2785218143403));
#36426=CARTESIAN_POINT('Ctrl Pts',(25.2463470121627,12.9133861579979,-18.3542161979467));
#36427=CARTESIAN_POINT('Ctrl Pts',(25.5899787396412,12.8400372670535,-18.4056632423981));
#36428=CARTESIAN_POINT('Ctrl Pts',(25.8759048428216,12.7850917865301,-18.4442660174715));
#36429=CARTESIAN_POINT('Ctrl Pts',(26.0755068065021,12.750236170981,-18.4689567859635));
#36430=CARTESIAN_POINT('Ctrl Pts',(26.1893780149121,12.7313725692324,-18.4824083304406));
#36431=CARTESIAN_POINT('Ctrl Pts',(26.2462863876012,12.722296957459,-18.4889145361413));
#36432=CARTESIAN_POINT('Ctrl Pts',(26.7102722067264,12.6496548741733,-18.5411896593424));
#36433=CARTESIAN_POINT('Ctrl Pts',(27.596090538688,12.5614420302552,-18.6020458648117));
#36434=CARTESIAN_POINT('Ctrl Pts',(28.5798438027281,12.5173520665106,-18.6298999603236));
#36435=CARTESIAN_POINT('Ctrl Pts',(29.1658297917573,12.4906249890437,-18.6480680632811));
#36436=CARTESIAN_POINT('Ctrl Pts',(29.3147155528133,12.4846522276653,-18.6521962493028));
#36437=CARTESIAN_POINT('Ctrl Pts',(29.6257654938386,12.4753713397179,-18.658563739707));
#36438=CARTESIAN_POINT('Ctrl Pts',(30.1719616098273,12.4668129248997,-18.6644443298451));
#36439=CARTESIAN_POINT('Ctrl Pts',(31.297773841033,12.4729611884878,-18.6602190141084));
#36440=CARTESIAN_POINT('Ctrl Pts',(32.3068669150105,12.4961463862895,-18.6445149503824));
#36441=CARTESIAN_POINT('Ctrl Pts',(33.170912704073,12.4962026881971,-18.6444874715364));
#36442=CARTESIAN_POINT('Ctrl Pts',(33.4960830255431,12.4962093123003,-18.6444844180378));
#36443=CARTESIAN_POINT('Ctrl Pts',(34.156313582216,12.4962208405722,-18.6444789016082));
#36444=CARTESIAN_POINT('Ctrl Pts',(34.9772414248896,12.4962577684094,-18.6444614154563));
#36445=CARTESIAN_POINT('Ctrl Pts',(35.9649463721128,12.4962728966389,-18.6444542286037));
#36446=CARTESIAN_POINT('Ctrl Pts',(37.9391834323221,12.4962938290756,-18.6444443083028));
#36447=CARTESIAN_POINT('Ctrl Pts',(39.5833333333333,12.4963973854121,-18.6443951831047));
#36448=CARTESIAN_POINT('Ctrl Pts',(40.9,12.4963973854121,-18.6443951831047));
#36449=CARTESIAN_POINT('Ctrl Pts',(6.90857970435318,29.5800408844791,-7.02038826853571));
#36450=CARTESIAN_POINT('Ctrl Pts',(7.67983757144493,29.1962153577801,-8.5857790108899));
#36451=CARTESIAN_POINT('Ctrl Pts',(8.48446296596919,28.7191114013952,-10.0765485557758));
#36452=CARTESIAN_POINT('Ctrl Pts',(10.2687526859613,27.5023711977385,-13.0935628879538));
#36453=CARTESIAN_POINT('Ctrl Pts',(11.2489627292759,26.6949552438923,-14.6224501564806));
#36454=CARTESIAN_POINT('Ctrl Pts',(13.2065810728343,25.1069038454382,-17.2294066625499));
#36455=CARTESIAN_POINT('Ctrl Pts',(14.1884325798659,24.2271697832518,-18.406995285395));
#36456=CARTESIAN_POINT('Ctrl Pts',(15.4296983589675,23.2080338536348,-19.6550892131211));
#36457=CARTESIAN_POINT('Ctrl Pts',(16.3788042670986,22.4189011948388,-20.5796860932724));
#36458=CARTESIAN_POINT('Ctrl Pts',(17.3450159165717,21.621722459271,-21.3903231452906));
#36459=CARTESIAN_POINT('Ctrl Pts',(18.999996264546,20.3951481814248,-22.5937460627633));
#36460=CARTESIAN_POINT('Ctrl Pts',(19.9686658165162,19.6835411202357,-23.1898054127386));
#36461=CARTESIAN_POINT('Ctrl Pts',(21.1489437168837,18.9783964629484,-23.7756910485746));
#36462=CARTESIAN_POINT('Ctrl Pts',(21.6136662410163,18.7043064424583,-23.9949385633149));
#36463=CARTESIAN_POINT('Ctrl Pts',(22.5341605437878,18.1932305660764,-24.384652173758));
#36464=CARTESIAN_POINT('Ctrl Pts',(23.2310352415758,17.8537326154784,-24.6315178872705));
#36465=CARTESIAN_POINT('Ctrl Pts',(23.9047680627604,17.5731511638348,-24.8394315921362));
#36466=CARTESIAN_POINT('Ctrl Pts',(24.3593217251587,17.3912549800687,-24.9695871891295));
#36467=CARTESIAN_POINT('Ctrl Pts',(24.9191284505002,17.1917285847403,-25.1069751863352));
#36468=CARTESIAN_POINT('Ctrl Pts',(25.3687829483019,17.0482631873588,-25.2041659752928));
#36469=CARTESIAN_POINT('Ctrl Pts',(25.7038809466233,16.9507036504238,-25.2699171894914));
#36470=CARTESIAN_POINT('Ctrl Pts',(25.9815275275372,16.8779731233099,-25.3190677310916));
#36471=CARTESIAN_POINT('Ctrl Pts',(26.17472557473,16.8320233777005,-25.350412411697));
#36472=CARTESIAN_POINT('Ctrl Pts',(26.2847430019933,16.8072090098448,-25.3674660195519));
#36473=CARTESIAN_POINT('Ctrl Pts',(26.3396756125245,16.795284989838,-25.3757090167846));
#36474=CARTESIAN_POINT('Ctrl Pts',(26.7867185605541,16.7000344271693,-25.4418392909468));
#36475=CARTESIAN_POINT('Ctrl Pts',(27.6343089133545,16.5847364280859,-25.5185659559037));
#36476=CARTESIAN_POINT('Ctrl Pts',(28.6086204191326,16.524382058732,-25.555224257615));
#36477=CARTESIAN_POINT('Ctrl Pts',(29.1952293795944,16.4877244301022,-25.5792110357042));
#36478=CARTESIAN_POINT('Ctrl Pts',(29.3380035933314,16.4799452423706,-25.5844033272726));
#36479=CARTESIAN_POINT('Ctrl Pts',(29.6413717635317,16.467569571443,-25.5925899885787));
#36480=CARTESIAN_POINT('Ctrl Pts',(30.1745368065166,16.456196787226,-25.6001268754991));
#36481=CARTESIAN_POINT('Ctrl Pts',(31.2855894033319,16.4643300419838,-25.594734665506));
#36482=CARTESIAN_POINT('Ctrl Pts',(32.2974015084452,16.4964013295027,-25.5738307704498));
#36483=CARTESIAN_POINT('Ctrl Pts',(33.173165111218,16.4965224425525,-25.5737672879572));
#36484=CARTESIAN_POINT('Ctrl Pts',(33.4969081472869,16.4965369996127,-25.5737598716198));
#36485=CARTESIAN_POINT('Ctrl Pts',(34.1578169391037,16.4965619872357,-25.5737469053192));
#36486=CARTESIAN_POINT('Ctrl Pts',(34.9780359591177,16.4966423446109,-25.5737054251285));
#36487=CARTESIAN_POINT('Ctrl Pts',(35.9658147840132,16.4966752246751,-25.5736884251094));
#36488=CARTESIAN_POINT('Ctrl Pts',(37.939780228271,16.4967207607425,-25.5736649097448));
#36489=CARTESIAN_POINT('Ctrl Pts',(39.5833333333333,16.4969459535258,-25.5735485612246));
#36490=CARTESIAN_POINT('Ctrl Pts',(40.9,16.4969459535258,-25.5735485612246));
#36491=CARTESIAN_POINT('Ctrl Pts',(6.93528330520032,33.9890447223856,-8.23173028337902));
#36492=CARTESIAN_POINT('Ctrl Pts',(7.70864561497005,33.5376786188307,-10.0357116563145));
#36493=CARTESIAN_POINT('Ctrl Pts',(8.51532719250786,32.9786927413523,-11.7528338486872));
#36494=CARTESIAN_POINT('Ctrl Pts',(10.3033707684643,31.5578840442132,-15.2242195800702));
#36495=CARTESIAN_POINT('Ctrl Pts',(11.285359425586,30.6179424293771,-16.9818886494149));
#36496=CARTESIAN_POINT('Ctrl Pts',(13.2503075123955,28.7660858779662,-19.9828238609275));
#36497=CARTESIAN_POINT('Ctrl Pts',(14.2335802328307,27.7445903826109,-21.333808720003));
#36498=CARTESIAN_POINT('Ctrl Pts',(15.4809874764708,26.5562215055806,-22.7701484639683));
#36499=CARTESIAN_POINT('Ctrl Pts',(16.4318967140332,25.6398645222147,-23.8303538982283));
#36500=CARTESIAN_POINT('Ctrl Pts',(17.402786088206,24.711406834453,-24.7620955812503));
#36501=CARTESIAN_POINT('Ctrl Pts',(19.0657008739462,23.2827894621992,-26.143876791427));
#36502=CARTESIAN_POINT('Ctrl Pts',(20.0370987955261,22.4568785783622,-26.8257745442824));
#36503=CARTESIAN_POINT('Ctrl Pts',(21.2219373681816,21.6368752952078,-27.4963832022119));
#36504=CARTESIAN_POINT('Ctrl Pts',(21.6873545199144,21.3192655757677,-27.7466423667123));
#36505=CARTESIAN_POINT('Ctrl Pts',(22.6095407883912,20.7266792263563,-28.1914275999314));
#36506=CARTESIAN_POINT('Ctrl Pts',(23.3063195468715,20.3342063552496,-28.4721721598027));
#36507=CARTESIAN_POINT('Ctrl Pts',(23.9774915837894,20.0111563083461,-28.7077527668373));
#36508=CARTESIAN_POINT('Ctrl Pts',(24.4307021142568,19.8016082531837,-28.8553793495029));
#36509=CARTESIAN_POINT('Ctrl Pts',(24.9871188326855,19.5726095610114,-29.0105626137829));
#36510=CARTESIAN_POINT('Ctrl Pts',(25.4329141726807,19.4084486444517,-29.1200357132456));
#36511=CARTESIAN_POINT('Ctrl Pts',(25.764395055469,19.2971155191101,-29.1939083663015));
#36512=CARTESIAN_POINT('Ctrl Pts',(26.0382972138567,19.2143910494167,-29.248971810693));
#36513=CARTESIAN_POINT('Ctrl Pts',(26.2284820979125,19.1622606931663,-29.2840172105118));
#36514=CARTESIAN_POINT('Ctrl Pts',(26.3366494455053,19.134150744928,-29.3030632173385));
#36515=CARTESIAN_POINT('Ctrl Pts',(26.3906225284356,19.120654372709,-29.3122642693055));
#36516=CARTESIAN_POINT('Ctrl Pts',(26.8293654116024,19.0129885834585,-29.3859982106881));
#36517=CARTESIAN_POINT('Ctrl Pts',(27.6560988760138,18.8833816200188,-29.4710985842859));
#36518=CARTESIAN_POINT('Ctrl Pts',(28.6249317030313,18.8137794716611,-29.5127595133991));
#36519=CARTESIAN_POINT('Ctrl Pts',(29.2119052185268,18.7714558506411,-29.5400636810172));
#36520=CARTESIAN_POINT('Ctrl Pts',(29.3512234939535,18.7627335234212,-29.5458124634019));
#36521=CARTESIAN_POINT('Ctrl Pts',(29.6502234545146,18.7486685476096,-29.5549926880428));
#36522=CARTESIAN_POINT('Ctrl Pts',(30.1759548990661,18.7357718416963,-29.5634265890416));
#36523=CARTESIAN_POINT('Ctrl Pts',(31.2785766862297,18.7449771625328,-29.5574021311853));
#36524=CARTESIAN_POINT('Ctrl Pts',(32.2919610610306,18.7821959068191,-29.5334837411521));
#36525=CARTESIAN_POINT('Ctrl Pts',(33.1744263360523,18.7823679845322,-29.5333904072538));
#36526=CARTESIAN_POINT('Ctrl Pts',(33.4973548461806,18.782388929425,-29.5333792377696));
#36527=CARTESIAN_POINT('Ctrl Pts',(34.1586526208333,18.7824245927185,-29.5333600113091));
#36528=CARTESIAN_POINT('Ctrl Pts',(34.9784715438078,18.7825395490481,-29.5332982308029));
#36529=CARTESIAN_POINT('Ctrl Pts',(35.9662945600332,18.7825865524219,-29.5332729456426));
#36530=CARTESIAN_POINT('Ctrl Pts',(37.9401075800397,18.7826516826342,-29.5332379342859));
#36531=CARTESIAN_POINT('Ctrl Pts',(39.5833333333333,18.7829737067336,-29.533064777293));
#36532=CARTESIAN_POINT('Ctrl Pts',(40.9,18.7829737067336,-29.533064777293));
#36533=CARTESIAN_POINT('Origin',(6.9,-5.51091059616309E-15,-30.));
#36534=CARTESIAN_POINT('',(6.9,21.8303175223207,-20.5775906479515));
#36535=CARTESIAN_POINT('Ctrl Pts',(6.9,8.44145532612415,-7.09789564133157));
#36536=CARTESIAN_POINT('Ctrl Pts',(6.9,11.09468188726,-9.87986401752105));
#36537=CARTESIAN_POINT('Ctrl Pts',(6.90000000166257,13.9485622548227,-12.753513475675));
#36538=CARTESIAN_POINT('Ctrl Pts',(6.90000000166257,18.0885125115534,-16.8843019432417));
#36539=CARTESIAN_POINT('Ctrl Pts',(6.9,19.9691972794379,-18.7449692586141));
#36540=CARTESIAN_POINT('Ctrl Pts',(6.9,21.8303175223207,-20.5775906479515));
#36541=CARTESIAN_POINT('Origin',(6.9,0.,0.));
#36542=CARTESIAN_POINT('Origin',(40.9,-1.65327317884893E-15,-9.));
#36543=CARTESIAN_POINT('Ctrl Pts',(40.9,1.5,-34.4673758792282));
#36544=CARTESIAN_POINT('Ctrl Pts',(40.9,1.5,-33.9668810740701));
#36545=CARTESIAN_POINT('Ctrl Pts',(40.9,1.49999999999999,-33.466386268912));
#36546=CARTESIAN_POINT('Ctrl Pts',(40.9,1.5,-32.9658914637539));
#36547=CARTESIAN_POINT('Ctrl Pts',(30.5,-1.56108868151375,-34.9651684126997));
#36548=CARTESIAN_POINT('Ctrl Pts',(30.5,-0.780932928377886,-35.));
#36549=CARTESIAN_POINT('Ctrl Pts',(30.5,-6.4293956955236E-15,-35.));
#36550=CARTESIAN_POINT('Ctrl Pts',(30.5,35.,-35.));
#36551=CARTESIAN_POINT('Ctrl Pts',(30.5,35.,-6.4293956955236E-15));
#36552=CARTESIAN_POINT('Ctrl Pts',(30.5,35.,35.));
#36553=CARTESIAN_POINT('Ctrl Pts',(30.5,6.4293956955236E-15,35.));
#36554=CARTESIAN_POINT('Ctrl Pts',(30.5,-35.,35.));
#36555=CARTESIAN_POINT('Ctrl Pts',(30.5,-35.,6.4293956955236E-15));
#36556=CARTESIAN_POINT('Ctrl Pts',(30.5,-35.,-33.472222479613));
#36557=CARTESIAN_POINT('Ctrl Pts',(30.5,-1.56108868151375,-34.9651684126997));
#36558=CARTESIAN_POINT('Ctrl Pts',(30.3311478274255,-1.55772383604588,-34.8898028105656));
#36559=CARTESIAN_POINT('Ctrl Pts',(30.3311478274255,-0.779249668063541,
-34.924559320191));
#36560=CARTESIAN_POINT('Ctrl Pts',(30.3311478274255,-6.41553746746556E-15,
-34.924559320191));
#36561=CARTESIAN_POINT('Ctrl Pts',(30.3311478274255,34.924559320191,-34.924559320191));
#36562=CARTESIAN_POINT('Ctrl Pts',(30.3311478274255,34.924559320191,-6.41553746746556E-15));
#36563=CARTESIAN_POINT('Ctrl Pts',(30.3311478274255,34.924559320191,34.924559320191));
#36564=CARTESIAN_POINT('Ctrl Pts',(30.3311478274255,6.41553746746556E-15,
34.924559320191));
#36565=CARTESIAN_POINT('Ctrl Pts',(30.3311478274255,-34.924559320191,34.924559320191));
#36566=CARTESIAN_POINT('Ctrl Pts',(30.3311478274255,-34.924559320191,6.41553746746556E-15));
#36567=CARTESIAN_POINT('Ctrl Pts',(30.3311478274255,-34.924559320191,-33.4000748447964));
#36568=CARTESIAN_POINT('Ctrl Pts',(30.3311478274255,-1.55772383604588,-34.8898028105656));
#36569=CARTESIAN_POINT('Ctrl Pts',(29.9897712690917,-1.55090794481747,-34.7371408974366));
#36570=CARTESIAN_POINT('Ctrl Pts',(29.9897712690917,-0.775840025831463,
-34.7717453283792));
#36571=CARTESIAN_POINT('Ctrl Pts',(29.9897712690917,-6.38746599257497E-15,
-34.7717453283792));
#36572=CARTESIAN_POINT('Ctrl Pts',(29.9897712690917,34.7717453283791,-34.7717453283791));
#36573=CARTESIAN_POINT('Ctrl Pts',(29.9897712690917,34.7717453283792,-6.38746599257497E-15));
#36574=CARTESIAN_POINT('Ctrl Pts',(29.9897712690917,34.7717453283791,34.7717453283791));
#36575=CARTESIAN_POINT('Ctrl Pts',(29.9897712690917,6.38746599257497E-15,
34.7717453283792));
#36576=CARTESIAN_POINT('Ctrl Pts',(29.9897712690917,-34.7717453283791,34.7717453283791));
#36577=CARTESIAN_POINT('Ctrl Pts',(29.9897712690917,-34.7717453283792,6.38746599257497E-15));
#36578=CARTESIAN_POINT('Ctrl Pts',(29.9897712690917,-34.7717453283791,-33.2539313038843));
#36579=CARTESIAN_POINT('Ctrl Pts',(29.9897712690917,-1.55090794481747,-34.7371408974366));
#36580=CARTESIAN_POINT('Ctrl Pts',(29.4666899049319,-1.54042548027395,-34.5023553003819));
#36581=CARTESIAN_POINT('Ctrl Pts',(29.4666899049319,-0.770596184255049,
-34.5367258427036));
#36582=CARTESIAN_POINT('Ctrl Pts',(29.4666899049319,-6.34429361344449E-15,
-34.5367258427036));
#36583=CARTESIAN_POINT('Ctrl Pts',(29.4666899049319,34.5367258427036,-34.5367258427036));
#36584=CARTESIAN_POINT('Ctrl Pts',(29.4666899049319,34.5367258427036,-6.34429361344449E-15));
#36585=CARTESIAN_POINT('Ctrl Pts',(29.4666899049319,34.5367258427036,34.5367258427036));
#36586=CARTESIAN_POINT('Ctrl Pts',(29.4666899049319,6.34429361344449E-15,
34.5367258427036));
#36587=CARTESIAN_POINT('Ctrl Pts',(29.4666899049319,-34.5367258427036,34.5367258427036));
#36588=CARTESIAN_POINT('Ctrl Pts',(29.4666899049319,-34.5367258427036,6.34429361344449E-15));
#36589=CARTESIAN_POINT('Ctrl Pts',(29.4666899049319,-34.5367258427036,-33.0291706035535));
#36590=CARTESIAN_POINT('Ctrl Pts',(29.4666899049319,-1.54042548027395,-34.5023553003819));
#36591=CARTESIAN_POINT('Ctrl Pts',(28.7471241621752,-1.52592972576568,-34.1776802811774));
#36592=CARTESIAN_POINT('Ctrl Pts',(28.7471241621752,-0.763344698704461,
-34.21172738887));
#36593=CARTESIAN_POINT('Ctrl Pts',(28.7471241621752,-6.28459236601221E-15,
-34.21172738887));
#36594=CARTESIAN_POINT('Ctrl Pts',(28.7471241621752,34.2117273888699,-34.2117273888699));
#36595=CARTESIAN_POINT('Ctrl Pts',(28.7471241621752,34.21172738887,-6.28459236601221E-15));
#36596=CARTESIAN_POINT('Ctrl Pts',(28.7471241621752,34.2117273888699,34.2117273888699));
#36597=CARTESIAN_POINT('Ctrl Pts',(28.7471241621752,6.28459236601221E-15,
34.21172738887));
#36598=CARTESIAN_POINT('Ctrl Pts',(28.7471241621752,-34.2117273888699,34.2117273888699));
#36599=CARTESIAN_POINT('Ctrl Pts',(28.7471241621752,-34.21172738887,6.28459236601221E-15));
#36600=CARTESIAN_POINT('Ctrl Pts',(28.7471241621752,-34.2117273888699,-32.718358587775));
#36601=CARTESIAN_POINT('Ctrl Pts',(28.7471241621752,-1.52592972576568,-34.1776802811774));
#36602=CARTESIAN_POINT('Ctrl Pts',(27.8100958442934,-1.50698029472894,-33.7532520886149));
#36603=CARTESIAN_POINT('Ctrl Pts',(27.8100958442934,-0.7538652662764,-33.7868763896026));
#36604=CARTESIAN_POINT('Ctrl Pts',(27.8100958442934,-6.20654850355712E-15,
-33.7868763896026));
#36605=CARTESIAN_POINT('Ctrl Pts',(27.8100958442934,33.7868763896026,-33.7868763896026));
#36606=CARTESIAN_POINT('Ctrl Pts',(27.8100958442934,33.7868763896026,-6.20654850355712E-15));
#36607=CARTESIAN_POINT('Ctrl Pts',(27.8100958442934,33.7868763896026,33.7868763896026));
#36608=CARTESIAN_POINT('Ctrl Pts',(27.8100958442934,6.20654850355712E-15,
33.7868763896026));
#36609=CARTESIAN_POINT('Ctrl Pts',(27.8100958442934,-33.7868763896026,33.7868763896026));
#36610=CARTESIAN_POINT('Ctrl Pts',(27.8100958442934,-33.7868763896026,6.20654850355712E-15));
#36611=CARTESIAN_POINT('Ctrl Pts',(27.8100958442934,-33.7868763896026,-32.3120526686846));
#36612=CARTESIAN_POINT('Ctrl Pts',(27.8100958442934,-1.50698029472894,-33.7532520886149));
#36613=CARTESIAN_POINT('Ctrl Pts',(26.8343111708818,-1.48733431337754,-33.3132226048841));
#36614=CARTESIAN_POINT('Ctrl Pts',(26.8343111708818,-0.744037385305072,
-33.3464085574791));
#36615=CARTESIAN_POINT('Ctrl Pts',(26.8343111708818,-6.1256358754465E-15,
-33.3464085574791));
#36616=CARTESIAN_POINT('Ctrl Pts',(26.8343111708818,33.3464085574791,-33.3464085574791));
#36617=CARTESIAN_POINT('Ctrl Pts',(26.8343111708818,33.3464085574791,-6.1256358754465E-15));
#36618=CARTESIAN_POINT('Ctrl Pts',(26.8343111708818,33.3464085574791,33.3464085574791));
#36619=CARTESIAN_POINT('Ctrl Pts',(26.8343111708818,6.1256358754465E-15,
33.3464085574791));
#36620=CARTESIAN_POINT('Ctrl Pts',(26.8343111708818,-33.3464085574791,33.3464085574791));
#36621=CARTESIAN_POINT('Ctrl Pts',(26.8343111708818,-33.3464085574791,6.1256358754465E-15));
#36622=CARTESIAN_POINT('Ctrl Pts',(26.8343111708818,-33.3464085574791,-31.8908116037717));
#36623=CARTESIAN_POINT('Ctrl Pts',(26.8343111708818,-1.48733431337754,-33.3132226048841));
#36624=CARTESIAN_POINT('Ctrl Pts',(25.8181479469611,-1.46726916269954,-32.8638045923198));
#36625=CARTESIAN_POINT('Ctrl Pts',(25.8181479469611,-0.733999815330429,
-32.8965428438611));
#36626=CARTESIAN_POINT('Ctrl Pts',(25.8181479469611,-6.04299688451223E-15,
-32.8965428438611));
#36627=CARTESIAN_POINT('Ctrl Pts',(25.8181479469611,32.896542843861,-32.896542843861));
#36628=CARTESIAN_POINT('Ctrl Pts',(25.8181479469611,32.8965428438611,-6.04299688451223E-15));
#36629=CARTESIAN_POINT('Ctrl Pts',(25.8181479469611,32.896542843861,32.896542843861));
#36630=CARTESIAN_POINT('Ctrl Pts',(25.8181479469611,6.04299688451223E-15,
32.8965428438611));
#36631=CARTESIAN_POINT('Ctrl Pts',(25.8181479469611,-32.896542843861,32.896542843861));
#36632=CARTESIAN_POINT('Ctrl Pts',(25.8181479469611,-32.8965428438611,6.04299688451223E-15));
#36633=CARTESIAN_POINT('Ctrl Pts',(25.8181479469611,-32.896542843861,-31.4605828822811));
#36634=CARTESIAN_POINT('Ctrl Pts',(25.8181479469611,-1.46726916269954,-32.8638045923198));
#36635=CARTESIAN_POINT('Ctrl Pts',(24.7595197917227,-1.44728584082668,-32.4162193763075));
#36636=CARTESIAN_POINT('Ctrl Pts',(24.7595197917227,-0.724003180127261,
-32.4485117525897));
#36637=CARTESIAN_POINT('Ctrl Pts',(24.7595197917227,-5.96069490823564E-15,
-32.4485117525897));
#36638=CARTESIAN_POINT('Ctrl Pts',(24.7595197917227,32.4485117525897,-32.4485117525897));
#36639=CARTESIAN_POINT('Ctrl Pts',(24.7595197917227,32.4485117525897,-5.96069490823564E-15));
#36640=CARTESIAN_POINT('Ctrl Pts',(24.7595197917227,32.4485117525897,32.4485117525897));
#36641=CARTESIAN_POINT('Ctrl Pts',(24.7595197917227,5.96069490823564E-15,
32.4485117525897));
#36642=CARTESIAN_POINT('Ctrl Pts',(24.7595197917227,-32.4485117525897,32.4485117525897));
#36643=CARTESIAN_POINT('Ctrl Pts',(24.7595197917227,-32.4485117525897,5.96069490823564E-15));
#36644=CARTESIAN_POINT('Ctrl Pts',(24.7595197917227,-32.4485117525897,-31.0321087004291));
#36645=CARTESIAN_POINT('Ctrl Pts',(24.7595197917227,-1.44728584082668,-32.4162193763075));
#36646=CARTESIAN_POINT('Ctrl Pts',(23.6563574780851,-1.42804494464108,-31.9852629652417));
#36647=CARTESIAN_POINT('Ctrl Pts',(23.6563574780851,-0.714377942573004,
-32.017126031541));
#36648=CARTESIAN_POINT('Ctrl Pts',(23.6563574780851,-5.88145063686361E-15,
-32.017126031541));
#36649=CARTESIAN_POINT('Ctrl Pts',(23.6563574780851,32.017126031541,-32.017126031541));
#36650=CARTESIAN_POINT('Ctrl Pts',(23.6563574780851,32.017126031541,-5.88145063686361E-15));
#36651=CARTESIAN_POINT('Ctrl Pts',(23.6563574780851,32.017126031541,32.017126031541));
#36652=CARTESIAN_POINT('Ctrl Pts',(23.6563574780851,5.88145063686361E-15,
32.017126031541));
#36653=CARTESIAN_POINT('Ctrl Pts',(23.6563574780851,-32.017126031541,32.017126031541));
#36654=CARTESIAN_POINT('Ctrl Pts',(23.6563574780851,-32.017126031541,5.88145063686361E-15));
#36655=CARTESIAN_POINT('Ctrl Pts',(23.6563574780851,-32.017126031541,-30.6195533053013));
#36656=CARTESIAN_POINT('Ctrl Pts',(23.6563574780851,-1.42804494464108,-31.9852629652417));
#36657=CARTESIAN_POINT('Ctrl Pts',(22.5073180101405,-1.41024006077928,-31.5864702700101));
#36658=CARTESIAN_POINT('Ctrl Pts',(22.5073180101405,-0.705471068634144,
-31.6179360671638));
#36659=CARTESIAN_POINT('Ctrl Pts',(22.5073180101405,-5.80812063004468E-15,
-31.6179360671638));
#36660=CARTESIAN_POINT('Ctrl Pts',(22.5073180101405,31.6179360671638,-31.6179360671638));
#36661=CARTESIAN_POINT('Ctrl Pts',(22.5073180101405,31.6179360671638,-5.80812063004468E-15));
#36662=CARTESIAN_POINT('Ctrl Pts',(22.5073180101405,31.6179360671638,31.6179360671638));
#36663=CARTESIAN_POINT('Ctrl Pts',(22.5073180101405,5.80812063004468E-15,
31.6179360671638));
#36664=CARTESIAN_POINT('Ctrl Pts',(22.5073180101405,-31.6179360671638,31.6179360671638));
#36665=CARTESIAN_POINT('Ctrl Pts',(22.5073180101405,-31.6179360671638,5.80812063004468E-15));
#36666=CARTESIAN_POINT('Ctrl Pts',(22.5073180101405,-31.6179360671638,-30.237788296751));
#36667=CARTESIAN_POINT('Ctrl Pts',(22.5073180101405,-1.41024006077928,-31.5864702700101));
#36668=CARTESIAN_POINT('Ctrl Pts',(21.3125219557939,-1.394486513532,-31.2336232862855));
#36669=CARTESIAN_POINT('Ctrl Pts',(21.3125219557939,-0.697590373623126,
-31.264737584474));
#36670=CARTESIAN_POINT('Ctrl Pts',(21.3125219557939,-5.7432391213512E-15,
-31.264737584474));
#36671=CARTESIAN_POINT('Ctrl Pts',(21.3125219557939,31.264737584474,-31.264737584474));
#36672=CARTESIAN_POINT('Ctrl Pts',(21.3125219557939,31.264737584474,-5.7432391213512E-15));
#36673=CARTESIAN_POINT('Ctrl Pts',(21.3125219557939,31.264737584474,31.264737584474));
#36674=CARTESIAN_POINT('Ctrl Pts',(21.3125219557939,5.7432391213512E-15,
31.264737584474));
#36675=CARTESIAN_POINT('Ctrl Pts',(21.3125219557939,-31.264737584474,31.264737584474));
#36676=CARTESIAN_POINT('Ctrl Pts',(21.3125219557939,-31.264737584474,5.7432391213512E-15));
#36677=CARTESIAN_POINT('Ctrl Pts',(21.3125219557939,-31.264737584474,-29.9000072055494));
#36678=CARTESIAN_POINT('Ctrl Pts',(21.3125219557939,-1.394486513532,-31.2336232862855));
#36679=CARTESIAN_POINT('Ctrl Pts',(20.0742472323676,-1.38121259194221,-30.9363148057487));
#36680=CARTESIAN_POINT('Ctrl Pts',(20.0742472323676,-0.690950108671538,
-30.9671329312955));
#36681=CARTESIAN_POINT('Ctrl Pts',(20.0742472323676,-5.68857003346224E-15,
-30.9671329312955));
#36682=CARTESIAN_POINT('Ctrl Pts',(20.0742472323676,30.9671329312955,-30.9671329312955));
#36683=CARTESIAN_POINT('Ctrl Pts',(20.0742472323676,30.9671329312955,-5.68857003346224E-15));
#36684=CARTESIAN_POINT('Ctrl Pts',(20.0742472323676,30.9671329312955,30.9671329312955));
#36685=CARTESIAN_POINT('Ctrl Pts',(20.0742472323676,5.68857003346224E-15,
30.9671329312955));
#36686=CARTESIAN_POINT('Ctrl Pts',(20.0742472323676,-30.9671329312955,30.9671329312955));
#36687=CARTESIAN_POINT('Ctrl Pts',(20.0742472323676,-30.9671329312955,5.68857003346224E-15));
#36688=CARTESIAN_POINT('Ctrl Pts',(20.0742472323676,-30.9671329312955,-29.6153932294878));
#36689=CARTESIAN_POINT('Ctrl Pts',(20.0742472323676,-1.38121259194221,-30.9363148057487));
#36690=CARTESIAN_POINT('Ctrl Pts',(18.7979917002302,-1.3705167280896,-30.6967495040754));
#36691=CARTESIAN_POINT('Ctrl Pts',(18.7979917002302,-0.685599514321032,
-30.727328979557));
#36692=CARTESIAN_POINT('Ctrl Pts',(18.7979917002302,-5.64451876217433E-15,
-30.727328979557));
#36693=CARTESIAN_POINT('Ctrl Pts',(18.7979917002302,30.727328979557,-30.727328979557));
#36694=CARTESIAN_POINT('Ctrl Pts',(18.7979917002302,30.727328979557,-5.64451876217433E-15));
#36695=CARTESIAN_POINT('Ctrl Pts',(18.7979917002302,30.727328979557,30.727328979557));
#36696=CARTESIAN_POINT('Ctrl Pts',(18.7979917002302,5.64451876217433E-15,
30.727328979557));
#36697=CARTESIAN_POINT('Ctrl Pts',(18.7979917002302,-30.727328979557,30.727328979557));
#36698=CARTESIAN_POINT('Ctrl Pts',(18.7979917002302,-30.727328979557,5.64451876217433E-15));
#36699=CARTESIAN_POINT('Ctrl Pts',(18.7979917002302,-30.727328979557,-29.3860569087997));
#36700=CARTESIAN_POINT('Ctrl Pts',(18.7979917002302,-1.3705167280896,-30.6967495040754));
#36701=CARTESIAN_POINT('Ctrl Pts',(17.4917404060759,-1.36221698336642,-30.5108523315028));
#36702=CARTESIAN_POINT('Ctrl Pts',(17.4917404060759,-0.681447575979401,
-30.5412466200144));
#36703=CARTESIAN_POINT('Ctrl Pts',(17.4917404060759,-5.61033598727558E-15,
-30.5412466200144));
#36704=CARTESIAN_POINT('Ctrl Pts',(17.4917404060759,30.5412466200144,-30.5412466200144));
#36705=CARTESIAN_POINT('Ctrl Pts',(17.4917404060759,30.5412466200144,-5.61033598727558E-15));
#36706=CARTESIAN_POINT('Ctrl Pts',(17.4917404060759,30.5412466200144,30.5412466200144));
#36707=CARTESIAN_POINT('Ctrl Pts',(17.4917404060759,5.61033598727558E-15,
30.5412466200144));
#36708=CARTESIAN_POINT('Ctrl Pts',(17.4917404060759,-30.5412466200144,30.5412466200144));
#36709=CARTESIAN_POINT('Ctrl Pts',(17.4917404060759,-30.5412466200144,5.61033598727558E-15));
#36710=CARTESIAN_POINT('Ctrl Pts',(17.4917404060759,-30.5412466200144,-29.2080971905671));
#36711=CARTESIAN_POINT('Ctrl Pts',(17.4917404060759,-1.36221698336642,-30.5108523315028));
#36712=CARTESIAN_POINT('Ctrl Pts',(16.1647270995715,-1.35595673938413,-30.3706357712668));
#36713=CARTESIAN_POINT('Ctrl Pts',(16.1647270995715,-0.678315895682607,
-30.4008903789023));
#36714=CARTESIAN_POINT('Ctrl Pts',(16.1647270995715,-5.58455296406284E-15,
-30.4008903789023));
#36715=CARTESIAN_POINT('Ctrl Pts',(16.1647270995715,30.4008903789023,-30.4008903789023));
#36716=CARTESIAN_POINT('Ctrl Pts',(16.1647270995715,30.4008903789023,-5.58455296406284E-15));
#36717=CARTESIAN_POINT('Ctrl Pts',(16.1647270995715,30.4008903789023,30.4008903789023));
#36718=CARTESIAN_POINT('Ctrl Pts',(16.1647270995715,5.58455296406284E-15,
30.4008903789023));
#36719=CARTESIAN_POINT('Ctrl Pts',(16.1647270995715,-30.4008903789023,30.4008903789023));
#36720=CARTESIAN_POINT('Ctrl Pts',(16.1647270995715,-30.4008903789023,5.58455296406284E-15));
#36721=CARTESIAN_POINT('Ctrl Pts',(16.1647270995715,-30.4008903789023,-29.0738676097412));
#36722=CARTESIAN_POINT('Ctrl Pts',(16.1647270995715,-1.35595673938413,-30.3706357712668));
#36723=CARTESIAN_POINT('Ctrl Pts',(14.8263876417415,-1.3512881251525,-30.2660684364343));
#36724=CARTESIAN_POINT('Ctrl Pts',(14.8263876417415,-0.675980426451069,
-30.2962188762245));
#36725=CARTESIAN_POINT('Ctrl Pts',(14.8263876417415,-5.5653251209554E-15,
-30.2962188762246));
#36726=CARTESIAN_POINT('Ctrl Pts',(14.8263876417415,30.2962188762245,-30.2962188762245));
#36727=CARTESIAN_POINT('Ctrl Pts',(14.8263876417415,30.2962188762246,-5.5653251209554E-15));
#36728=CARTESIAN_POINT('Ctrl Pts',(14.8263876417415,30.2962188762245,30.2962188762245));
#36729=CARTESIAN_POINT('Ctrl Pts',(14.8263876417415,5.5653251209554E-15,
30.2962188762246));
#36730=CARTESIAN_POINT('Ctrl Pts',(14.8263876417415,-30.2962188762245,30.2962188762245));
#36731=CARTESIAN_POINT('Ctrl Pts',(14.8263876417415,-30.2962188762246,5.5653251209554E-15));
#36732=CARTESIAN_POINT('Ctrl Pts',(14.8263876417415,-30.2962188762245,-28.9737651004582));
#36733=CARTESIAN_POINT('Ctrl Pts',(14.8263876417415,-1.3512881251525,-30.2660684364343));
#36734=CARTESIAN_POINT('Ctrl Pts',(13.4853470903953,-1.34775518513426,-30.186937862885));
#36735=CARTESIAN_POINT('Ctrl Pts',(13.4853470903953,-0.674213077019295,
-30.2170094744125));
#36736=CARTESIAN_POINT('Ctrl Pts',(13.4853470903953,-5.55077458989668E-15,
-30.2170094744125));
#36737=CARTESIAN_POINT('Ctrl Pts',(13.4853470903953,30.2170094744125,-30.2170094744125));
#36738=CARTESIAN_POINT('Ctrl Pts',(13.4853470903953,30.2170094744125,-5.55077458989668E-15));
#36739=CARTESIAN_POINT('Ctrl Pts',(13.4853470903953,30.2170094744125,30.2170094744125));
#36740=CARTESIAN_POINT('Ctrl Pts',(13.4853470903953,5.55077458989668E-15,
30.2170094744125));
#36741=CARTESIAN_POINT('Ctrl Pts',(13.4853470903953,-30.2170094744125,30.2170094744125));
#36742=CARTESIAN_POINT('Ctrl Pts',(13.4853470903953,-30.2170094744125,5.55077458989668E-15));
#36743=CARTESIAN_POINT('Ctrl Pts',(13.4853470903953,-30.2170094744125,-28.8980132513174));
#36744=CARTESIAN_POINT('Ctrl Pts',(13.4853470903953,-1.34775518513426,-30.186937862885));
#36745=CARTESIAN_POINT('Ctrl Pts',(12.1482076787549,-1.34498727870743,-30.1249424647305));
#36746=CARTESIAN_POINT('Ctrl Pts',(12.1482076787549,-0.672828434816079,
-30.1549523177074));
#36747=CARTESIAN_POINT('Ctrl Pts',(12.1482076787549,-5.53937487514822E-15,
-30.1549523177074));
#36748=CARTESIAN_POINT('Ctrl Pts',(12.1482076787549,30.1549523177074,-30.1549523177074));
#36749=CARTESIAN_POINT('Ctrl Pts',(12.1482076787549,30.1549523177074,-5.53937487514822E-15));
#36750=CARTESIAN_POINT('Ctrl Pts',(12.1482076787549,30.1549523177074,30.1549523177074));
#36751=CARTESIAN_POINT('Ctrl Pts',(12.1482076787549,5.53937487514822E-15,
30.1549523177074));
#36752=CARTESIAN_POINT('Ctrl Pts',(12.1482076787549,-30.1549523177074,30.1549523177074));
#36753=CARTESIAN_POINT('Ctrl Pts',(12.1482076787549,-30.1549523177074,5.53937487514822E-15));
#36754=CARTESIAN_POINT('Ctrl Pts',(12.1482076787549,-30.1549523177074,-28.8386649382978));
#36755=CARTESIAN_POINT('Ctrl Pts',(12.1482076787549,-1.34498727870743,-30.1249424647305));
#36756=CARTESIAN_POINT('Ctrl Pts',(10.8190675759626,-1.34274367710657,-30.0746904138676));
#36757=CARTESIAN_POINT('Ctrl Pts',(10.8190675759626,-0.671706075536292,
-30.1046502067769));
#36758=CARTESIAN_POINT('Ctrl Pts',(10.8190675759626,-5.530134527277E-15,
-30.1046502067769));
#36759=CARTESIAN_POINT('Ctrl Pts',(10.8190675759626,30.1046502067769,-30.1046502067769));
#36760=CARTESIAN_POINT('Ctrl Pts',(10.8190675759626,30.1046502067769,-5.530134527277E-15));
#36761=CARTESIAN_POINT('Ctrl Pts',(10.8190675759626,30.1046502067769,30.1046502067769));
#36762=CARTESIAN_POINT('Ctrl Pts',(10.8190675759626,5.530134527277E-15,
30.1046502067769));
#36763=CARTESIAN_POINT('Ctrl Pts',(10.8190675759626,-30.1046502067769,30.1046502067769));
#36764=CARTESIAN_POINT('Ctrl Pts',(10.8190675759626,-30.1046502067769,5.530134527277E-15));
#36765=CARTESIAN_POINT('Ctrl Pts',(10.8190675759626,-30.1046502067769,-28.7905585540618));
#36766=CARTESIAN_POINT('Ctrl Pts',(10.8190675759626,-1.34274367710657,-30.0746904138676));
#36767=CARTESIAN_POINT('Ctrl Pts',(9.50027713254189,-1.3408752011877,-30.032840404991));
#36768=CARTESIAN_POINT('Ctrl Pts',(9.50027713254189,-0.67077137247412,-30.0627585077754));
#36769=CARTESIAN_POINT('Ctrl Pts',(9.50027713254189,-5.52243914701304E-15,
-30.0627585077754));
#36770=CARTESIAN_POINT('Ctrl Pts',(9.50027713254189,30.0627585077753,-30.0627585077753));
#36771=CARTESIAN_POINT('Ctrl Pts',(9.50027713254189,30.0627585077754,-5.52243914701304E-15));
#36772=CARTESIAN_POINT('Ctrl Pts',(9.5002771325419,30.0627585077753,30.0627585077753));
#36773=CARTESIAN_POINT('Ctrl Pts',(9.5002771325419,5.52243914701304E-15,
30.0627585077754));
#36774=CARTESIAN_POINT('Ctrl Pts',(9.5002771325419,-30.0627585077753,30.0627585077753));
#36775=CARTESIAN_POINT('Ctrl Pts',(9.50027713254189,-30.0627585077754,5.52243914701304E-15));
#36776=CARTESIAN_POINT('Ctrl Pts',(9.50027713254189,-30.0627585077754,-28.750495460661));
#36777=CARTESIAN_POINT('Ctrl Pts',(9.50027713254189,-1.3408752011877,-30.032840404991));
#36778=CARTESIAN_POINT('Ctrl Pts',(8.45435372222587,-1.33961990745209,-30.0047244129961));
#36779=CARTESIAN_POINT('Ctrl Pts',(8.45435372222587,-0.670143413137455,
-30.0346145072029));
#36780=CARTESIAN_POINT('Ctrl Pts',(8.45435372222587,-5.51726917798061E-15,
-30.0346145072029));
#36781=CARTESIAN_POINT('Ctrl Pts',(8.45435372222587,30.0346145072029,-30.0346145072029));
#36782=CARTESIAN_POINT('Ctrl Pts',(8.45435372222587,30.0346145072029,-5.51726917798061E-15));
#36783=CARTESIAN_POINT('Ctrl Pts',(8.45435372222587,30.0346145072029,30.0346145072029));
#36784=CARTESIAN_POINT('Ctrl Pts',(8.45435372222587,5.51726917798061E-15,
30.0346145072029));
#36785=CARTESIAN_POINT('Ctrl Pts',(8.45435372222587,-30.0346145072029,30.0346145072029));
#36786=CARTESIAN_POINT('Ctrl Pts',(8.45435372222587,-30.0346145072029,5.51726917798061E-15));
#36787=CARTESIAN_POINT('Ctrl Pts',(8.45435372222587,-30.0346145072029,-28.7235799678431));
#36788=CARTESIAN_POINT('Ctrl Pts',(8.45435372222587,-1.33961990745209,-30.0047244129961));
#36789=CARTESIAN_POINT('Ctrl Pts',(7.67514864245731,-1.33880061938141,-29.9863740491064));
#36790=CARTESIAN_POINT('Ctrl Pts',(7.67514864245731,-0.66973356516418,-30.0162458630552));
#36791=CARTESIAN_POINT('Ctrl Pts',(7.67514864245731,-5.51389491279158E-15,
-30.0162458630552));
#36792=CARTESIAN_POINT('Ctrl Pts',(7.67514864245731,30.0162458630552,-30.0162458630552));
#36793=CARTESIAN_POINT('Ctrl Pts',(7.67514864245731,30.0162458630552,-5.51389491279158E-15));
#36794=CARTESIAN_POINT('Ctrl Pts',(7.67514864245731,30.0162458630552,30.0162458630552));
#36795=CARTESIAN_POINT('Ctrl Pts',(7.67514864245731,5.51389491279158E-15,
30.0162458630552));
#36796=CARTESIAN_POINT('Ctrl Pts',(7.67514864245731,-30.0162458630552,30.0162458630552));
#36797=CARTESIAN_POINT('Ctrl Pts',(7.67514864245731,-30.0162458630552,5.51389491279158E-15));
#36798=CARTESIAN_POINT('Ctrl Pts',(7.67514864245731,-30.0162458630552,-28.7060131294556));
#36799=CARTESIAN_POINT('Ctrl Pts',(7.67514864245731,-1.33880061938141,-29.9863740491064));
#36800=CARTESIAN_POINT('Ctrl Pts',(7.15799654185577,-1.33830853171149,-29.9753522996976));
#36801=CARTESIAN_POINT('Ctrl Pts',(7.15799654185577,-0.669487398838308,
-30.0052131340045));
#36802=CARTESIAN_POINT('Ctrl Pts',(7.15799654185577,-5.51186823334392E-15,
-30.0052131340045));
#36803=CARTESIAN_POINT('Ctrl Pts',(7.15799654185577,30.0052131340045,-30.0052131340045));
#36804=CARTESIAN_POINT('Ctrl Pts',(7.15799654185577,30.0052131340045,-5.51186823334392E-15));
#36805=CARTESIAN_POINT('Ctrl Pts',(7.15799654185577,30.0052131340045,30.0052131340045));
#36806=CARTESIAN_POINT('Ctrl Pts',(7.15799654185577,5.51186823334392E-15,
30.0052131340045));
#36807=CARTESIAN_POINT('Ctrl Pts',(7.15799654185577,-30.0052131340045,30.0052131340045));
#36808=CARTESIAN_POINT('Ctrl Pts',(7.15799654185577,-30.0052131340045,5.51186823334392E-15));
#36809=CARTESIAN_POINT('Ctrl Pts',(7.15799654185577,-30.0052131340045,-28.695461987703));
#36810=CARTESIAN_POINT('Ctrl Pts',(7.15799654185577,-1.33830853171149,-29.9753522996976));
#36811=CARTESIAN_POINT('Ctrl Pts',(6.9,-1.33807601272607,-29.9701443537426));
#36812=CARTESIAN_POINT('Ctrl Pts',(6.9,-0.669371081466759,-30.));
#36813=CARTESIAN_POINT('Ctrl Pts',(6.9,-5.51091059616309E-15,-30.));
#36814=CARTESIAN_POINT('Ctrl Pts',(6.9,30.,-30.));
#36815=CARTESIAN_POINT('Ctrl Pts',(6.9,30.,-5.51091059616309E-15));
#36816=CARTESIAN_POINT('Ctrl Pts',(6.9,30.,30.));
#36817=CARTESIAN_POINT('Ctrl Pts',(6.9,5.51091059616309E-15,30.));
#36818=CARTESIAN_POINT('Ctrl Pts',(6.9,-30.,30.));
#36819=CARTESIAN_POINT('Ctrl Pts',(6.9,-30.,5.51091059616309E-15));
#36820=CARTESIAN_POINT('Ctrl Pts',(6.9,-30.,-28.6904764110968));
#36821=CARTESIAN_POINT('Ctrl Pts',(6.9,-1.33807601272607,-29.9701443537426));
#36822=CARTESIAN_POINT('Ctrl Pts',(6.9,21.8303175223207,-20.5775906479515));
#36823=CARTESIAN_POINT('Ctrl Pts',(7.85773098116326,20.4889265372405,-22.0288565043892));
#36824=CARTESIAN_POINT('Ctrl Pts',(8.88781981167334,19.0414114324084,-23.3171626725998));
#36825=CARTESIAN_POINT('Ctrl Pts',(10.5914578196776,16.6247285680552,-25.1150390010341));
#36826=CARTESIAN_POINT('Ctrl Pts',(11.2365058953701,15.703976734769,-25.7254166302984));
#36827=CARTESIAN_POINT('Ctrl Pts',(12.0558885382926,14.5853792872662,-26.3926147460599));
#36828=CARTESIAN_POINT('Ctrl Pts',(12.1875764958397,14.4076425286694,-26.4963665374952));
#36829=CARTESIAN_POINT('Ctrl Pts',(13.194901830313,13.0552778456719,-27.2691057169114));
#36830=CARTESIAN_POINT('Ctrl Pts',(14.2258982134098,11.6381637544796,-27.991732600527));
#36831=CARTESIAN_POINT('Ctrl Pts',(18.2616480823244,6.95587410790868,-29.9350198014187));
#36832=CARTESIAN_POINT('Ctrl Pts',(21.0496416709525,4.29983295736293,-30.7693084982877));
#36833=CARTESIAN_POINT('Ctrl Pts',(25.8000196361138,1.93741001991748,-32.8040277065106));
#36834=CARTESIAN_POINT('Ctrl Pts',(26.8976561124457,1.74039351523169,-33.3305524688301));
#36835=CARTESIAN_POINT('Ctrl Pts',(28.0045908801237,1.58669630450145,-33.8378020212277));
#36836=CARTESIAN_POINT('Ctrl Pts',(28.5235971652406,1.54532623843658,-34.0754855762016));
#36837=CARTESIAN_POINT('Ctrl Pts',(29.0834839543824,1.4982885487127,-34.3307100593381));
#36838=CARTESIAN_POINT('Ctrl Pts',(29.1146288039499,1.49562082188433,-34.3449058451715));
#36839=CARTESIAN_POINT('Ctrl Pts',(29.5949306848436,1.45589225448013,-34.5637016811193));
#36840=CARTESIAN_POINT('Ctrl Pts',(30.0492939924726,1.44682754698747,-34.7685410859787));
#36841=CARTESIAN_POINT('Ctrl Pts',(30.5,1.44976976333441,-34.9699609326822));
#36842=CARTESIAN_POINT('Ctrl Pts',(6.45331003273164,8.65286216739172,-6.83943894028999));
#36843=CARTESIAN_POINT('Ctrl Pts',(7.20830533428676,8.29622318255582,-7.28712780725476));
#36844=CARTESIAN_POINT('Ctrl Pts',(7.99924796920645,7.91909532230128,-7.69991572864563));
#36845=CARTESIAN_POINT('Ctrl Pts',(9.76163642871394,7.0702837202071,-8.50127829248443));
#36846=CARTESIAN_POINT('Ctrl Pts',(10.7316626231511,6.57783879792861,-8.8793528128254));
#36847=CARTESIAN_POINT('Ctrl Pts',(12.6608237755523,5.67260683532432,-9.49392179513702));
#36848=CARTESIAN_POINT('Ctrl Pts',(13.6376935580087,5.20677839827646,-9.74868549844379));
#36849=CARTESIAN_POINT('Ctrl Pts',(14.8683081444882,4.68571756497415,-10.0072371758851));
#36850=CARTESIAN_POINT('Ctrl Pts',(15.814981546047,4.28615487511135,-10.1933420307132));
#36851=CARTESIAN_POINT('Ctrl Pts',(16.7774761024725,3.90183726466219,-10.3417484740057));
#36852=CARTESIAN_POINT('Ctrl Pts',(18.4438470226175,3.30966453460613,-10.5575964922699));
#36853=CARTESIAN_POINT('Ctrl Pts',(19.4166260537867,2.98271399009539,-10.6478897990578));
#36854=CARTESIAN_POINT('Ctrl Pts',(20.8624415465507,2.5875063027773,-10.7552000633454));
#36855=CARTESIAN_POINT('Ctrl Pts',(21.8144010701944,2.34040933534244,-10.8125125199159));
#36856=CARTESIAN_POINT('Ctrl Pts',(22.7817704456175,2.13286375196528,-10.8543372932887));
#36857=CARTESIAN_POINT('Ctrl Pts',(23.3296603631195,2.03163991938108,-10.8753724962822));
#36858=CARTESIAN_POINT('Ctrl Pts',(23.4469280425869,2.01025391532517,-10.8796667005723));
#36859=CARTESIAN_POINT('Ctrl Pts',(23.6810288813553,1.96865773783264,-10.8878000542956));
#36860=CARTESIAN_POINT('Ctrl Pts',(24.0941214149603,1.89824222375215,-10.9009272596696));
#36861=CARTESIAN_POINT('Ctrl Pts',(24.6899984645715,1.80575737992304,-10.9167861221079));
#36862=CARTESIAN_POINT('Ctrl Pts',(25.4117472347965,1.71023812556292,-10.9320835607493));
#36863=CARTESIAN_POINT('Ctrl Pts',(25.8944359856997,1.65861072075244,-10.9403877892627));
#36864=CARTESIAN_POINT('Ctrl Pts',(26.3669426319602,1.61476081138877,-10.9478841337461));
#36865=CARTESIAN_POINT('Ctrl Pts',(27.2927605647398,1.54499465236548,-10.9593568588012));
#36866=CARTESIAN_POINT('Ctrl Pts',(28.2852623623168,1.51981821556059,-10.9616475307267));
#36867=CARTESIAN_POINT('Ctrl Pts',(29.2044123671999,1.49506529955051,-10.9652006081482));
#36868=CARTESIAN_POINT('Ctrl Pts',(29.5205491106405,1.48868169066078,-10.9661656603817));
#36869=CARTESIAN_POINT('Ctrl Pts',(30.1691034959588,1.48263221141176,-10.9670510696507));
#36870=CARTESIAN_POINT('Ctrl Pts',(31.3134334344234,1.4864605825931,-10.9664912432219));
#36871=CARTESIAN_POINT('Ctrl Pts',(32.3203424123247,1.49997009105206,-10.9645690748214));
#36872=CARTESIAN_POINT('Ctrl Pts',(33.1675465322482,1.49998069520818,-10.9645713457497));
#36873=CARTESIAN_POINT('Ctrl Pts',(33.4947519346945,1.49998093738942,-10.9645717110255));
#36874=CARTESIAN_POINT('Ctrl Pts',(34.1540738134336,1.49998231763443,-10.9645721532421));
#36875=CARTESIAN_POINT('Ctrl Pts',(34.81145110075,1.499985805429,-10.9645737361772));
#36876=CARTESIAN_POINT('Ctrl Pts',(35.7991041415374,1.49998654292927,-10.9645740230236));
#36877=CARTESIAN_POINT('Ctrl Pts',(37.7734954411133,1.49999064614178,-10.9645758157224));
#36878=CARTESIAN_POINT('Ctrl Pts',(39.5833333333333,1.5,-10.9645797934319));
#36879=CARTESIAN_POINT('Ctrl Pts',(40.9,1.5,-10.9645797934319));
#36880=CARTESIAN_POINT('Ctrl Pts',(6.63336813585096,11.0008793183436,-9.34202246898051));
#36881=CARTESIAN_POINT('Ctrl Pts',(7.389696336477,10.5126404716241,-9.9106502389341));
#36882=CARTESIAN_POINT('Ctrl Pts',(8.18028889045472,10.0000669136624,-10.4323217834721));
#36883=CARTESIAN_POINT('Ctrl Pts',(9.94159575574687,8.85353468669098,-11.439192222287));
#36884=CARTESIAN_POINT('Ctrl Pts',(10.9109419422817,8.192010210379,-11.9102705993651));
#36885=CARTESIAN_POINT('Ctrl Pts',(12.8335218625484,6.98387303125937,-12.6683977976686));
#36886=CARTESIAN_POINT('Ctrl Pts',(13.8091851210584,6.36343771133682,-12.9798296118147));
#36887=CARTESIAN_POINT('Ctrl Pts',(15.0310774900381,5.67481209887734,-13.2915570052697));
#36888=CARTESIAN_POINT('Ctrl Pts',(15.9749773134882,5.14536755152679,-13.5160612446606));
#36889=CARTESIAN_POINT('Ctrl Pts',(16.930312943506,4.63930769376668,-13.6911692618857));
#36890=CARTESIAN_POINT('Ctrl Pts',(18.5806860927912,3.86175938608204,-13.9445588072223));
#36891=CARTESIAN_POINT('Ctrl Pts',(19.548719041905,3.43185831734755,-14.047648520923));
#36892=CARTESIAN_POINT('Ctrl Pts',(20.9744115808253,2.91639691217872,-14.1690991173097));
#36893=CARTESIAN_POINT('Ctrl Pts',(21.9189583606345,2.59280390983887,-14.2328177454448));
#36894=CARTESIAN_POINT('Ctrl Pts',(22.8721113115929,2.32284159836073,-14.2778669302766));
#36895=CARTESIAN_POINT('Ctrl Pts',(23.4111206282029,2.1913240624154,-14.300719458499));
#36896=CARTESIAN_POINT('Ctrl Pts',(23.5272640974129,2.16340494095905,-14.3053783578071));
#36897=CARTESIAN_POINT('Ctrl Pts',(23.7586042074435,2.10919630050476,-14.3141392731538));
#36898=CARTESIAN_POINT('Ctrl Pts',(24.1668594457504,2.01743796447889,-14.3281409258012));
#36899=CARTESIAN_POINT('Ctrl Pts',(24.7549510427126,1.89707890772754,-14.3447231768686));
#36900=CARTESIAN_POINT('Ctrl Pts',(25.4661619742724,1.77296928480105,-14.3604369110458));
#36901=CARTESIAN_POINT('Ctrl Pts',(25.940793652308,1.7060154102986,-14.3689791856741));
#36902=CARTESIAN_POINT('Ctrl Pts',(26.4047985025956,1.64920950338615,-14.3768131131953));
#36903=CARTESIAN_POINT('Ctrl Pts',(27.3109130873601,1.55899536298034,-14.3886741790609));
#36904=CARTESIAN_POINT('Ctrl Pts',(28.2968127703992,1.52586579774316,-14.3906288624532));
#36905=CARTESIAN_POINT('Ctrl Pts',(29.216365869052,1.49337715415662,-14.3942351181099));
#36906=CARTESIAN_POINT('Ctrl Pts',(29.5273677411776,1.48510498656914,-14.3952146919186));
#36907=CARTESIAN_POINT('Ctrl Pts',(30.1704748351474,1.47720108681952,-14.3961140069303));
#36908=CARTESIAN_POINT('Ctrl Pts',(31.3076822233502,1.48219673215098,-14.3955480332033));
#36909=CARTESIAN_POINT('Ctrl Pts',(32.3162781940781,1.49994928257769,-14.3936026936296));
#36910=CARTESIAN_POINT('Ctrl Pts',(33.1684720644413,1.49996698297726,-14.3936066618446));
#36911=CARTESIAN_POINT('Ctrl Pts',(33.4950641584122,1.49996744488463,-14.3936073001223));
#36912=CARTESIAN_POINT('Ctrl Pts',(34.1546952525893,1.49996977575843,-14.3936080728485));
#36913=CARTESIAN_POINT('Ctrl Pts',(34.811773768313,1.49997575137035,-14.3936108388537));
#36914=CARTESIAN_POINT('Ctrl Pts',(35.7994747102212,1.49997700611746,-14.3936113400865));
#36915=CARTESIAN_POINT('Ctrl Pts',(37.7736758948774,1.499984023326,-14.3936144726314));
#36916=CARTESIAN_POINT('Ctrl Pts',(39.5833333333333,1.5,-14.3936214232436));
#36917=CARTESIAN_POINT('Ctrl Pts',(40.9,1.5,-14.3936214232436));
#36918=CARTESIAN_POINT('Ctrl Pts',(6.84643360079894,16.506001665025,-15.1545575883324));
#36919=CARTESIAN_POINT('Ctrl Pts',(7.61273218496772,15.7040687667121,-16.0159127642118));
#36920=CARTESIAN_POINT('Ctrl Pts',(8.4126771054426,14.8690272591124,-16.7980113101253));
#36921=CARTESIAN_POINT('Ctrl Pts',(10.1879439641556,13.0164926384401,-18.2945580567154));
#36922=CARTESIAN_POINT('Ctrl Pts',(11.1642689802371,11.9550510602025,-18.9856854823124));
#36923=CARTESIAN_POINT('Ctrl Pts',(13.1036036726265,10.022452207883,-20.0861315198186));
#36924=CARTESIAN_POINT('Ctrl Pts',(14.0826172183607,9.03879487952599,-20.5290484396468));
#36925=CARTESIAN_POINT('Ctrl Pts',(15.3089235211201,7.95158583831005,-20.9656035967448));
#36926=CARTESIAN_POINT('Ctrl Pts',(16.2536562498252,7.11690983506512,-21.279069264144));
#36927=CARTESIAN_POINT('Ctrl Pts',(17.2094234535123,6.32372298857519,-21.5156901422925));
#36928=CARTESIAN_POINT('Ctrl Pts',(18.8492103514785,5.11428176787038,-21.8541559656567));
#36929=CARTESIAN_POINT('Ctrl Pts',(19.8132789859546,4.44555314736778,-21.9855288021884));
#36930=CARTESIAN_POINT('Ctrl Pts',(21.2105274130183,3.65671370764623,-22.1378650260475));
#36931=CARTESIAN_POINT('Ctrl Pts',(22.1435262947165,3.15760868632205,-22.2155499994866));
#36932=CARTESIAN_POINT('Ctrl Pts',(23.0712019161591,2.74759983583376,-22.2672966100825));
#36933=CARTESIAN_POINT('Ctrl Pts',(23.5926643019347,2.54861011877026,-22.2940508574536));
#36934=CARTESIAN_POINT('Ctrl Pts',(23.7065967589747,2.50584172092975,-22.2995097248263));
#36935=CARTESIAN_POINT('Ctrl Pts',(23.9324349207315,2.42316535684894,-22.3096292230893));
#36936=CARTESIAN_POINT('Ctrl Pts',(24.3308966188196,2.28324508302851,-22.3255066595418));
#36937=CARTESIAN_POINT('Ctrl Pts',(24.9027307486989,2.10031694390082,-22.3435822260678));
#36938=CARTESIAN_POINT('Ctrl Pts',(25.5912058020402,1.91242242103884,-22.3601136597686));
#36939=CARTESIAN_POINT('Ctrl Pts',(26.0479116166522,1.81155274261715,-22.3691489781576));
#36940=CARTESIAN_POINT('Ctrl Pts',(26.4927766852066,1.72621142470537,-22.3777261422415));
#36941=CARTESIAN_POINT('Ctrl Pts',(27.3538144829414,1.59133675559696,-22.3904445374985));
#36942=CARTESIAN_POINT('Ctrl Pts',(28.3239440765631,1.5395372712982,-22.3916143651133));
#36943=CARTESIAN_POINT('Ctrl Pts',(29.2444087331683,1.48903537353033,-22.3953365265065));
#36944=CARTESIAN_POINT('Ctrl Pts',(29.5434413064006,1.4765958448865,-22.3963491807022));
#36945=CARTESIAN_POINT('Ctrl Pts',(30.1738228526165,1.46445321166481,-22.3972793088217));
#36946=CARTESIAN_POINT('Ctrl Pts',(31.2943937060125,1.47211763918551,-22.3966964278384));
#36947=CARTESIAN_POINT('Ctrl Pts',(32.3068807810285,1.49983279134388,-22.394691709999));
#36948=CARTESIAN_POINT('Ctrl Pts',(33.1706991860564,1.49988437406509,-22.3946974029306));
#36949=CARTESIAN_POINT('Ctrl Pts',(33.4958573126069,1.49988713027318,-22.3946983171245));
#36950=CARTESIAN_POINT('Ctrl Pts',(34.1562063695874,1.49989458266054,-22.394699425001));
#36951=CARTESIAN_POINT('Ctrl Pts',(34.8125750960603,1.49991575825724,-22.3947033892012));
#36952=CARTESIAN_POINT('Ctrl Pts',(35.8003855127833,1.49991999484082,-22.3947041076692));
#36953=CARTESIAN_POINT('Ctrl Pts',(37.7741287617181,1.49994455667285,-22.394708597346));
#36954=CARTESIAN_POINT('Ctrl Pts',(39.5833333333333,1.5,-22.394718559471));
#36955=CARTESIAN_POINT('Ctrl Pts',(40.9,1.5,-22.394718559471));
#36956=CARTESIAN_POINT('Ctrl Pts',(6.90857970435319,22.1068727166734,-20.8698550272217));
#36957=CARTESIAN_POINT('Ctrl Pts',(7.67983757144493,20.991774688754,-22.0336104135999));
#36958=CARTESIAN_POINT('Ctrl Pts',(8.48444928201916,19.8332461961107,-23.0860770683301));
#36959=CARTESIAN_POINT('Ctrl Pts',(10.2687663769551,17.2709888357559,-25.0905346149111));
#36960=CARTESIAN_POINT('Ctrl Pts',(11.2490111943913,15.8072894822424,-26.0108786577409));
#36961=CARTESIAN_POINT('Ctrl Pts',(13.2067599054631,13.1283892637642,-27.4745835397));
#36962=CARTESIAN_POINT('Ctrl Pts',(14.1887708824687,11.7775873547894,-28.0545611646472));
#36963=CARTESIAN_POINT('Ctrl Pts',(15.4301927253883,10.2708149751555,-28.6258871350548));
#36964=CARTESIAN_POINT('Ctrl Pts',(16.3793034376203,9.12509880827948,-29.0320485193235));
#36965=CARTESIAN_POINT('Ctrl Pts',(17.3459407209746,8.02905385413649,-29.335531334809));
#36966=CARTESIAN_POINT('Ctrl Pts',(19.0016786397101,6.36442803225958,-29.764530122403));
#36967=CARTESIAN_POINT('Ctrl Pts',(19.9708024570658,5.44984750618438,-29.9249381814107));
#36968=CARTESIAN_POINT('Ctrl Pts',(21.3726541621532,4.37628680649797,-30.1088343166975));
#36969=CARTESIAN_POINT('Ctrl Pts',(22.305997327355,3.69883691082954,-30.2002109026539));
#36970=CARTESIAN_POINT('Ctrl Pts',(23.2278577930096,3.14826448808768,-30.2581794306256));
#36971=CARTESIAN_POINT('Ctrl Pts',(23.7415516356673,2.88362049576681,-30.2885183156943));
#36972=CARTESIAN_POINT('Ctrl Pts',(23.8544946510481,2.82623659223922,-30.2947200062415));
#36973=CARTESIAN_POINT('Ctrl Pts',(24.0777274663499,2.71573667925152,-30.3060802342181));
#36974=CARTESIAN_POINT('Ctrl Pts',(24.4711727956187,2.52895535356898,-30.32363513723));
#36975=CARTESIAN_POINT('Ctrl Pts',(25.0334457271175,2.28601411482693,-30.3429441514165));
#36976=CARTESIAN_POINT('Ctrl Pts',(25.706214488466,2.03835403030808,-30.3600503901637));
#36977=CARTESIAN_POINT('Ctrl Pts',(26.1486936133439,1.90670660027133,-30.3694723684124));
#36978=CARTESIAN_POINT('Ctrl Pts',(26.5774366289031,1.79594947825407,-30.3787139799022));
#36979=CARTESIAN_POINT('Ctrl Pts',(27.3975110717084,1.62272694197858,-30.392198133447));
#36980=CARTESIAN_POINT('Ctrl Pts',(28.3508259392473,1.55227638555954,-30.3926064111246));
#36981=CARTESIAN_POINT('Ctrl Pts',(29.2723062856311,1.48380439950633,-30.3964396342324));
#36982=CARTESIAN_POINT('Ctrl Pts',(29.5594622066961,1.46775103384065,-30.3974855836748));
#36983=CARTESIAN_POINT('Ctrl Pts',(30.1771168569175,1.45157152773897,-30.3984465770314));
#36984=CARTESIAN_POINT('Ctrl Pts',(31.281071177308,1.46177125475314,-30.3978463334884));
#36985=CARTESIAN_POINT('Ctrl Pts',(32.297455993961,1.49958178095818,-30.3957818406259));
#36986=CARTESIAN_POINT('Ctrl Pts',(33.1729044426911,1.49970257782127,-30.395789026338));
#36987=CARTESIAN_POINT('Ctrl Pts',(33.4966295876142,1.4997109685702,-30.3957901777219));
#36988=CARTESIAN_POINT('Ctrl Pts',(34.1576977268014,1.49972932651149,-30.3957915749198));
#36989=CARTESIAN_POINT('Ctrl Pts',(34.813360769929,1.4997840805116,-30.3957965718591));
#36990=CARTESIAN_POINT('Ctrl Pts',(35.8012813983216,1.49979479816102,-30.3957974776821));
#36991=CARTESIAN_POINT('Ctrl Pts',(37.7745713511015,1.49985796376524,-30.395803137258));
#36992=CARTESIAN_POINT('Ctrl Pts',(39.5833333333333,1.49999999999999,-30.3958156956984));
#36993=CARTESIAN_POINT('Ctrl Pts',(40.9,1.49999999999999,-30.3958156956984));
#36994=CARTESIAN_POINT('Ctrl Pts',(6.93528330520032,25.3195110382618,-24.1234099037007));
#36995=CARTESIAN_POINT('Ctrl Pts',(7.70864561497005,24.0266258397084,-25.4600205488393));
#36996=CARTESIAN_POINT('Ctrl Pts',(8.51531156164573,22.6840056101462,-26.6675788409114));
#36997=CARTESIAN_POINT('Ctrl Pts',(10.3033767345502,19.7178334181139,-28.9634999585434));
#36998=CARTESIAN_POINT('Ctrl Pts',(11.2853975328499,18.024966824446,-30.0157138764657));
#36999=CARTESIAN_POINT('Ctrl Pts',(13.2504656206425,14.920608256729,-31.6887121402305));
#37000=CARTESIAN_POINT('Ctrl Pts',(14.2338911783743,13.360326515741,-32.3479754973602));
#37001=CARTESIAN_POINT('Ctrl Pts',(15.4814489736579,11.6128587845954,-32.9977120049688));
#37002=CARTESIAN_POINT('Ctrl Pts',(16.4323633322631,10.2891584164032,-33.457701559807));
#37003=CARTESIAN_POINT('Ctrl Pts',(17.4036580739675,9.01884161707319,-33.8004278805126));
#37004=CARTESIAN_POINT('Ctrl Pts',(19.0672887678302,7.09001985912387,-34.2828730898379));
#37005=CARTESIAN_POINT('Ctrl Pts',(20.0391149919151,6.03348815316116,-34.4604737318843));
#37006=CARTESIAN_POINT('Ctrl Pts',(21.4462778487112,4.79159535501522,-34.6632929668281));
#37007=CARTESIAN_POINT('Ctrl Pts',(22.3811728101678,4.01020122074908,-34.7627792680187));
#37008=CARTESIAN_POINT('Ctrl Pts',(23.3032595484893,3.37635643636738,-34.8244923190156));
#37009=CARTESIAN_POINT('Ctrl Pts',(23.8149974822583,3.07312481135075,-34.8569118346709));
#37010=CARTESIAN_POINT('Ctrl Pts',(23.9276845297173,3.00725282827683,-34.8635414236987));
#37011=CARTESIAN_POINT('Ctrl Pts',(24.1501932465709,2.88055633977638,-34.8756163196445));
#37012=CARTESIAN_POINT('Ctrl Pts',(24.5421106234083,2.66656979475214,-34.8941314993696));
#37013=CARTESIAN_POINT('Ctrl Pts',(25.1010166003946,2.38896069563579,-34.9141289755492));
#37014=CARTESIAN_POINT('Ctrl Pts',(25.7673676623321,2.10719515267299,-34.9315307898229));
#37015=CARTESIAN_POINT('Ctrl Pts',(26.2032614590243,1.95837832513291,-34.9411502230501));
#37016=CARTESIAN_POINT('Ctrl Pts',(26.6241220770206,1.83365744353248,-34.9507523611205));
#37017=CARTESIAN_POINT('Ctrl Pts',(27.4227877709103,1.64008822157604,-34.9646463474546));
#37018=CARTESIAN_POINT('Ctrl Pts',(28.3660425122777,1.55920845841384,-34.9646178111257));
#37019=CARTESIAN_POINT('Ctrl Pts',(29.288154079426,1.48047877405357,-34.9685099768711));
#37020=CARTESIAN_POINT('Ctrl Pts',(29.5685743108623,1.46254110097229,-34.9695745039167));
#37021=CARTESIAN_POINT('Ctrl Pts',(30.1789566228709,1.44412472938078,-34.9705522790041));
#37022=CARTESIAN_POINT('Ctrl Pts',(31.273428633048,1.45573528147978,-34.9699406754865));
#37023=CARTESIAN_POINT('Ctrl Pts',(32.2920480078111,1.49937027232428,-34.9678391394653));
#37024=CARTESIAN_POINT('Ctrl Pts',(33.1741467941405,1.49954725443549,-34.9678459524317));
#37025=CARTESIAN_POINT('Ctrl Pts',(33.4970538821705,1.49956078207587,-34.9678470414555));
#37026=CARTESIAN_POINT('Ctrl Pts',(34.1585338443542,1.49958825610693,-34.9678483649439));
#37027=CARTESIAN_POINT('Ctrl Pts',(34.8137969787743,1.49967176946747,-34.9678530956496));
#37028=CARTESIAN_POINT('Ctrl Pts',(35.8017811867034,1.49968797974803,-34.9678539534013));
#37029=CARTESIAN_POINT('Ctrl Pts',(37.7748158892396,1.49978412416472,-34.9678593117153));
#37030=CARTESIAN_POINT('Ctrl Pts',(39.5833333333333,1.49999999999999,-34.967871202114));
#37031=CARTESIAN_POINT('Ctrl Pts',(40.9,1.49999999999999,-34.967871202114));
#37032=CARTESIAN_POINT('Origin',(6.9,-15.,-25.9807621135332));
#37033=CARTESIAN_POINT('',(6.9,8.61681422303452,-28.7358750109634));
#37034=CARTESIAN_POINT('Ctrl Pts',(6.9,3.76156693666918,-10.3676856018661));
#37035=CARTESIAN_POINT('Ctrl Pts',(6.9,4.66834435251375,-14.103554168739));
#37036=CARTESIAN_POINT('Ctrl Pts',(6.90000000166257,5.70305252110769,-18.0191477848531));
#37037=CARTESIAN_POINT('Ctrl Pts',(6.90000000166257,7.22296038005705,-23.666490663791));
#37038=CARTESIAN_POINT('Ctrl Pts',(6.9,7.92134750786925,-26.2182182108371));
#37039=CARTESIAN_POINT('Ctrl Pts',(6.9,8.61681422303452,-28.7358750109634));
#37040=CARTESIAN_POINT('Origin',(6.9,0.,0.));
#37041=CARTESIAN_POINT('Origin',(40.9,-4.5,-7.79422863405994));
#37042=CARTESIAN_POINT('Ctrl Pts',(40.9,-15.9346498339374,-30.5996231131986));
#37043=CARTESIAN_POINT('Ctrl Pts',(40.9,-15.6844024313584,-30.1661818974695));
#37044=CARTESIAN_POINT('Ctrl Pts',(40.9,-15.4341550287793,-29.7327406817405));
#37045=CARTESIAN_POINT('Ctrl Pts',(40.9,-15.1839076262003,-29.2992994660114));
#37046=CARTESIAN_POINT('Ctrl Pts',(30.5,-18.8345266621011,-29.5001797522422));
#37047=CARTESIAN_POINT('Ctrl Pts',(30.5,-18.176307754627,-29.9204226682664));
#37048=CARTESIAN_POINT('Ctrl Pts',(30.5,-17.5,-30.3108891324553));
#37049=CARTESIAN_POINT('Ctrl Pts',(30.5,12.8108891324553,-47.8108891324553));
#37050=CARTESIAN_POINT('Ctrl Pts',(30.5,30.3108891324553,-17.5));
#37051=CARTESIAN_POINT('Ctrl Pts',(30.5,47.8108891324553,12.8108891324553));
#37052=CARTESIAN_POINT('Ctrl Pts',(30.5,17.5,30.3108891324553));
#37053=CARTESIAN_POINT('Ctrl Pts',(30.5,-12.8108891324553,47.8108891324553));
#37054=CARTESIAN_POINT('Ctrl Pts',(30.5,-30.3108891324553,17.5));
#37055=CARTESIAN_POINT('Ctrl Pts',(30.5,-47.0470003722618,-11.4877949884694));
#37056=CARTESIAN_POINT('Ctrl Pts',(30.5,-18.8345266621011,-29.5001797522422));
#37057=CARTESIAN_POINT('Ctrl Pts',(30.3311478274255,-18.7939298193791,-29.4365936489566));
#37058=CARTESIAN_POINT('Ctrl Pts',(30.3311478274255,-18.1371296685291,-29.8559307532302));
#37059=CARTESIAN_POINT('Ctrl Pts',(30.3311478274255,-17.4622796600955,-30.245555587262));
#37060=CARTESIAN_POINT('Ctrl Pts',(30.3311478274255,12.7832759271664,-47.7078352473574));
#37061=CARTESIAN_POINT('Ctrl Pts',(30.3311478274255,30.245555587262,-17.4622796600955));
#37062=CARTESIAN_POINT('Ctrl Pts',(30.3311478274255,47.7078352473574,12.7832759271664));
#37063=CARTESIAN_POINT('Ctrl Pts',(30.3311478274255,17.4622796600955,30.245555587262));
#37064=CARTESIAN_POINT('Ctrl Pts',(30.3311478274255,-12.7832759271664,47.7078352473574));
#37065=CARTESIAN_POINT('Ctrl Pts',(30.3311478274255,-30.245555587262,17.4622796600955));
#37066=CARTESIAN_POINT('Ctrl Pts',(30.3311478274255,-46.9455930096601,-11.4630336437997));
#37067=CARTESIAN_POINT('Ctrl Pts',(30.3311478274255,-18.7939298193791,-29.4365936489566));
#37068=CARTESIAN_POINT('Ctrl Pts',(29.9897712690917,-18.7116961278613,-29.3077924996107));
#37069=CARTESIAN_POINT('Ctrl Pts',(29.9897712690917,-18.0577698358324,-29.7252947753835));
#37070=CARTESIAN_POINT('Ctrl Pts',(29.9897712690917,-17.3858726641896,-30.1132147882992));
#37071=CARTESIAN_POINT('Ctrl Pts',(29.9897712690917,12.7273421241096,-47.4990874524888));
#37072=CARTESIAN_POINT('Ctrl Pts',(29.9897712690917,30.1132147882992,-17.3858726641896));
#37073=CARTESIAN_POINT('Ctrl Pts',(29.9897712690917,47.4990874524888,12.7273421241096));
#37074=CARTESIAN_POINT('Ctrl Pts',(29.9897712690917,17.3858726641896,30.1132147882992));
#37075=CARTESIAN_POINT('Ctrl Pts',(29.9897712690917,-12.7273421241096,47.4990874524888));
#37076=CARTESIAN_POINT('Ctrl Pts',(29.9897712690917,-30.1132147882992,17.3858726641896));
#37077=CARTESIAN_POINT('Ctrl Pts',(29.9897712690917,-46.7401804402414,-11.4128766206768));
#37078=CARTESIAN_POINT('Ctrl Pts',(29.9897712690917,-18.7116961278613,-29.3077924996107));
#37079=CARTESIAN_POINT('Ctrl Pts',(29.4666899049319,-18.5852252487451,-29.1097034403905));
#37080=CARTESIAN_POINT('Ctrl Pts',(29.4666899049319,-17.935718792976,-29.5243838511923));
#37081=CARTESIAN_POINT('Ctrl Pts',(29.4666899049319,-17.2683629213518,-29.9096819433198));
#37082=CARTESIAN_POINT('Ctrl Pts',(29.4666899049319,12.641319021968,-47.1780448646716));
#37083=CARTESIAN_POINT('Ctrl Pts',(29.4666899049319,29.9096819433198,-17.2683629213518));
#37084=CARTESIAN_POINT('Ctrl Pts',(29.4666899049319,47.1780448646716,12.641319021968));
#37085=CARTESIAN_POINT('Ctrl Pts',(29.4666899049319,17.2683629213518,29.9096819433198));
#37086=CARTESIAN_POINT('Ctrl Pts',(29.4666899049319,-12.641319021968,47.1780448646716));
#37087=CARTESIAN_POINT('Ctrl Pts',(29.4666899049319,-29.9096819433198,17.2683629213518));
#37088=CARTESIAN_POINT('Ctrl Pts',(29.4666899049319,-46.4242672450966,-11.3357378872557));
#37089=CARTESIAN_POINT('Ctrl Pts',(29.4666899049319,-18.5852252487451,-29.1097034403905));
#37090=CARTESIAN_POINT('Ctrl Pts',(28.7471241621752,-18.4103340474916,-28.8357745030392));
#37091=CARTESIAN_POINT('Ctrl Pts',(28.7471241621752,-17.7669395953572,-29.246552676757));
#37092=CARTESIAN_POINT('Ctrl Pts',(28.7471241621752,-17.105863694435,-29.6282250261092));
#37093=CARTESIAN_POINT('Ctrl Pts',(28.7471241621752,12.5223613316742,-46.7340887205442));
#37094=CARTESIAN_POINT('Ctrl Pts',(28.7471241621752,29.6282250261092,-17.105863694435));
#37095=CARTESIAN_POINT('Ctrl Pts',(28.7471241621752,46.7340887205442,12.5223613316742));
#37096=CARTESIAN_POINT('Ctrl Pts',(28.7471241621752,17.105863694435,29.6282250261092));
#37097=CARTESIAN_POINT('Ctrl Pts',(28.7471241621752,-12.5223613316742,46.7340887205442));
#37098=CARTESIAN_POINT('Ctrl Pts',(28.7471241621752,-29.6282250261092,17.105863694435));
#37099=CARTESIAN_POINT('Ctrl Pts',(28.7471241621752,-45.9874043199967,-11.2290660127069));
#37100=CARTESIAN_POINT('Ctrl Pts',(28.7471241621752,-18.4103340474916,-28.8357745030392));
#37101=CARTESIAN_POINT('Ctrl Pts',(27.8100958442934,-18.1817092625453,-28.4776836217162));
#37102=CARTESIAN_POINT('Ctrl Pts',(27.8100958442934,-17.5463046664274,-28.8833606347823));
#37103=CARTESIAN_POINT('Ctrl Pts',(27.8100958442934,-16.8934381948013,-29.2602932679205));
#37104=CARTESIAN_POINT('Ctrl Pts',(27.8100958442934,12.3668550731192,-46.1537314627218));
#37105=CARTESIAN_POINT('Ctrl Pts',(27.8100958442934,29.2602932679205,-16.8934381948013));
#37106=CARTESIAN_POINT('Ctrl Pts',(27.8100958442934,46.1537314627218,12.3668550731192));
#37107=CARTESIAN_POINT('Ctrl Pts',(27.8100958442934,16.8934381948013,29.2602932679205));
#37108=CARTESIAN_POINT('Ctrl Pts',(27.8100958442934,-12.3668550731192,46.1537314627218));
#37109=CARTESIAN_POINT('Ctrl Pts',(27.8100958442934,-29.2602932679205,16.8934381948013));
#37110=CARTESIAN_POINT('Ctrl Pts',(27.8100958442934,-45.4163196022628,-11.0896202647003));
#37111=CARTESIAN_POINT('Ctrl Pts',(27.8100958442934,-18.1817092625453,-28.4776836217162));
#37112=CARTESIAN_POINT('Ctrl Pts',(26.8343111708818,-17.9446806017473,-28.1064299010669));
#37113=CARTESIAN_POINT('Ctrl Pts',(26.8343111708818,-17.3175595557791,-28.5068182430991));
#37114=CARTESIAN_POINT('Ctrl Pts',(26.8343111708818,-16.6732042787396,-28.8788369357517));
#37115=CARTESIAN_POINT('Ctrl Pts',(26.8343111708818,12.2056326570121,-45.5520412144912));
#37116=CARTESIAN_POINT('Ctrl Pts',(26.8343111708818,28.8788369357517,-16.6732042787396));
#37117=CARTESIAN_POINT('Ctrl Pts',(26.8343111708818,45.5520412144912,12.2056326570121));
#37118=CARTESIAN_POINT('Ctrl Pts',(26.8343111708818,16.6732042787396,28.8788369357517));
#37119=CARTESIAN_POINT('Ctrl Pts',(26.8343111708818,-12.2056326570121,45.5520412144912));
#37120=CARTESIAN_POINT('Ctrl Pts',(26.8343111708818,-28.8788369357517,16.6732042787396));
#37121=CARTESIAN_POINT('Ctrl Pts',(26.8343111708818,-44.8242427376375,-10.9450487174303));
#37122=CARTESIAN_POINT('Ctrl Pts',(26.8343111708818,-17.9446806017473,-28.1064299010669));
#37123=CARTESIAN_POINT('Ctrl Pts',(25.8181479469611,-17.7025946652472,-27.7272550606068));
#37124=CARTESIAN_POINT('Ctrl Pts',(25.8181479469611,-17.0839339083798,-28.1222418918016));
#37125=CARTESIAN_POINT('Ctrl Pts',(25.8181479469611,-16.4482714219305,-28.4892417994668));
#37126=CARTESIAN_POINT('Ctrl Pts',(25.8181479469611,12.0409703775363,-44.9375132213974));
#37127=CARTESIAN_POINT('Ctrl Pts',(25.8181479469611,28.4892417994668,-16.4482714219305));
#37128=CARTESIAN_POINT('Ctrl Pts',(25.8181479469611,44.9375132213974,12.0409703775363));
#37129=CARTESIAN_POINT('Ctrl Pts',(25.8181479469611,16.4482714219305,28.4892417994668));
#37130=CARTESIAN_POINT('Ctrl Pts',(25.8181479469611,-12.0409703775363,44.9375132213974));
#37131=CARTESIAN_POINT('Ctrl Pts',(25.8181479469611,-28.4892417994668,16.4482714219305));
#37132=CARTESIAN_POINT('Ctrl Pts',(25.8181479469611,-44.2195332406074,-10.7973925719907));
#37133=CARTESIAN_POINT('Ctrl Pts',(25.8181479469611,-17.7025946652472,-27.7272550606068));
#37134=CARTESIAN_POINT('Ctrl Pts',(24.7595197917227,-17.4614959928472,-27.3496265541183));
#37135=CARTESIAN_POINT('Ctrl Pts',(24.7595197917227,-16.8512610227058,-27.739233902677));
#37136=CARTESIAN_POINT('Ctrl Pts',(24.7595197917227,-16.2242558762949,-28.1012354927406));
#37137=CARTESIAN_POINT('Ctrl Pts',(24.7595197917227,11.8769796164457,-44.3254913690355));
#37138=CARTESIAN_POINT('Ctrl Pts',(24.7595197917227,28.1012354927406,-16.2242558762949));
#37139=CARTESIAN_POINT('Ctrl Pts',(24.7595197917227,44.3254913690355,11.8769796164457));
#37140=CARTESIAN_POINT('Ctrl Pts',(24.7595197917227,16.2242558762949,28.1012354927406));
#37141=CARTESIAN_POINT('Ctrl Pts',(24.7595197917227,-11.8769796164457,44.3254913690355));
#37142=CARTESIAN_POINT('Ctrl Pts',(24.7595197917227,-28.1012354927406,16.2242558762949));
#37143=CARTESIAN_POINT('Ctrl Pts',(24.7595197917227,-43.6172898429552,-10.6503385912768));
#37144=CARTESIAN_POINT('Ctrl Pts',(24.7595197917227,-17.4614959928472,-27.3496265541183));
#37145=CARTESIAN_POINT('Ctrl Pts',(23.6563574780851,-17.229354682426,-26.9860278023044));
#37146=CARTESIAN_POINT('Ctrl Pts',(23.6563574780851,-16.627232461942,-27.370455528196));
#37147=CARTESIAN_POINT('Ctrl Pts',(23.6563574780851,-16.0085630157705,-27.7276444994825));
#37148=CARTESIAN_POINT('Ctrl Pts',(23.6563574780851,11.719081483712,-43.736207515253));
#37149=CARTESIAN_POINT('Ctrl Pts',(23.6563574780851,27.7276444994825,-16.0085630157705));
#37150=CARTESIAN_POINT('Ctrl Pts',(23.6563574780851,43.736207515253,11.719081483712));
#37151=CARTESIAN_POINT('Ctrl Pts',(23.6563574780851,16.0085630157705,27.7276444994825));
#37152=CARTESIAN_POINT('Ctrl Pts',(23.6563574780851,-11.719081483712,43.736207515253));
#37153=CARTESIAN_POINT('Ctrl Pts',(23.6563574780851,-27.7276444994825,16.0085630157705));
#37154=CARTESIAN_POINT('Ctrl Pts',(23.6563574780851,-43.0374211521332,-10.5087479991522));
#37155=CARTESIAN_POINT('Ctrl Pts',(23.6563574780851,-17.229354682426,-26.9860278023044));
#37156=CARTESIAN_POINT('Ctrl Pts',(22.5073180101405,-17.0145388530744,-26.649565639321));
#37157=CARTESIAN_POINT('Ctrl Pts',(22.5073180101405,-16.419923900654,-27.029200315079));
#37158=CARTESIAN_POINT('Ctrl Pts',(22.5073180101405,-15.8089680335819,-27.3819358493961));
#37159=CARTESIAN_POINT('Ctrl Pts',(22.5073180101405,11.5729678158142,-43.190903882978));
#37160=CARTESIAN_POINT('Ctrl Pts',(22.5073180101405,27.3819358493961,-15.8089680335819));
#37161=CARTESIAN_POINT('Ctrl Pts',(22.5073180101405,43.190903882978,11.5729678158142));
#37162=CARTESIAN_POINT('Ctrl Pts',(22.5073180101405,15.8089680335819,27.3819358493961));
#37163=CARTESIAN_POINT('Ctrl Pts',(22.5073180101405,-11.5729678158142,43.190903882978));
#37164=CARTESIAN_POINT('Ctrl Pts',(22.5073180101405,-27.3819358493961,15.8089680335819));
#37165=CARTESIAN_POINT('Ctrl Pts',(22.5073180101405,-42.5008299977716,-10.3777247856603));
#37166=CARTESIAN_POINT('Ctrl Pts',(22.5073180101405,-17.0145388530744,-26.649565639321));
#37167=CARTESIAN_POINT('Ctrl Pts',(21.3125219557939,-16.8244723890963,-26.3518679613905));
#37168=CARTESIAN_POINT('Ctrl Pts',(21.3125219557939,-16.2364997772301,-26.727261803997));
#37169=CARTESIAN_POINT('Ctrl Pts',(21.3125219557939,-15.632368792237,-27.0760569908086));
#37170=CARTESIAN_POINT('Ctrl Pts',(21.3125219557939,11.4436881985716,-42.7084257830456));
#37171=CARTESIAN_POINT('Ctrl Pts',(21.3125219557939,27.0760569908086,-15.632368792237));
#37172=CARTESIAN_POINT('Ctrl Pts',(21.3125219557939,42.7084257830456,11.4436881985716));
#37173=CARTESIAN_POINT('Ctrl Pts',(21.3125219557939,15.632368792237,27.0760569908086));
#37174=CARTESIAN_POINT('Ctrl Pts',(21.3125219557939,-11.4436881985716,42.7084257830456));
#37175=CARTESIAN_POINT('Ctrl Pts',(21.3125219557939,-27.0760569908086,15.632368792237));
#37176=CARTESIAN_POINT('Ctrl Pts',(21.3125219557939,-42.0260605935833,-10.2617970211066));
#37177=CARTESIAN_POINT('Ctrl Pts',(21.3125219557939,-16.8244723890963,-26.3518679613905));
#37178=CARTESIAN_POINT('Ctrl Pts',(20.0742472323676,-16.6643225955233,-26.1010282252799));
#37179=CARTESIAN_POINT('Ctrl Pts',(20.0742472323676,-16.0819468125049,-26.4728487465358));
#37180=CARTESIAN_POINT('Ctrl Pts',(20.0742472323676,-15.4835664656478,-26.8183238008715));
#37181=CARTESIAN_POINT('Ctrl Pts',(20.0742472323676,11.3347573352238,-42.3018902665193));
#37182=CARTESIAN_POINT('Ctrl Pts',(20.0742472323676,26.8183238008715,-15.4835664656478));
#37183=CARTESIAN_POINT('Ctrl Pts',(20.0742472323676,42.3018902665193,11.3347573352238));
#37184=CARTESIAN_POINT('Ctrl Pts',(20.0742472323676,15.4835664656478,26.8183238008715));
#37185=CARTESIAN_POINT('Ctrl Pts',(20.0742472323676,-11.3347573352238,42.3018902665193));
#37186=CARTESIAN_POINT('Ctrl Pts',(20.0742472323676,-26.8183238008715,15.4835664656478));
#37187=CARTESIAN_POINT('Ctrl Pts',(20.0742472323676,-41.6260204156154,-10.1641164141543));
#37188=CARTESIAN_POINT('Ctrl Pts',(20.0742472323676,-16.6643225955233,-26.1010282252799));
#37189=CARTESIAN_POINT('Ctrl Pts',(18.7979917002302,-16.5352770548748,-25.8989065200918));
#37190=CARTESIAN_POINT('Ctrl Pts',(18.7979917002302,-15.9574110860028,-26.2678477295776));
#37191=CARTESIAN_POINT('Ctrl Pts',(18.7979917002302,-15.3636644897785,-26.6106474867381));
#37192=CARTESIAN_POINT('Ctrl Pts',(18.7979917002302,11.2469829969596,-41.9743119765166));
#37193=CARTESIAN_POINT('Ctrl Pts',(18.7979917002302,26.6106474867381,-15.3636644897785));
#37194=CARTESIAN_POINT('Ctrl Pts',(18.7979917002302,41.9743119765166,11.2469829969596));
#37195=CARTESIAN_POINT('Ctrl Pts',(18.7979917002302,15.3636644897785,26.6106474867381));
#37196=CARTESIAN_POINT('Ctrl Pts',(18.7979917002302,-11.2469829969596,41.9743119765166));
#37197=CARTESIAN_POINT('Ctrl Pts',(18.7979917002302,-26.6106474867381,15.3636644897785));
#37198=CARTESIAN_POINT('Ctrl Pts',(18.7979917002302,-41.303675941138,-10.0854073102973));
#37199=CARTESIAN_POINT('Ctrl Pts',(18.7979917002302,-16.5352770548748,-25.8989065200918));
#37200=CARTESIAN_POINT('Ctrl Pts',(17.4917404060759,-16.4351406788133,-25.7420647185138));
#37201=CARTESIAN_POINT('Ctrl Pts',(17.4917404060759,-15.8607742221527,-26.1087716481884));
#37202=CARTESIAN_POINT('Ctrl Pts',(17.4917404060759,-15.2706233100072,-26.4494954361781));
#37203=CARTESIAN_POINT('Ctrl Pts',(17.4917404060759,11.1788721261709,-41.7201187461852));
#37204=CARTESIAN_POINT('Ctrl Pts',(17.4917404060759,26.4494954361781,-15.2706233100072));
#37205=CARTESIAN_POINT('Ctrl Pts',(17.4917404060759,41.7201187461852,11.1788721261709));
#37206=CARTESIAN_POINT('Ctrl Pts',(17.4917404060759,15.2706233100072,26.4494954361781));
#37207=CARTESIAN_POINT('Ctrl Pts',(17.4917404060759,-11.1788721261709,41.7201187461852));
#37208=CARTESIAN_POINT('Ctrl Pts',(17.4917404060759,-26.4494954361781,15.2706233100072));
#37209=CARTESIAN_POINT('Ctrl Pts',(17.4917404060759,-41.0535440314616,-10.0243308532288));
#37210=CARTESIAN_POINT('Ctrl Pts',(17.4917404060759,-16.4351406788133,-25.7420647185138));
#37211=CARTESIAN_POINT('Ctrl Pts',(16.1647270995715,-16.3596108683728,-25.6237637373094));
#37212=CARTESIAN_POINT('Ctrl Pts',(16.1647270995715,-15.7878839869031,-25.988785417954));
#37213=CARTESIAN_POINT('Ctrl Pts',(16.1647270995715,-15.2004451894512,-26.3279433657953));
#37214=CARTESIAN_POINT('Ctrl Pts',(16.1647270995715,11.1274981763441,-41.5283885552464));
#37215=CARTESIAN_POINT('Ctrl Pts',(16.1647270995715,26.3279433657953,-15.2004451894512));
#37216=CARTESIAN_POINT('Ctrl Pts',(16.1647270995715,41.5283885552464,11.1274981763441));
#37217=CARTESIAN_POINT('Ctrl Pts',(16.1647270995715,15.2004451894512,26.3279433657953));
#37218=CARTESIAN_POINT('Ctrl Pts',(16.1647270995715,-11.1274981763441,41.5283885552464));
#37219=CARTESIAN_POINT('Ctrl Pts',(16.1647270995715,-26.3279433657953,15.2004451894512));
#37220=CARTESIAN_POINT('Ctrl Pts',(16.1647270995715,-40.8648771706659,-9.97826274685029));
#37221=CARTESIAN_POINT('Ctrl Pts',(16.1647270995715,-16.3596108683728,-25.6237637373094));
#37222=CARTESIAN_POINT('Ctrl Pts',(14.8263876417415,-16.3032840624315,-25.5355400760542));
#37223=CARTESIAN_POINT('Ctrl Pts',(14.8263876417415,-15.7335256598799,-25.8993049721986));
#37224=CARTESIAN_POINT('Ctrl Pts',(14.8263876417415,-15.1481094381123,-26.2372951854241));
#37225=CARTESIAN_POINT('Ctrl Pts',(14.8263876417415,11.0891857473118,-41.3854046235364));
#37226=CARTESIAN_POINT('Ctrl Pts',(14.8263876417415,26.2372951854241,-15.1481094381123));
#37227=CARTESIAN_POINT('Ctrl Pts',(14.8263876417415,41.3854046235364,11.0891857473118));
#37228=CARTESIAN_POINT('Ctrl Pts',(14.8263876417415,15.1481094381123,26.2372951854241));
#37229=CARTESIAN_POINT('Ctrl Pts',(14.8263876417415,-11.0891857473118,41.3854046235364));
#37230=CARTESIAN_POINT('Ctrl Pts',(14.8263876417415,-26.2372951854241,15.1481094381123));
#37231=CARTESIAN_POINT('Ctrl Pts',(14.8263876417415,-40.7241777356532,-9.94390718216752));
#37232=CARTESIAN_POINT('Ctrl Pts',(14.8263876417415,-16.3032840624315,-25.5355400760542));
#37233=CARTESIAN_POINT('Ctrl Pts',(13.4853470903953,-16.260659159851,-25.4687774591536));
#37234=CARTESIAN_POINT('Ctrl Pts',(13.4853470903953,-15.6923903894687,-25.8315912927267));
#37235=CARTESIAN_POINT('Ctrl Pts',(13.4853470903953,-15.1085047372063,-26.1686978312363));
#37236=CARTESIAN_POINT('Ctrl Pts',(13.4853470903953,11.06019309403,-41.2772025684426));
#37237=CARTESIAN_POINT('Ctrl Pts',(13.4853470903953,26.1686978312363,-15.1085047372063));
#37238=CARTESIAN_POINT('Ctrl Pts',(13.4853470903953,41.2772025684426,11.06019309403));
#37239=CARTESIAN_POINT('Ctrl Pts',(13.4853470903953,15.1085047372063,26.1686978312363));
#37240=CARTESIAN_POINT('Ctrl Pts',(13.4853470903953,-11.06019309403,41.2772025684426));
#37241=CARTESIAN_POINT('Ctrl Pts',(13.4853470903953,-26.1686978312363,15.1085047372063));
#37242=CARTESIAN_POINT('Ctrl Pts',(13.4853470903953,-40.617704456895,-9.91790885733393));
#37243=CARTESIAN_POINT('Ctrl Pts',(13.4853470903953,-16.260659159851,-25.4687774591536));
#37244=CARTESIAN_POINT('Ctrl Pts',(12.1482076787549,-16.2272643834928,-25.4164718226475));
#37245=CARTESIAN_POINT('Ctrl Pts',(12.1482076787549,-15.660162675793,-25.778540539635));
#37246=CARTESIAN_POINT('Ctrl Pts',(12.1482076787549,-15.0774761588537,-26.1149547570431));
#37247=CARTESIAN_POINT('Ctrl Pts',(12.1482076787549,11.0374785981893,-41.1924309158968));
#37248=CARTESIAN_POINT('Ctrl Pts',(12.1482076787549,26.1149547570431,-15.0774761588537));
#37249=CARTESIAN_POINT('Ctrl Pts',(12.1482076787549,41.1924309158968,11.0374785981893));
#37250=CARTESIAN_POINT('Ctrl Pts',(12.1482076787549,15.0774761588537,26.1149547570431));
#37251=CARTESIAN_POINT('Ctrl Pts',(12.1482076787549,-11.0374785981893,41.1924309158968));
#37252=CARTESIAN_POINT('Ctrl Pts',(12.1482076787549,-26.1149547570431,15.0774761588537));
#37253=CARTESIAN_POINT('Ctrl Pts',(12.1482076787549,-40.534287226192,-9.89754028893977));
#37254=CARTESIAN_POINT('Ctrl Pts',(12.1482076787549,-16.2272643834928,-25.4164718226475));
#37255=CARTESIAN_POINT('Ctrl Pts',(10.8190675759626,-16.2001953420791,-25.3740740708084));
#37256=CARTESIAN_POINT('Ctrl Pts',(10.8190675759626,-15.6340396286792,-25.7355388133451));
#37257=CARTESIAN_POINT('Ctrl Pts',(10.8190675759626,-15.0523251033885,-26.0713918511132));
#37258=CARTESIAN_POINT('Ctrl Pts',(10.8190675759626,11.0190667477248,-41.1237169545017));
#37259=CARTESIAN_POINT('Ctrl Pts',(10.8190675759626,26.0713918511132,-15.0523251033885));
#37260=CARTESIAN_POINT('Ctrl Pts',(10.8190675759626,41.1237169545017,11.0190667477248));
#37261=CARTESIAN_POINT('Ctrl Pts',(10.8190675759626,15.0523251033885,26.0713918511132));
#37262=CARTESIAN_POINT('Ctrl Pts',(10.8190675759626,-11.0190667477248,41.1237169545017));
#37263=CARTESIAN_POINT('Ctrl Pts',(10.8190675759626,-26.0713918511132,15.0523251033885));
#37264=CARTESIAN_POINT('Ctrl Pts',(10.8190675759626,-40.4666711281441,-9.88102999357242));
#37265=CARTESIAN_POINT('Ctrl Pts',(10.8190675759626,-16.2001953420791,-25.3740740708084));
#37266=CARTESIAN_POINT('Ctrl Pts',(9.50027713254189,-16.1776521900286,-25.3387651379321));
#37267=CARTESIAN_POINT('Ctrl Pts',(9.50027713254189,-15.6122843025816,-25.6997268893331));
#37268=CARTESIAN_POINT('Ctrl Pts',(9.50027713254189,-15.0313792538877,-26.0351125755702));
#37269=CARTESIAN_POINT('Ctrl Pts',(9.50027713254189,11.0037333216825,-41.0664918294579));
#37270=CARTESIAN_POINT('Ctrl Pts',(9.50027713254189,26.0351125755702,-15.0313792538877));
#37271=CARTESIAN_POINT('Ctrl Pts',(9.5002771325419,41.0664918294579,11.0037333216825));
#37272=CARTESIAN_POINT('Ctrl Pts',(9.5002771325419,15.0313792538877,26.0351125755702));
#37273=CARTESIAN_POINT('Ctrl Pts',(9.5002771325419,-11.0037333216825,41.0664918294579));
#37274=CARTESIAN_POINT('Ctrl Pts',(9.50027713254189,-26.0351125755702,15.0313792538877));
#37275=CARTESIAN_POINT('Ctrl Pts',(9.50027713254189,-40.4103603059007,-9.86728018643389));
#37276=CARTESIAN_POINT('Ctrl Pts',(9.50027713254189,-16.1776521900286,-25.3387651379321));
#37277=CARTESIAN_POINT('Ctrl Pts',(8.45435372222587,-16.1625070777669,-25.3150436214797));
#37278=CARTESIAN_POINT('Ctrl Pts',(8.45435372222587,-15.5976684735573,-25.6756674495416));
#37279=CARTESIAN_POINT('Ctrl Pts',(8.45435372222587,-15.0173072536015,-26.0107391561104));
#37280=CARTESIAN_POINT('Ctrl Pts',(8.45435372222587,10.9934319025089,-41.0280464097118));
#37281=CARTESIAN_POINT('Ctrl Pts',(8.45435372222587,26.0107391561104,-15.0173072536015));
#37282=CARTESIAN_POINT('Ctrl Pts',(8.45435372222587,41.0280464097118,10.9934319025089));
#37283=CARTESIAN_POINT('Ctrl Pts',(8.45435372222587,15.0173072536015,26.0107391561104));
#37284=CARTESIAN_POINT('Ctrl Pts',(8.45435372222587,-10.9934319025089,41.0280464097118));
#37285=CARTESIAN_POINT('Ctrl Pts',(8.45435372222587,-26.0107391561104,15.0173072536015));
#37286=CARTESIAN_POINT('Ctrl Pts',(8.45435372222587,-40.3725291400319,-9.85804268618443));
#37287=CARTESIAN_POINT('Ctrl Pts',(8.45435372222587,-16.1625070777669,-25.3150436214797));
#37288=CARTESIAN_POINT('Ctrl Pts',(7.67514864245731,-16.1526223715399,-25.2995613842179));
#37289=CARTESIAN_POINT('Ctrl Pts',(7.67514864245731,-15.5881292127269,-25.6599646610633));
#37290=CARTESIAN_POINT('Ctrl Pts',(7.67514864245731,-15.0081229315276,-25.9948314436453));
#37291=CARTESIAN_POINT('Ctrl Pts',(7.67514864245731,10.9867085121177,-41.0029543751729));
#37292=CARTESIAN_POINT('Ctrl Pts',(7.67514864245731,25.9948314436453,-15.0081229315276));
#37293=CARTESIAN_POINT('Ctrl Pts',(7.67514864245731,41.0029543751729,10.9867085121177));
#37294=CARTESIAN_POINT('Ctrl Pts',(7.67514864245731,15.0081229315276,25.9948314436453));
#37295=CARTESIAN_POINT('Ctrl Pts',(7.67514864245731,-10.9867085121177,41.0029543751729));
#37296=CARTESIAN_POINT('Ctrl Pts',(7.67514864245731,-25.9948314436453,15.0081229315276));
#37297=CARTESIAN_POINT('Ctrl Pts',(7.67514864245731,-40.3478380083732,-9.85201367995056));
#37298=CARTESIAN_POINT('Ctrl Pts',(7.67514864245731,-16.1526223715399,-25.2995613842179));
#37299=CARTESIAN_POINT('Ctrl Pts',(7.15799654185577,-16.1466853364124,-25.2902623130707));
#37300=CARTESIAN_POINT('Ctrl Pts',(7.15799654185577,-15.5823996619098,-25.6505331205953));
#37301=CARTESIAN_POINT('Ctrl Pts',(7.15799654185577,-15.0026065670023,-25.9852768200144));
#37302=CARTESIAN_POINT('Ctrl Pts',(7.15799654185577,10.9826702530121,-40.9878833870167));
#37303=CARTESIAN_POINT('Ctrl Pts',(7.15799654185577,25.9852768200144,-15.0026065670023));
#37304=CARTESIAN_POINT('Ctrl Pts',(7.15799654185577,40.9878833870167,10.9826702530121));
#37305=CARTESIAN_POINT('Ctrl Pts',(7.15799654185577,15.0026065670023,25.9852768200144));
#37306=CARTESIAN_POINT('Ctrl Pts',(7.15799654185577,-10.9826702530121,40.9878833870167));
#37307=CARTESIAN_POINT('Ctrl Pts',(7.15799654185577,-25.9852768200144,15.0026065670023));
#37308=CARTESIAN_POINT('Ctrl Pts',(7.15799654185577,-40.3330078138659,-9.84839248767921));
#37309=CARTESIAN_POINT('Ctrl Pts',(7.15799654185577,-16.1466853364124,-25.2902623130707));
#37310=CARTESIAN_POINT('Ctrl Pts',(6.9,-16.1438799960867,-25.2858683590648));
#37311=CARTESIAN_POINT('Ctrl Pts',(6.9,-15.5796923611089,-25.6460765727998));
#37312=CARTESIAN_POINT('Ctrl Pts',(6.9,-15.,-25.9807621135332));
#37313=CARTESIAN_POINT('Ctrl Pts',(6.9,10.9807621135331,-40.9807621135332));
#37314=CARTESIAN_POINT('Ctrl Pts',(6.9,25.9807621135332,-15.));
#37315=CARTESIAN_POINT('Ctrl Pts',(6.9,40.9807621135332,10.9807621135331));
#37316=CARTESIAN_POINT('Ctrl Pts',(6.9,15.,25.9807621135332));
#37317=CARTESIAN_POINT('Ctrl Pts',(6.9,-10.9807621135331,40.9807621135332));
#37318=CARTESIAN_POINT('Ctrl Pts',(6.9,-25.9807621135332,15.));
#37319=CARTESIAN_POINT('Ctrl Pts',(6.9,-40.3260003190816,-9.84668141868802));
#37320=CARTESIAN_POINT('Ctrl Pts',(6.9,-16.1438799960867,-25.2858683590648));
#37321=CARTESIAN_POINT('Ctrl Pts',(6.9,8.61681422303452,-28.7358750109634));
#37322=CARTESIAN_POINT('Ctrl Pts',(7.85773098116326,6.72950262532882,-29.3220126177434));
#37323=CARTESIAN_POINT('Ctrl Pts',(8.88781981167334,4.83176468807715,-29.7139609348499));
#37324=CARTESIAN_POINT('Ctrl Pts',(10.5914578196776,1.83991777043966,-30.0626260759601));
#37325=CARTESIAN_POINT('Ctrl Pts',(11.2365058953701,0.737334477600518,-30.1308526921615));
#37326=CARTESIAN_POINT('Ctrl Pts',(12.0558885382926,-0.564998386426074,
-30.1493644860168));
#37327=CARTESIAN_POINT('Ctrl Pts',(12.1875764958397,-0.770798830274841,
-30.1503477937894));
#37328=CARTESIAN_POINT('Ctrl Pts',(13.194901830313,-2.32835059063961,-30.1433772121647));
#37329=CARTESIAN_POINT('Ctrl Pts',(14.2258982134098,-3.91692083548089,-30.0606334052373));
#37330=CARTESIAN_POINT('Ctrl Pts',(18.2616480823244,-8.94354621773405,-29.4024246647732));
#37331=CARTESIAN_POINT('Ctrl Pts',(21.0496416709525,-11.660889676038,-28.796919295079));
#37332=CARTESIAN_POINT('Ctrl Pts',(25.8000196361138,-14.7241675584603,-29.3778263502455));
#37333=CARTESIAN_POINT('Ctrl Pts',(26.8976561124457,-15.1580512376427,-29.7353019177929));
#37334=CARTESIAN_POINT('Ctrl Pts',(28.0045908801237,-15.5447817028247,-30.0977443108623));
#37335=CARTESIAN_POINT('Ctrl Pts',(28.5235971652406,-15.6994510084801,-30.2828992744991));
#37336=CARTESIAN_POINT('Ctrl Pts',(29.0834839543824,-15.8677990842846,-30.4804113157011));
#37337=CARTESIAN_POINT('Ctrl Pts',(29.1146288039499,-15.877207296405,-30.4913713634453));
#37338=CARTESIAN_POINT('Ctrl Pts',(29.5949306848436,-16.0210111630069,-30.6609898319163));
#37339=CARTESIAN_POINT('Ctrl Pts',(30.0492939924726,-16.1312811324031,-30.8338536064743));
#37340=CARTESIAN_POINT('Ctrl Pts',(30.5,-16.229443021655,-31.0097594187194));
#37341=CARTESIAN_POINT('Ctrl Pts',(6.45331003273164,4.07387898226151,-10.2495589536195));
#37342=CARTESIAN_POINT('Ctrl Pts',(7.20830533428676,3.54117612793134,-10.4589493929845));
#37343=CARTESIAN_POINT('Ctrl Pts',(7.99943720515023,3.00808536723907,-10.6278530262204));
#37344=CARTESIAN_POINT('Ctrl Pts',(9.76195392812149,1.87226624217412,-10.8974188156737));
#37345=CARTESIAN_POINT('Ctrl Pts',(10.7319699357145,1.2567580486118,-10.978614804603));
#37346=CARTESIAN_POINT('Ctrl Pts',(12.6618070777417,0.165209663835397,-11.0581512103982));
#37347=CARTESIAN_POINT('Ctrl Pts',(13.6366888866736,-0.364704064273056,
-11.0460663569154));
#37348=CARTESIAN_POINT('Ctrl Pts',(15.55636942495,-1.27025231764748,-10.9884970038505));
#37349=CARTESIAN_POINT('Ctrl Pts',(16.5294822240034,-1.69980161462952,-10.9232664847119));
#37350=CARTESIAN_POINT('Ctrl Pts',(18.4405353898674,-2.41132585012622,-10.79829507883));
#37351=CARTESIAN_POINT('Ctrl Pts',(19.4148048972756,-2.74047342809724,-10.7128845485963));
#37352=CARTESIAN_POINT('Ctrl Pts',(20.6320159197513,-3.0737286362331,-10.6248232626625));
#37353=CARTESIAN_POINT('Ctrl Pts',(21.104508195865,-3.19855905527614,-10.5890632628362));
#37354=CARTESIAN_POINT('Ctrl Pts',(22.0534615876999,-3.42883778652051,-10.5175158204589));
#37355=CARTESIAN_POINT('Ctrl Pts',(22.7823820470182,-3.58029681662341,-10.4664588970829));
#37356=CARTESIAN_POINT('Ctrl Pts',(23.3297776630266,-3.67835397010644,-10.4341170945838));
#37357=CARTESIAN_POINT('Ctrl Pts',(23.4470599317458,-3.69902619132825,-10.4271412460567));
#37358=CARTESIAN_POINT('Ctrl Pts',(23.6811266122299,-3.73910834650869,-10.4133903945396));
#37359=CARTESIAN_POINT('Ctrl Pts',(24.0941730950848,-3.80664723977492,-10.3895545652128));
#37360=CARTESIAN_POINT('Ctrl Pts',(24.6899146335615,-3.89464075109998,-10.3570603924451));
#37361=CARTESIAN_POINT('Ctrl Pts',(25.291236117096,-3.96994444386567,-10.3283061836387));
#37362=CARTESIAN_POINT('Ctrl Pts',(25.7735285180351,-4.02162740546582,-10.308597305488));
#37363=CARTESIAN_POINT('Ctrl Pts',(26.0148283477099,-4.04448759176679,-10.3000025859217));
#37364=CARTESIAN_POINT('Ctrl Pts',(26.5981242438444,-4.09600397233591,-10.2809495486037));
#37365=CARTESIAN_POINT('Ctrl Pts',(27.5413774795629,-4.1475207788653,-10.2607319091994));
#37366=CARTESIAN_POINT('Ctrl Pts',(28.5384263877914,-4.17105255246827,-10.2503835882543));
#37367=CARTESIAN_POINT('Ctrl Pts',(29.1235503058368,-4.18584784382925,-10.2444533826691));
#37368=CARTESIAN_POINT('Ctrl Pts',(29.28127198738,-4.1893484810251,-10.2430815653883));
#37369=CARTESIAN_POINT('Ctrl Pts',(29.6033573831699,-4.19465178436654,-10.2409825864505));
#37370=CARTESIAN_POINT('Ctrl Pts',(30.1682075695059,-4.19956029863432,-10.23904328544));
#37371=CARTESIAN_POINT('Ctrl Pts',(31.3151152846708,-4.19601580459665,-10.2404426493562));
#37372=CARTESIAN_POINT('Ctrl Pts',(32.3203773995796,-4.18330340731801,-10.2455622764131));
#37373=CARTESIAN_POINT('Ctrl Pts',(33.1677006908681,-4.18329188254757,-10.2455713422049));
#37374=CARTESIAN_POINT('Ctrl Pts',(33.4949132850989,-4.18329063364474,-10.2455724350351));
#37375=CARTESIAN_POINT('Ctrl Pts',(34.1541785734606,-4.18328832445805,-10.2455743198854));
#37376=CARTESIAN_POINT('Ctrl Pts',(34.9761291047989,-4.18328098024985,-10.2455804319183));
#37377=CARTESIAN_POINT('Ctrl Pts',(35.9637295000903,-4.18327789132126,-10.2455829874647));
#37378=CARTESIAN_POINT('Ctrl Pts',(37.9383590406839,-4.18327370253668,-10.2455864680815));
#37379=CARTESIAN_POINT('Ctrl Pts',(39.5833333333333,-4.18325179103929,-10.2456046429335));
#37380=CARTESIAN_POINT('Ctrl Pts',(40.9,-4.18325179103929,-10.2456046429335));
#37381=CARTESIAN_POINT('Ctrl Pts',(6.63336813585096,4.85602971916216,-13.590868440034));
#37382=CARTESIAN_POINT('Ctrl Pts',(7.389696336477,4.14888858981181,-13.8391951107513));
#37383=CARTESIAN_POINT('Ctrl Pts',(8.18053946683774,3.44401143686367,-14.0346488726453));
#37384=CARTESIAN_POINT('Ctrl Pts',(9.94201947683641,1.94757748540837,-14.3333081335907));
#37385=CARTESIAN_POINT('Ctrl Pts',(10.9113717350149,1.13915583855168,-14.4104989873604));
#37386=CARTESIAN_POINT('Ctrl Pts',(12.834739732217,-0.286629408466326,-14.4628660834126));
#37387=CARTESIAN_POINT('Ctrl Pts',(13.808142871698,-0.978270473832919,-14.422640991687));
#37388=CARTESIAN_POINT('Ctrl Pts',(15.7151185916567,-2.15221389622411,-14.3061107665235));
#37389=CARTESIAN_POINT('Ctrl Pts',(16.6852254797785,-2.70962741922243,-14.2015789338064));
#37390=CARTESIAN_POINT('Ctrl Pts',(18.5768226767694,-3.62608620812781,-14.0076819635675));
#37391=CARTESIAN_POINT('Ctrl Pts',(19.5464729449596,-4.05120533415428,-13.8818273075211));
#37392=CARTESIAN_POINT('Ctrl Pts',(20.7463406818481,-4.47793026920171,-13.7535017581768));
#37393=CARTESIAN_POINT('Ctrl Pts',(21.2156214332096,-4.63869318435443,-13.7015810566901));
#37394=CARTESIAN_POINT('Ctrl Pts',(22.1537708528638,-4.93390876526188,-13.5988388255708));
#37395=CARTESIAN_POINT('Ctrl Pts',(22.8728508922896,-5.12767073297797,-13.5262523639446));
#37396=CARTESIAN_POINT('Ctrl Pts',(23.4112391022537,-5.25280074041751,-13.4803679794399));
#37397=CARTESIAN_POINT('Ctrl Pts',(23.5274006995053,-5.27931561824263,-13.4704404449521));
#37398=CARTESIAN_POINT('Ctrl Pts',(23.7586975975699,-5.33062970711066,-13.4509289072633));
#37399=CARTESIAN_POINT('Ctrl Pts',(24.1668938536998,-5.41708560365394,-13.4171810922989));
#37400=CARTESIAN_POINT('Ctrl Pts',(24.7548128660956,-5.52956305821881,-13.3713845002051));
#37401=CARTESIAN_POINT('Ctrl Pts',(25.3473131502196,-5.6256707359588,-13.3310219589391));
#37402=CARTESIAN_POINT('Ctrl Pts',(25.821804155628,-5.6915437851135,-13.3034028562424));
#37403=CARTESIAN_POINT('Ctrl Pts',(26.0589587666351,-5.72065900880545,-13.2913640661324));
#37404=CARTESIAN_POINT('Ctrl Pts',(26.631694838376,-5.78623492045641,-13.2646759506015));
#37405=CARTESIAN_POINT('Ctrl Pts',(27.5576851463965,-5.85186367837986,-13.2364409873879));
#37406=CARTESIAN_POINT('Ctrl Pts',(28.5507795710393,-5.88219883517418,-13.221915949884));
#37407=CARTESIAN_POINT('Ctrl Pts',(29.1361849357886,-5.90128718803101,-13.2135466774644));
#37408=CARTESIAN_POINT('Ctrl Pts',(29.2912521292176,-5.90574282943919,-13.2116327381159));
#37409=CARTESIAN_POINT('Ctrl Pts',(29.6100275770337,-5.91253309751285,-13.2086893874641));
#37410=CARTESIAN_POINT('Ctrl Pts',(30.1692894984411,-5.91881362945883,-13.2059721234291));
#37411=CARTESIAN_POINT('Ctrl Pts',(31.3098805820072,-5.91428725204099,-13.2079309635128));
#37412=CARTESIAN_POINT('Ctrl Pts',(32.3163182251691,-5.8978567744948,-13.215170536538));
#37413=CARTESIAN_POINT('Ctrl Pts',(33.168669589941,-5.89783797451689,-13.2151857432769));
#37414=CARTESIAN_POINT('Ctrl Pts',(33.4952713010556,-5.89783593918776,-13.2151875891279));
#37415=CARTESIAN_POINT('Ctrl Pts',(34.1548283685117,-5.89783217350437,-13.2151907586341));
#37416=CARTESIAN_POINT('Ctrl Pts',(34.9764778638341,-5.89782019909881,-13.2152010495211));
#37417=CARTESIAN_POINT('Ctrl Pts',(35.964110112416,-5.89781516246841,-13.2152053506642));
#37418=CARTESIAN_POINT('Ctrl Pts',(37.9386244259606,-5.89780833274504,-13.2152112104218));
#37419=CARTESIAN_POINT('Ctrl Pts',(39.5833333333333,-5.89777260594516,-13.2152418049849));
#37420=CARTESIAN_POINT('Ctrl Pts',(40.9,-5.89777260594516,-13.2152418049849));
#37421=CARTESIAN_POINT('Ctrl Pts',(6.84649785567288,6.71741536412572,-21.3772113060719));
#37422=CARTESIAN_POINT('Ctrl Pts',(7.61279643984166,5.5922435141165,-21.7222003209083));
#37423=CARTESIAN_POINT('Ctrl Pts',(8.41290239278216,4.4778139915129,-21.9819683115275));
#37424=CARTESIAN_POINT('Ctrl Pts',(10.1883118359637,2.12504829883047,-22.3516942143149));
#37425=CARTESIAN_POINT('Ctrl Pts',(11.1645908932198,0.860235293933488,-22.4195115822635));
#37426=CARTESIAN_POINT('Ctrl Pts',(13.104616539894,-1.36442582505286,-22.4060524143024));
#37427=CARTESIAN_POINT('Ctrl Pts',(14.0814329274866,-2.43568052201622,-22.2982732069865));
#37428=CARTESIAN_POINT('Ctrl Pts',(15.9946796213894,-4.24582169215594,-22.0394507048972));
#37429=CARTESIAN_POINT('Ctrl Pts',(16.9653275559585,-5.10151618176832,-21.84127820419));
#37430=CARTESIAN_POINT('Ctrl Pts',(18.8448710605556,-6.49486940232066,-21.4842569534398));
#37431=CARTESIAN_POINT('Ctrl Pts',(19.8101236302159,-7.14150804350575,-21.2634255374821));
#37432=CARTESIAN_POINT('Ctrl Pts',(20.9856903475787,-7.78021164720299,-21.0426589820635));
#37433=CARTESIAN_POINT('Ctrl Pts',(21.4500377829479,-8.02347291078476,-20.9532273635235));
#37434=CARTESIAN_POINT('Ctrl Pts',(22.3710393802637,-8.46623345546778,-20.7788884454095));
#37435=CARTESIAN_POINT('Ctrl Pts',(23.071969318899,-8.75491470148117,-20.6575298272076));
#37436=CARTESIAN_POINT('Ctrl Pts',(23.5926347936585,-8.94023465873168,-20.581371981806));
#37437=CARTESIAN_POINT('Ctrl Pts',(23.7065892332643,-8.98001571960566,-20.5647099449238));
#37438=CARTESIAN_POINT('Ctrl Pts',(23.9323706520526,-9.05664995495945,-20.5321468576874));
#37439=CARTESIAN_POINT('Ctrl Pts',(24.3307466212142,-9.18574049076626,-20.475948578475));
#37440=CARTESIAN_POINT('Ctrl Pts',(24.9023508233184,-9.35309964749796,-20.4001844372315));
#37441=CARTESIAN_POINT('Ctrl Pts',(25.475797257311,-9.49555868076774,-20.333847241253));
#37442=CARTESIAN_POINT('Ctrl Pts',(25.9330914993693,-9.59288697707766,-20.2886464898199));
#37443=CARTESIAN_POINT('Ctrl Pts',(26.160978182331,-9.63581705245673,-20.2689918009897));
#37444=CARTESIAN_POINT('Ctrl Pts',(26.7099322414348,-9.73235004955931,-20.2254900271806));
#37445=CARTESIAN_POINT('Ctrl Pts',(27.5959509089717,-9.8291584788779,-20.1795241403996));
#37446=CARTESIAN_POINT('Ctrl Pts',(28.5797495606368,-9.8753206064194,-20.1552722532429));
#37447=CARTESIAN_POINT('Ctrl Pts',(29.1657855350675,-9.9044166994659,-20.1412111689924));
#37448=CARTESIAN_POINT('Ctrl Pts',(29.3146731630635,-9.91097811975316,-20.1381027603738));
#37449=CARTESIAN_POINT('Ctrl Pts',(29.6257300067641,-9.92113271524799,-20.1332492263267));
#37450=CARTESIAN_POINT('Ctrl Pts',(30.1719452394075,-9.93050366138692,-20.1287785103478));
#37451=CARTESIAN_POINT('Ctrl Pts',(31.2977811219681,-9.92376874726296,-20.131991612471));
#37452=CARTESIAN_POINT('Ctrl Pts',(32.3069259117669,-9.89857089566955,-20.1442225454145));
#37453=CARTESIAN_POINT('Ctrl Pts',(33.1709940314751,-9.89851679451548,-20.1442592438602));
#37454=CARTESIAN_POINT('Ctrl Pts',(33.4961680489759,-9.89851046735383,-20.144263738865));
#37455=CARTESIAN_POINT('Ctrl Pts',(34.1564024558334,-9.89849933968829,-20.1442714128623));
#37456=CARTESIAN_POINT('Ctrl Pts',(34.9773378017946,-9.89846345509216,-20.1442963704307));
#37457=CARTESIAN_POINT('Ctrl Pts',(35.965039526566,-9.89844842592579,-20.1443067963912));
#37458=CARTESIAN_POINT('Ctrl Pts',(37.9392783163647,-9.89842798176077,-20.1443210056783));
#37459=CARTESIAN_POINT('Ctrl Pts',(39.5833333333333,-9.89832117405886,-20.1443951831047));
#37460=CARTESIAN_POINT('Ctrl Pts',(40.9,-9.89832117405886,-20.1443951831047));
#37461=CARTESIAN_POINT('Ctrl Pts',(6.90857970435318,8.71018585725739,-29.1272609852091));
#37462=CARTESIAN_POINT('Ctrl Pts',(7.67983757144493,7.16260494418019,-29.5775536996439));
#37463=CARTESIAN_POINT('Ctrl Pts',(8.48457055999567,5.63283520142948,-29.9097225030882));
#37464=CARTESIAN_POINT('Ctrl Pts',(10.2689932185249,2.41146069737717,-30.3644487697131));
#37465=CARTESIAN_POINT('Ctrl Pts',(11.2491988139072,0.683672158318399,-30.4296414097155));
#37466=CARTESIAN_POINT('Ctrl Pts',(13.2074449203971,-2.36894751212039,-30.3576235761244));
#37467=CARTESIAN_POINT('Ctrl Pts',(14.1878085217557,-3.82665309566743,-30.1849659988379));
#37468=CARTESIAN_POINT('Ctrl Pts',(16.1228140255811,-6.30658851121944,-29.7814752498472));
#37469=CARTESIAN_POINT('Ctrl Pts',(17.0983171044691,-7.46839135174,-29.4886591763938));
#37470=CARTESIAN_POINT('Ctrl Pts',(18.9977376700381,-9.36704911481259,-28.960082872958));
#37471=CARTESIAN_POINT('Ctrl Pts',(19.9674462816336,-10.2409515663328,-28.6415548808293));
#37472=CARTESIAN_POINT('Ctrl Pts',(21.1471060032309,-11.1004135437215,-28.3239820751164));
#37473=CARTESIAN_POINT('Ctrl Pts',(21.6116736136673,-11.4272945418467,-28.1962714220823));
#37474=CARTESIAN_POINT('Ctrl Pts',(22.5321107331753,-12.020283834991,-27.9485409607958));
#37475=CARTESIAN_POINT('Ctrl Pts',(23.2282372947767,-12.4035528917693,-27.7781185470826));
#37476=CARTESIAN_POINT('Ctrl Pts',(23.7411423015334,-12.6473785079705,-27.6723004799182));
#37477=CARTESIAN_POINT('Ctrl Pts',(23.8541050059081,-12.7001926206311,-27.6489722597555));
#37478=CARTESIAN_POINT('Ctrl Pts',(24.0772792343327,-12.801532363273,-27.6035767537809));
#37479=CARTESIAN_POINT('Ctrl Pts',(24.4706231308704,-12.9720321690744,-27.5254067801745));
#37480=CARTESIAN_POINT('Ctrl Pts',(25.0326506601032,-13.1919318242547,-27.4207276483817));
#37481=CARTESIAN_POINT('Ctrl Pts',(25.592916616209,-13.3777331675808,-27.3299203180182));
#37482=CARTESIAN_POINT('Ctrl Pts',(26.0369869863338,-13.5038445845533,-27.2685418387999));
#37483=CARTESIAN_POINT('Ctrl Pts',(26.2572892845279,-13.5592118403735,-27.2420133361896));
#37484=CARTESIAN_POINT('Ctrl Pts',(26.7861809172633,-13.6833062419415,-27.1835476308026));
#37485=CARTESIAN_POINT('Ctrl Pts',(27.6340630276977,-13.8074117592231,-27.1220525704356));
#37486=CARTESIAN_POINT('Ctrl Pts',(28.6084466264573,-13.8693290201702,-27.0881176443601));
#37487=CARTESIAN_POINT('Ctrl Pts',(29.1951297895238,-13.9084309041029,-27.0683644245335));
#37488=CARTESIAN_POINT('Ctrl Pts',(29.3379067795073,-13.9168171018366,-27.0642236253565));
#37489=CARTESIAN_POINT('Ctrl Pts',(29.6412852452591,-13.9300946799831,-27.05759935462));
#37490=CARTESIAN_POINT('Ctrl Pts',(30.1744790744101,-13.9423073235084,-27.0515191755616));
#37491=CARTESIAN_POINT('Ctrl Pts',(31.2855677213348,-13.9335693345849,-27.0558675796334));
#37492=CARTESIAN_POINT('Ctrl Pts',(32.297459923672,-13.8994232817536,-27.0731946134561));
#37493=CARTESIAN_POINT('Ctrl Pts',(33.173257907635,-13.89930470752,-27.0732696672435));
#37494=CARTESIAN_POINT('Ctrl Pts',(33.4970065888604,-13.899290450687,-27.0732789151666));
#37495=CARTESIAN_POINT('Ctrl Pts',(34.1579215418454,-13.8992658208366,-27.0732946436724));
#37496=CARTESIAN_POINT('Ctrl Pts',(34.9781539333148,-13.8991859907804,-27.0733458523265));
#37497=CARTESIAN_POINT('Ctrl Pts',(35.9659297143335,-13.8991526077107,-27.0733672375488));
#37498=CARTESIAN_POINT('Ctrl Pts',(37.9398993196361,-13.8991071452309,-27.0733963900546));
#37499=CARTESIAN_POINT('Ctrl Pts',(39.5833333333333,-13.8988697421725,-27.0735485612246));
#37500=CARTESIAN_POINT('Ctrl Pts',(40.9,-13.8988697421725,-27.0735485612246));
#37501=CARTESIAN_POINT('Ctrl Pts',(6.93528330520032,9.86563481868489,-33.5512413216408));
#37502=CARTESIAN_POINT('Ctrl Pts',(7.70864561497005,8.07765806999139,-34.0623374960229));
#37503=CARTESIAN_POINT('Ctrl Pts',(8.51541871352369,6.31093086144101,-34.4367698578614));
#37504=CARTESIAN_POINT('Ctrl Pts',(10.3035747340621,2.59403255178488,-34.941954951338));
#37505=CARTESIAN_POINT('Ctrl Pts',(11.2855474597114,0.601863607331421,-35.0067705115655));
#37506=CARTESIAN_POINT('Ctrl Pts',(13.2510271399958,-2.92382891559037,-34.9032893217431));
#37507=CARTESIAN_POINT('Ctrl Pts',(14.2329608248363,-4.60257161238984,-34.6945593989858));
#37508=CARTESIAN_POINT('Ctrl Pts',(16.1768697182174,-7.46747574760142,-34.2095752766376));
#37509=CARTESIAN_POINT('Ctrl Pts',(17.1545233971705,-8.80499374792142,-33.863251175018));
#37510=CARTESIAN_POINT('Ctrl Pts',(19.0635787323924,-10.9976618314205,-33.2359528227276));
#37511=CARTESIAN_POINT('Ctrl Pts',(20.0357940514506,-12.0029926013879,-32.8613840028834));
#37512=CARTESIAN_POINT('Ctrl Pts',(21.220027374451,-12.9932317593815,-32.4867165469275));
#37513=CARTESIAN_POINT('Ctrl Pts',(21.6852779128343,-13.3687144259958,-32.3368305207216));
#37514=CARTESIAN_POINT('Ctrl Pts',(22.6074094382986,-14.0501505350056,-32.046046858365));
#37515=CARTESIAN_POINT('Ctrl Pts',(23.3034045560159,-14.48918193341,-31.8467199720654));
#37516=CARTESIAN_POINT('Ctrl Pts',(23.8143672767889,-14.7674149360665,-31.7234333079364));
#37517=CARTESIAN_POINT('Ctrl Pts',(23.9270724954073,-14.8277950271987,-31.6962311639844));
#37518=CARTESIAN_POINT('Ctrl Pts',(24.1495225469483,-14.9435144746796,-31.6433583861174));
#37519=CARTESIAN_POINT('Ctrl Pts',(24.5413305977735,-15.1380475804187,-31.5524212197085));
#37520=CARTESIAN_POINT('Ctrl Pts',(25.0999889357198,-15.3882930140602,-31.4310156375915));
#37521=CARTESIAN_POINT('Ctrl Pts',(25.6548568854791,-15.5988027583031,-31.3262265443362));
#37522=CARTESIAN_POINT('Ctrl Pts',(26.0929602492092,-15.7410876933159,-31.2557376661539));
#37523=CARTESIAN_POINT('Ctrl Pts',(26.3096479269531,-15.8033473177939,-31.2253935968529));
#37524=CARTESIAN_POINT('Ctrl Pts',(26.828712163834,-15.9425694431083,-31.1587088311852));
#37525=CARTESIAN_POINT('Ctrl Pts',(27.6557884297531,-16.0810926132799,-31.0890012981155));
#37526=CARTESIAN_POINT('Ctrl Pts',(28.6247091266679,-16.1519656805033,-31.0495586097515));
#37527=CARTESIAN_POINT('Ctrl Pts',(29.2117706203407,-16.1967753671695,-31.0265558099779));
#37528=CARTESIAN_POINT('Ctrl Pts',(29.3510921954878,-16.206115111319,-31.0218764373728));
#37529=CARTESIAN_POINT('Ctrl Pts',(29.6501043905814,-16.2210980111664,-31.0142857961678));
#37530=CARTESIAN_POINT('Ctrl Pts',(30.1758702019789,-16.2348498398373,-31.0073340046884));
#37531=CARTESIAN_POINT('Ctrl Pts',(31.2785352103419,-16.2250286703998,-31.0122942956316));
#37532=CARTESIAN_POINT('Ctrl Pts',(32.2920164760144,-16.1856975481828,-31.0325718136051));
#37533=CARTESIAN_POINT('Ctrl Pts',(33.1745232741629,-16.1855272745483,-31.0326760798737));
#37534=CARTESIAN_POINT('Ctrl Pts',(33.4974585875214,-16.1855064782318,-31.0326890056741));
#37535=CARTESIAN_POINT('Ctrl Pts',(34.1587639155489,-16.1854709093048,-31.0327109045832));
#37536=CARTESIAN_POINT('Ctrl Pts',(34.9785998474406,-16.1853552918984,-31.0327822824582));
#37537=CARTESIAN_POINT('Ctrl Pts',(35.9664200829454,-16.1853069853609,-31.0328120805001));
#37538=CARTESIAN_POINT('Ctrl Pts',(37.9402388284555,-16.1852411572709,-31.032852711537));
#37539=CARTESIAN_POINT('Ctrl Pts',(39.5833333333333,-16.1848974953804,-31.033064777293));
#37540=CARTESIAN_POINT('Ctrl Pts',(40.9,-16.1848974953804,-31.033064777293));
#37541=CARTESIAN_POINT('Origin',(6.9,-25.9807621135332,-15.));
#37542=CARTESIAN_POINT('',(6.9,-6.90555748864273,-29.194404870986));
#37543=CARTESIAN_POINT('Ctrl Pts',(6.9,-1.92623027574191,-10.8594625780007));
#37544=CARTESIAN_POINT('Ctrl Pts',(6.9,-3.00887228147899,-14.5482083700348));
#37545=CARTESIAN_POINT('Ctrl Pts',(6.90000000166257,-4.07058553003038,-18.4565659967827));
#37546=CARTESIAN_POINT('Ctrl Pts',(6.90000000166257,-5.57797815223759,-24.1072623232988));
#37547=CARTESIAN_POINT('Ctrl Pts',(6.9,-6.24902093139925,-26.6663167664834));
#37548=CARTESIAN_POINT('Ctrl Pts',(6.9,-6.90555748864273,-29.194404870986));
#37549=CARTESIAN_POINT('Origin',(6.9,0.,0.));
#37550=CARTESIAN_POINT('Origin',(40.9,-7.79422863405995,-4.5));
#37551=CARTESIAN_POINT('Ctrl Pts',(40.9,-29.0996231131986,-18.5327260452907));
#37552=CARTESIAN_POINT('Ctrl Pts',(40.9,-28.6661818974695,-18.2824786427117));
#37553=CARTESIAN_POINT('Ctrl Pts',(40.9,-28.2327406817405,-18.0322312401326));
#37554=CARTESIAN_POINT('Ctrl Pts',(40.9,-27.7992994660114,-17.7819838375536));
#37555=CARTESIAN_POINT('Ctrl Pts',(30.5,-31.061268433756,-16.1306417505986));
#37556=CARTESIAN_POINT('Ctrl Pts',(30.5,-30.7013555966443,-16.823692245373));
#37557=CARTESIAN_POINT('Ctrl Pts',(30.5,-30.3108891324554,-17.5));
#37558=CARTESIAN_POINT('Ctrl Pts',(30.5,-12.8108891324554,-47.8108891324553));
#37559=CARTESIAN_POINT('Ctrl Pts',(30.5,17.5,-30.3108891324554));
#37560=CARTESIAN_POINT('Ctrl Pts',(30.5,47.8108891324553,-12.8108891324554));
#37561=CARTESIAN_POINT('Ctrl Pts',(30.5,30.3108891324554,17.5));
#37562=CARTESIAN_POINT('Ctrl Pts',(30.5,12.8108891324554,47.8108891324553));
#37563=CARTESIAN_POINT('Ctrl Pts',(30.5,-17.5,30.3108891324554));
#37564=CARTESIAN_POINT('Ctrl Pts',(30.5,-46.4877949884694,13.5747778926489));
#37565=CARTESIAN_POINT('Ctrl Pts',(30.5,-31.061268433756,-16.1306417505986));
#37566=CARTESIAN_POINT('Ctrl Pts',(30.3311478274255,-30.9943174850025,-16.0958729911865));
#37567=CARTESIAN_POINT('Ctrl Pts',(30.3311478274255,-30.6351804212937,-16.7874296516619));
#37568=CARTESIAN_POINT('Ctrl Pts',(30.3311478274255,-30.245555587262,-17.4622796600955));
#37569=CARTESIAN_POINT('Ctrl Pts',(30.3311478274255,-12.7832759271665,-47.7078352473574));
#37570=CARTESIAN_POINT('Ctrl Pts',(30.3311478274255,17.4622796600955,-30.245555587262));
#37571=CARTESIAN_POINT('Ctrl Pts',(30.3311478274255,47.7078352473574,-12.7832759271665));
#37572=CARTESIAN_POINT('Ctrl Pts',(30.3311478274255,30.245555587262,17.4622796600955));
#37573=CARTESIAN_POINT('Ctrl Pts',(30.3311478274255,12.7832759271665,47.7078352473574));
#37574=CARTESIAN_POINT('Ctrl Pts',(30.3311478274255,-17.4622796600955,30.245555587262));
#37575=CARTESIAN_POINT('Ctrl Pts',(30.3311478274255,-46.3875929639907,13.5455181648638));
#37576=CARTESIAN_POINT('Ctrl Pts',(30.3311478274255,-30.9943174850025,-16.0958729911865));
#37577=CARTESIAN_POINT('Ctrl Pts',(29.9897712690917,-30.8587004444282,-16.0254447695752));
#37578=CARTESIAN_POINT('Ctrl Pts',(29.9897712690917,-30.501134801215,-16.7139754925467));
#37579=CARTESIAN_POINT('Ctrl Pts',(29.9897712690917,-30.1132147882992,-17.3858726641896));
#37580=CARTESIAN_POINT('Ctrl Pts',(29.9897712690917,-12.7273421241097,-47.4990874524888));
#37581=CARTESIAN_POINT('Ctrl Pts',(29.9897712690917,17.3858726641896,-30.1132147882992));
#37582=CARTESIAN_POINT('Ctrl Pts',(29.9897712690917,47.4990874524888,-12.7273421241097));
#37583=CARTESIAN_POINT('Ctrl Pts',(29.9897712690917,30.1132147882992,17.3858726641896));
#37584=CARTESIAN_POINT('Ctrl Pts',(29.9897712690917,12.7273421241097,47.4990874524888));
#37585=CARTESIAN_POINT('Ctrl Pts',(29.9897712690917,-17.3858726641896,30.1132147882992));
#37586=CARTESIAN_POINT('Ctrl Pts',(29.9897712690917,-46.1846219490559,13.4862491363571));
#37587=CARTESIAN_POINT('Ctrl Pts',(29.9897712690917,-30.8587004444282,-16.0254447695752));
#37588=CARTESIAN_POINT('Ctrl Pts',(29.4666899049319,-30.6501289206644,-15.9171300516369));
#37589=CARTESIAN_POINT('Ctrl Pts',(29.4666899049319,-30.2949800354474,-16.6010070497276));
#37590=CARTESIAN_POINT('Ctrl Pts',(29.4666899049319,-29.9096819433198,-17.2683629213518));
#37591=CARTESIAN_POINT('Ctrl Pts',(29.4666899049319,-12.6413190219681,-47.1780448646716));
#37592=CARTESIAN_POINT('Ctrl Pts',(29.4666899049319,17.2683629213518,-29.9096819433198));
#37593=CARTESIAN_POINT('Ctrl Pts',(29.4666899049319,47.1780448646716,-12.6413190219681));
#37594=CARTESIAN_POINT('Ctrl Pts',(29.4666899049319,29.9096819433198,17.2683629213518));
#37595=CARTESIAN_POINT('Ctrl Pts',(29.4666899049319,12.6413190219681,47.1780448646716));
#37596=CARTESIAN_POINT('Ctrl Pts',(29.4666899049319,-17.2683629213518,29.9096819433198));
#37597=CARTESIAN_POINT('Ctrl Pts',(29.4666899049319,-45.8724637299593,13.3950966415431));
#37598=CARTESIAN_POINT('Ctrl Pts',(29.4666899049319,-30.6501289206644,-15.9171300516369));
#37599=CARTESIAN_POINT('Ctrl Pts',(28.7471241621752,-30.3617042288049,-15.7673462336858));
#37600=CARTESIAN_POINT('Ctrl Pts',(28.7471241621752,-30.0098973754615,-16.4447877935127));
#37601=CARTESIAN_POINT('Ctrl Pts',(28.7471241621752,-29.6282250261092,-17.105863694435));
#37602=CARTESIAN_POINT('Ctrl Pts',(28.7471241621752,-12.5223613316743,-46.7340887205442));
#37603=CARTESIAN_POINT('Ctrl Pts',(28.7471241621752,17.105863694435,-29.6282250261092));
#37604=CARTESIAN_POINT('Ctrl Pts',(28.7471241621752,46.7340887205442,-12.5223613316743));
#37605=CARTESIAN_POINT('Ctrl Pts',(28.7471241621752,29.6282250261092,17.105863694435));
#37606=CARTESIAN_POINT('Ctrl Pts',(28.7471241621752,12.5223613316743,46.7340887205442));
#37607=CARTESIAN_POINT('Ctrl Pts',(28.7471241621752,-17.105863694435,29.6282250261092));
#37608=CARTESIAN_POINT('Ctrl Pts',(28.7471241621752,-45.4407934015768,13.2690457322218));
#37609=CARTESIAN_POINT('Ctrl Pts',(28.7471241621752,-30.3617042288049,-15.7673462336858));
#37610=CARTESIAN_POINT('Ctrl Pts',(27.8100958442934,-29.9846639164451,-15.5715428260696));
#37611=CARTESIAN_POINT('Ctrl Pts',(27.8100958442934,-29.6372259010587,-16.2405717231752));
#37612=CARTESIAN_POINT('Ctrl Pts',(27.8100958442934,-29.2602932679205,-16.8934381948013));
#37613=CARTESIAN_POINT('Ctrl Pts',(27.8100958442934,-12.3668550731192,-46.1537314627218));
#37614=CARTESIAN_POINT('Ctrl Pts',(27.8100958442934,16.8934381948013,-29.2602932679205));
#37615=CARTESIAN_POINT('Ctrl Pts',(27.8100958442934,46.1537314627218,-12.3668550731192));
#37616=CARTESIAN_POINT('Ctrl Pts',(27.8100958442934,29.2602932679205,16.8934381948013));
#37617=CARTESIAN_POINT('Ctrl Pts',(27.8100958442934,12.3668550731192,46.1537314627218));
#37618=CARTESIAN_POINT('Ctrl Pts',(27.8100958442934,-16.8934381948013,29.2602932679205));
#37619=CARTESIAN_POINT('Ctrl Pts',(27.8100958442934,-44.8764966543029,13.1042669335782));
#37620=CARTESIAN_POINT('Ctrl Pts',(27.8100958442934,-29.9846639164451,-15.5715428260696));
#37621=CARTESIAN_POINT('Ctrl Pts',(26.8343111708818,-29.5937642144445,-15.3685420031368));
#37622=CARTESIAN_POINT('Ctrl Pts',(26.8343111708818,-29.2508556284042,-16.0288490017));
#37623=CARTESIAN_POINT('Ctrl Pts',(26.8343111708818,-28.8788369357517,-16.6732042787395));
#37624=CARTESIAN_POINT('Ctrl Pts',(26.8343111708818,-12.2056326570122,-45.5520412144912));
#37625=CARTESIAN_POINT('Ctrl Pts',(26.8343111708818,16.6732042787395,-28.8788369357517));
#37626=CARTESIAN_POINT('Ctrl Pts',(26.8343111708818,45.5520412144912,-12.2056326570122));
#37627=CARTESIAN_POINT('Ctrl Pts',(26.8343111708818,28.8788369357517,16.6732042787395));
#37628=CARTESIAN_POINT('Ctrl Pts',(26.8343111708818,12.2056326570122,45.5520412144912));
#37629=CARTESIAN_POINT('Ctrl Pts',(26.8343111708818,-16.6732042787395,28.8788369357517));
#37630=CARTESIAN_POINT('Ctrl Pts',(26.8343111708818,-44.2914572749094,12.9334311338658));
#37631=CARTESIAN_POINT('Ctrl Pts',(26.8343111708818,-29.5937642144445,-15.3685420031368));
#37632=CARTESIAN_POINT('Ctrl Pts',(25.8181479469611,-29.1945242233064,-15.1612099270726));
#37633=CARTESIAN_POINT('Ctrl Pts',(25.8181479469611,-28.8562417071321,-15.8126089354813));
#37634=CARTESIAN_POINT('Ctrl Pts',(25.8181479469611,-28.4892417994669,-16.4482714219305));
#37635=CARTESIAN_POINT('Ctrl Pts',(25.8181479469611,-12.0409703775363,-44.9375132213974));
#37636=CARTESIAN_POINT('Ctrl Pts',(25.8181479469611,16.4482714219305,-28.4892417994669));
#37637=CARTESIAN_POINT('Ctrl Pts',(25.8181479469611,44.9375132213974,-12.0409703775363));
#37638=CARTESIAN_POINT('Ctrl Pts',(25.8181479469611,28.4892417994669,16.4482714219305));
#37639=CARTESIAN_POINT('Ctrl Pts',(25.8181479469611,12.0409703775363,44.9375132213974));
#37640=CARTESIAN_POINT('Ctrl Pts',(25.8181479469611,-16.4482714219305,28.4892417994669));
#37641=CARTESIAN_POINT('Ctrl Pts',(25.8181479469611,-43.6939354158518,12.7589503583263));
#37642=CARTESIAN_POINT('Ctrl Pts',(25.8181479469611,-29.1945242233064,-15.1612099270726));
#37643=CARTESIAN_POINT('Ctrl Pts',(24.7595197917227,-28.796912394945,-14.9547233834603));
#37644=CARTESIAN_POINT('Ctrl Pts',(24.7595197917227,-28.4632370828042,-15.5972507298839));
#37645=CARTESIAN_POINT('Ctrl Pts',(24.7595197917227,-28.1012354927406,-16.2242558762949));
#37646=CARTESIAN_POINT('Ctrl Pts',(24.7595197917227,-11.8769796164458,-44.3254913690355));
#37647=CARTESIAN_POINT('Ctrl Pts',(24.7595197917227,16.2242558762949,-28.1012354927406));
#37648=CARTESIAN_POINT('Ctrl Pts',(24.7595197917227,44.3254913690355,-11.8769796164458));
#37649=CARTESIAN_POINT('Ctrl Pts',(24.7595197917227,28.1012354927406,16.2242558762949));
#37650=CARTESIAN_POINT('Ctrl Pts',(24.7595197917227,11.8769796164458,44.3254913690355));
#37651=CARTESIAN_POINT('Ctrl Pts',(24.7595197917227,-16.2242558762949,28.1012354927406));
#37652=CARTESIAN_POINT('Ctrl Pts',(24.7595197917227,-43.0988503438666,12.5851811425261));
#37653=CARTESIAN_POINT('Ctrl Pts',(24.7595197917227,-28.796912394945,-14.9547233834603));
#37654=CARTESIAN_POINT('Ctrl Pts',(23.6563574780851,-28.4140727469455,-14.7559082828157));
#37655=CARTESIAN_POINT('Ctrl Pts',(23.6563574780851,-28.084833470769,-15.389893569599));
#37656=CARTESIAN_POINT('Ctrl Pts',(23.6563574780851,-27.7276444994825,-16.0085630157705));
#37657=CARTESIAN_POINT('Ctrl Pts',(23.6563574780851,-11.7190814837121,-43.736207515253));
#37658=CARTESIAN_POINT('Ctrl Pts',(23.6563574780851,16.0085630157705,-27.7276444994825));
#37659=CARTESIAN_POINT('Ctrl Pts',(23.6563574780851,43.736207515253,-11.7190814837121));
#37660=CARTESIAN_POINT('Ctrl Pts',(23.6563574780851,27.7276444994825,16.0085630157705));
#37661=CARTESIAN_POINT('Ctrl Pts',(23.6563574780851,11.7190814837121,43.736207515253));
#37662=CARTESIAN_POINT('Ctrl Pts',(23.6563574780851,-16.0085630157705,27.7276444994825));
#37663=CARTESIAN_POINT('Ctrl Pts',(23.6563574780851,-42.5258740306932,12.4178678468319));
#37664=CARTESIAN_POINT('Ctrl Pts',(23.6563574780851,-28.4140727469455,-14.7559082828157));
#37665=CARTESIAN_POINT('Ctrl Pts',(22.5073180101405,-28.0598057001003,-14.5719314169357));
#37666=CARTESIAN_POINT('Ctrl Pts',(22.5073180101405,-27.7346713837132,-15.1980121665098));
#37667=CARTESIAN_POINT('Ctrl Pts',(22.5073180101405,-27.3819358493961,-15.8089680335819));
#37668=CARTESIAN_POINT('Ctrl Pts',(22.5073180101405,-11.5729678158142,-43.190903882978));
#37669=CARTESIAN_POINT('Ctrl Pts',(22.5073180101405,15.8089680335819,-27.3819358493961));
#37670=CARTESIAN_POINT('Ctrl Pts',(22.5073180101405,43.190903882978,-11.5729678158142));
#37671=CARTESIAN_POINT('Ctrl Pts',(22.5073180101405,27.3819358493961,15.8089680335819));
#37672=CARTESIAN_POINT('Ctrl Pts',(22.5073180101405,11.5729678158142,43.190903882978));
#37673=CARTESIAN_POINT('Ctrl Pts',(22.5073180101405,-15.8089680335819,27.3819358493961));
#37674=CARTESIAN_POINT('Ctrl Pts',(22.5073180101405,-41.9956608528241,12.2630417010206));
#37675=CARTESIAN_POINT('Ctrl Pts',(22.5073180101405,-28.0598057001003,-14.5719314169357));
#37676=CARTESIAN_POINT('Ctrl Pts',(21.3125219557939,-27.7463544749225,-14.4091508971893));
#37677=CARTESIAN_POINT('Ctrl Pts',(21.3125219557939,-27.4248521776202,-15.0282378072439));
#37678=CARTESIAN_POINT('Ctrl Pts',(21.3125219557939,-27.0760569908086,-15.632368792237));
#37679=CARTESIAN_POINT('Ctrl Pts',(21.3125219557939,-11.4436881985716,-42.7084257830456));
#37680=CARTESIAN_POINT('Ctrl Pts',(21.3125219557939,15.632368792237,-27.0760569908086));
#37681=CARTESIAN_POINT('Ctrl Pts',(21.3125219557939,42.7084257830456,-11.4436881985716));
#37682=CARTESIAN_POINT('Ctrl Pts',(21.3125219557939,27.0760569908086,15.632368792237));
#37683=CARTESIAN_POINT('Ctrl Pts',(21.3125219557939,11.4436881985716,42.7084257830456));
#37684=CARTESIAN_POINT('Ctrl Pts',(21.3125219557939,-15.632368792237,27.0760569908086));
#37685=CARTESIAN_POINT('Ctrl Pts',(21.3125219557939,-41.5265346055806,12.1260533880339));
#37686=CARTESIAN_POINT('Ctrl Pts',(21.3125219557939,-27.7463544749225,-14.4091508971893));
#37687=CARTESIAN_POINT('Ctrl Pts',(20.0742472323676,-27.4822408172221,-14.2719922102254));
#37688=CARTESIAN_POINT('Ctrl Pts',(20.0742472323676,-27.1637988552073,-14.8851861187906));
#37689=CARTESIAN_POINT('Ctrl Pts',(20.0742472323676,-26.8183238008716,-15.4835664656477));
#37690=CARTESIAN_POINT('Ctrl Pts',(20.0742472323676,-11.3347573352238,-42.3018902665193));
#37691=CARTESIAN_POINT('Ctrl Pts',(20.0742472323676,15.4835664656477,-26.8183238008716));
#37692=CARTESIAN_POINT('Ctrl Pts',(20.0742472323676,42.3018902665193,-11.3347573352238));
#37693=CARTESIAN_POINT('Ctrl Pts',(20.0742472323676,26.8183238008716,15.4835664656477));
#37694=CARTESIAN_POINT('Ctrl Pts',(20.0742472323676,11.3347573352238,42.3018902665193));
#37695=CARTESIAN_POINT('Ctrl Pts',(20.0742472323676,-15.4835664656477,26.8183238008716));
#37696=CARTESIAN_POINT('Ctrl Pts',(20.0742472323676,-41.1312493454498,12.0106271861277));
#37697=CARTESIAN_POINT('Ctrl Pts',(20.0742472323676,-27.4822408172221,-14.2719922102254));
#37698=CARTESIAN_POINT('Ctrl Pts',(18.7979917002302,-27.2694232481814,-14.1614724492006));
#37699=CARTESIAN_POINT('Ctrl Pts',(18.7979917002302,-26.9534472438987,-14.7699178935542));
#37700=CARTESIAN_POINT('Ctrl Pts',(18.7979917002302,-26.6106474867381,-15.3636644897785));
#37701=CARTESIAN_POINT('Ctrl Pts',(18.7979917002302,-11.2469829969596,-41.9743119765166));
#37702=CARTESIAN_POINT('Ctrl Pts',(18.7979917002302,15.3636644897785,-26.6106474867381));
#37703=CARTESIAN_POINT('Ctrl Pts',(18.7979917002302,41.9743119765166,-11.2469829969596));
#37704=CARTESIAN_POINT('Ctrl Pts',(18.7979917002302,26.6106474867381,15.3636644897785));
#37705=CARTESIAN_POINT('Ctrl Pts',(18.7979917002302,11.2469829969596,41.9743119765166));
#37706=CARTESIAN_POINT('Ctrl Pts',(18.7979917002302,-15.3636644897785,26.6106474867381));
#37707=CARTESIAN_POINT('Ctrl Pts',(18.7979917002302,-40.8127362898543,11.9176190323383));
#37708=CARTESIAN_POINT('Ctrl Pts',(18.7979917002302,-27.2694232481814,-14.1614724492006));
#37709=CARTESIAN_POINT('Ctrl Pts',(17.4917404060759,-27.1042817018803,-14.0757116526895));
#37710=CARTESIAN_POINT('Ctrl Pts',(17.4917404060759,-26.7902192241678,-14.6804723978617));
#37711=CARTESIAN_POINT('Ctrl Pts',(17.4917404060759,-26.4494954361781,-15.2706233100072));
#37712=CARTESIAN_POINT('Ctrl Pts',(17.4917404060759,-11.1788721261709,-41.7201187461852));
#37713=CARTESIAN_POINT('Ctrl Pts',(17.4917404060759,15.2706233100072,-26.4494954361781));
#37714=CARTESIAN_POINT('Ctrl Pts',(17.4917404060759,41.7201187461852,-11.1788721261709));
#37715=CARTESIAN_POINT('Ctrl Pts',(17.4917404060759,26.4494954361781,15.2706233100072));
#37716=CARTESIAN_POINT('Ctrl Pts',(17.4917404060759,11.1788721261709,41.7201187461852));
#37717=CARTESIAN_POINT('Ctrl Pts',(17.4917404060759,-15.2706233100072,26.4494954361781));
#37718=CARTESIAN_POINT('Ctrl Pts',(17.4917404060759,-40.5655774732432,11.8454468408945));
#37719=CARTESIAN_POINT('Ctrl Pts',(17.4917404060759,-27.1042817018803,-14.0757116526895));
#37720=CARTESIAN_POINT('Ctrl Pts',(16.1647270995715,-26.9797204766935,-14.011024902894));
#37721=CARTESIAN_POINT('Ctrl Pts',(16.1647270995715,-26.6671013136366,-14.6130063919992));
#37722=CARTESIAN_POINT('Ctrl Pts',(16.1647270995715,-26.3279433657953,-15.2004451894511));
#37723=CARTESIAN_POINT('Ctrl Pts',(16.1647270995715,-11.1274981763442,-41.5283885552464));
#37724=CARTESIAN_POINT('Ctrl Pts',(16.1647270995715,15.2004451894511,-26.3279433657953));
#37725=CARTESIAN_POINT('Ctrl Pts',(16.1647270995715,41.5283885552464,-11.1274981763442));
#37726=CARTESIAN_POINT('Ctrl Pts',(16.1647270995715,26.3279433657953,15.2004451894511));
#37727=CARTESIAN_POINT('Ctrl Pts',(16.1647270995715,11.1274981763442,41.5283885552464));
#37728=CARTESIAN_POINT('Ctrl Pts',(16.1647270995715,-15.2004451894511,26.3279433657953));
#37729=CARTESIAN_POINT('Ctrl Pts',(16.1647270995715,-40.3791531257526,11.7910095609247));
#37730=CARTESIAN_POINT('Ctrl Pts',(16.1647270995715,-26.9797204766935,-14.011024902894));
#37731=CARTESIAN_POINT('Ctrl Pts',(14.8263876417415,-26.8868282012067,-13.9627843740029));
#37732=CARTESIAN_POINT('Ctrl Pts',(14.8263876417415,-26.5752853986496,-14.5626932163446));
#37733=CARTESIAN_POINT('Ctrl Pts',(14.8263876417415,-26.2372951854241,-15.1481094381123));
#37734=CARTESIAN_POINT('Ctrl Pts',(14.8263876417415,-11.0891857473118,-41.3854046235364));
#37735=CARTESIAN_POINT('Ctrl Pts',(14.8263876417415,15.1481094381123,-26.2372951854241));
#37736=CARTESIAN_POINT('Ctrl Pts',(14.8263876417415,41.3854046235364,-11.0891857473118));
#37737=CARTESIAN_POINT('Ctrl Pts',(14.8263876417415,26.2372951854241,15.1481094381123));
#37738=CARTESIAN_POINT('Ctrl Pts',(14.8263876417415,11.0891857473118,41.3854046235364));
#37739=CARTESIAN_POINT('Ctrl Pts',(14.8263876417415,-15.1481094381123,26.2372951854241));
#37740=CARTESIAN_POINT('Ctrl Pts',(14.8263876417415,-40.2401260583921,11.750412635195));
#37741=CARTESIAN_POINT('Ctrl Pts',(14.8263876417415,-26.8868282012067,-13.9627843740029));
#37742=CARTESIAN_POINT('Ctrl Pts',(13.4853470903953,-26.8165326442879,-13.926278703034));
#37743=CARTESIAN_POINT('Ctrl Pts',(13.4853470903953,-26.505804369746,-14.5246190849439));
#37744=CARTESIAN_POINT('Ctrl Pts',(13.4853470903953,-26.1686978312363,-15.1085047372063));
#37745=CARTESIAN_POINT('Ctrl Pts',(13.4853470903953,-11.0601930940301,-41.2772025684426));
#37746=CARTESIAN_POINT('Ctrl Pts',(13.4853470903953,15.1085047372063,-26.1686978312363));
#37747=CARTESIAN_POINT('Ctrl Pts',(13.4853470903953,41.2772025684426,-11.0601930940301));
#37748=CARTESIAN_POINT('Ctrl Pts',(13.4853470903953,26.1686978312363,15.1085047372063));
#37749=CARTESIAN_POINT('Ctrl Pts',(13.4853470903953,11.0601930940301,41.2772025684426));
#37750=CARTESIAN_POINT('Ctrl Pts',(13.4853470903953,-15.1085047372063,26.1686978312363));
#37751=CARTESIAN_POINT('Ctrl Pts',(13.4853470903953,-40.1349183317465,11.7196912055776));
#37752=CARTESIAN_POINT('Ctrl Pts',(13.4853470903953,-26.8165326442879,-13.926278703034));
#37753=CARTESIAN_POINT('Ctrl Pts',(12.1482076787549,-26.7614591013549,-13.8976780812377));
#37754=CARTESIAN_POINT('Ctrl Pts',(12.1482076787549,-26.4513689744511,-14.4947896419145));
#37755=CARTESIAN_POINT('Ctrl Pts',(12.1482076787549,-26.1149547570431,-15.0774761588537));
#37756=CARTESIAN_POINT('Ctrl Pts',(12.1482076787549,-11.0374785981894,-41.1924309158968));
#37757=CARTESIAN_POINT('Ctrl Pts',(12.1482076787549,15.0774761588537,-26.1149547570431));
#37758=CARTESIAN_POINT('Ctrl Pts',(12.1482076787549,41.1924309158968,-11.0374785981894));
#37759=CARTESIAN_POINT('Ctrl Pts',(12.1482076787549,26.1149547570431,15.0774761588537));
#37760=CARTESIAN_POINT('Ctrl Pts',(12.1482076787549,11.0374785981894,41.1924309158968));
#37761=CARTESIAN_POINT('Ctrl Pts',(12.1482076787549,-15.0774761588537,26.1149547570431));
#37762=CARTESIAN_POINT('Ctrl Pts',(12.1482076787549,-40.0524926066472,11.6956222878942));
#37763=CARTESIAN_POINT('Ctrl Pts',(12.1482076787549,-26.7614591013549,-13.8976780812377));
#37764=CARTESIAN_POINT('Ctrl Pts',(10.8190675759626,-26.716817747915,-13.8744950717886));
#37765=CARTESIAN_POINT('Ctrl Pts',(10.8190675759626,-26.4072448888814,-14.4706105780977));
#37766=CARTESIAN_POINT('Ctrl Pts',(10.8190675759626,-26.0713918511132,-15.0523251033884));
#37767=CARTESIAN_POINT('Ctrl Pts',(10.8190675759626,-11.0190667477248,-41.1237169545017));
#37768=CARTESIAN_POINT('Ctrl Pts',(10.8190675759626,15.0523251033884,-26.0713918511132));
#37769=CARTESIAN_POINT('Ctrl Pts',(10.8190675759626,41.1237169545017,-11.0190667477248));
#37770=CARTESIAN_POINT('Ctrl Pts',(10.8190675759626,26.0713918511132,15.0523251033884));
#37771=CARTESIAN_POINT('Ctrl Pts',(10.8190675759626,11.0190667477248,41.1237169545017));
#37772=CARTESIAN_POINT('Ctrl Pts',(10.8190675759626,-15.0523251033884,26.0713918511132));
#37773=CARTESIAN_POINT('Ctrl Pts',(10.8190675759626,-39.9856802003493,11.6761125740824));
#37774=CARTESIAN_POINT('Ctrl Pts',(10.8190675759626,-26.716817747915,-13.8744950717886));
#37775=CARTESIAN_POINT('Ctrl Pts',(9.50027713254189,-26.6796403391198,-13.8551882149624));
#37776=CARTESIAN_POINT('Ctrl Pts',(9.50027713254189,-26.3704982618073,-14.4504742051937));
#37777=CARTESIAN_POINT('Ctrl Pts',(9.50027713254189,-26.0351125755702,-15.0313792538877));
#37778=CARTESIAN_POINT('Ctrl Pts',(9.50027713254189,-11.0037333216826,-41.0664918294579));
#37779=CARTESIAN_POINT('Ctrl Pts',(9.50027713254189,15.0313792538877,-26.0351125755702));
#37780=CARTESIAN_POINT('Ctrl Pts',(9.5002771325419,41.0664918294579,-11.0037333216826));
#37781=CARTESIAN_POINT('Ctrl Pts',(9.5002771325419,26.0351125755702,15.0313792538877));
#37782=CARTESIAN_POINT('Ctrl Pts',(9.5002771325419,11.0037333216826,41.0664918294579));
#37783=CARTESIAN_POINT('Ctrl Pts',(9.50027713254189,-15.0313792538877,26.0351125755702));
#37784=CARTESIAN_POINT('Ctrl Pts',(9.50027713254189,-39.9300386942093,11.6598648452397));
#37785=CARTESIAN_POINT('Ctrl Pts',(9.50027713254189,-26.6796403391198,-13.8551882149624));
#37786=CARTESIAN_POINT('Ctrl Pts',(8.45435372222587,-26.6546635289318,-13.8422173352292));
#37787=CARTESIAN_POINT('Ctrl Pts',(8.45435372222587,-26.3458108626791,-14.4369460336456));
#37788=CARTESIAN_POINT('Ctrl Pts',(8.45435372222587,-26.0107391561104,-15.0173072536015));
#37789=CARTESIAN_POINT('Ctrl Pts',(8.45435372222587,-10.9934319025089,-41.0280464097118));
#37790=CARTESIAN_POINT('Ctrl Pts',(8.45435372222587,15.0173072536015,-26.0107391561104));
#37791=CARTESIAN_POINT('Ctrl Pts',(8.45435372222587,41.0280464097118,-10.9934319025089));
#37792=CARTESIAN_POINT('Ctrl Pts',(8.45435372222587,26.0107391561104,15.0173072536015));
#37793=CARTESIAN_POINT('Ctrl Pts',(8.45435372222587,10.9934319025089,41.0280464097118));
#37794=CARTESIAN_POINT('Ctrl Pts',(8.45435372222587,-15.0173072536015,26.0107391561104));
#37795=CARTESIAN_POINT('Ctrl Pts',(8.45435372222587,-39.8926571933874,11.6489491721888));
#37796=CARTESIAN_POINT('Ctrl Pts',(8.45435372222587,-26.6546635289318,-13.8422173352292));
#37797=CARTESIAN_POINT('Ctrl Pts',(7.67514864245731,-26.6383620035993,-13.8337516775665));
#37798=CARTESIAN_POINT('Ctrl Pts',(7.67514864245731,-26.3296982262274,-14.4281166503283));
#37799=CARTESIAN_POINT('Ctrl Pts',(7.67514864245731,-25.9948314436454,-15.0081229315276));
#37800=CARTESIAN_POINT('Ctrl Pts',(7.67514864245731,-10.9867085121178,-41.0029543751729));
#37801=CARTESIAN_POINT('Ctrl Pts',(7.67514864245731,15.0081229315276,-25.9948314436454));
#37802=CARTESIAN_POINT('Ctrl Pts',(7.67514864245731,41.0029543751729,-10.9867085121178));
#37803=CARTESIAN_POINT('Ctrl Pts',(7.67514864245731,25.9948314436454,15.0081229315276));
#37804=CARTESIAN_POINT('Ctrl Pts',(7.67514864245731,10.9867085121178,41.0029543751729));
#37805=CARTESIAN_POINT('Ctrl Pts',(7.67514864245731,-15.0081229315276,25.9948314436454));
#37806=CARTESIAN_POINT('Ctrl Pts',(7.67514864245731,-39.8682595430058,11.6418248789176));
#37807=CARTESIAN_POINT('Ctrl Pts',(7.67514864245731,-26.6383620035993,-13.8337516775665));
#37808=CARTESIAN_POINT('Ctrl Pts',(7.15799654185577,-26.6285708447822,-13.8286669632852));
#37809=CARTESIAN_POINT('Ctrl Pts',(7.15799654185577,-26.3200205194336,-14.4228134720947));
#37810=CARTESIAN_POINT('Ctrl Pts',(7.15799654185577,-25.9852768200144,-15.0026065670023));
#37811=CARTESIAN_POINT('Ctrl Pts',(7.15799654185577,-10.9826702530122,-40.9878833870167));
#37812=CARTESIAN_POINT('Ctrl Pts',(7.15799654185577,15.0026065670023,-25.9852768200144));
#37813=CARTESIAN_POINT('Ctrl Pts',(7.15799654185577,40.9878833870167,-10.9826702530122));
#37814=CARTESIAN_POINT('Ctrl Pts',(7.15799654185577,25.9852768200144,15.0026065670023));
#37815=CARTESIAN_POINT('Ctrl Pts',(7.15799654185577,10.9826702530122,40.9878833870167));
#37816=CARTESIAN_POINT('Ctrl Pts',(7.15799654185577,-15.0026065670023,25.9852768200144));
#37817=CARTESIAN_POINT('Ctrl Pts',(7.15799654185577,-39.8536056216838,11.6375458261629));
#37818=CARTESIAN_POINT('Ctrl Pts',(7.15799654185577,-26.6285708447822,-13.8286669632852));
#37819=CARTESIAN_POINT('Ctrl Pts',(6.9,-26.6239443717909,-13.8262643576559));
#37820=CARTESIAN_POINT('Ctrl Pts',(6.9,-26.3154476542665,-14.4203076388911));
#37821=CARTESIAN_POINT('Ctrl Pts',(6.9,-25.9807621135332,-15.));
#37822=CARTESIAN_POINT('Ctrl Pts',(6.9,-10.9807621135332,-40.9807621135331));
#37823=CARTESIAN_POINT('Ctrl Pts',(6.9,15.,-25.9807621135332));
#37824=CARTESIAN_POINT('Ctrl Pts',(6.9,40.9807621135331,-10.9807621135332));
#37825=CARTESIAN_POINT('Ctrl Pts',(6.9,25.9807621135332,15.));
#37826=CARTESIAN_POINT('Ctrl Pts',(6.9,10.9807621135332,40.9807621135331));
#37827=CARTESIAN_POINT('Ctrl Pts',(6.9,-15.,25.9807621135332));
#37828=CARTESIAN_POINT('Ctrl Pts',(6.9,-39.846681418688,11.6355239079848));
#37829=CARTESIAN_POINT('Ctrl Pts',(6.9,-26.6239443717909,-13.8262643576559));
#37830=CARTESIAN_POINT('Ctrl Pts',(6.9,-6.90555748864273,-29.194404870986));
#37831=CARTESIAN_POINT('Ctrl Pts',(7.85773098116326,-8.83308608050287,-28.7583591297181));
#37832=CARTESIAN_POINT('Ctrl Pts',(8.88781981167334,-10.6725495024415,-28.148927360677));
#37833=CARTESIAN_POINT('Ctrl Pts',(10.5914578196776,-13.4378975079049,-26.9549567714738));
#37834=CARTESIAN_POINT('Ctrl Pts',(11.2365058953701,-14.4268759573926,-26.4627511078989));
#37835=CARTESIAN_POINT('Ctrl Pts',(12.0558885382926,-15.5639851987506,-25.8276163596339));
#37836=CARTESIAN_POINT('Ctrl Pts',(12.1875764958397,-15.7427052651201,-25.7255677072203));
#37837=CARTESIAN_POINT('Ctrl Pts',(13.194901830313,-17.0880993664927,-24.9407551262718));
#37838=CARTESIAN_POINT('Ctrl Pts',(14.2258982134098,-18.4224696507577,-24.0748117650462));
#37839=CARTESIAN_POINT('Ctrl Pts',(18.2616480823244,-22.4465505568645,-20.9914735836847));
#37840=CARTESIAN_POINT('Ctrl Pts',(21.0496416709525,-24.4970863377161,-19.1084188222497));
#37841=CARTESIAN_POINT('Ctrl Pts',(25.8000196361138,-27.440416330328,-18.0798601480504));
#37842=CARTESIAN_POINT('Ctrl Pts',(26.8976561124457,-27.9949084025612,-18.1725012311874));
#37843=CARTESIAN_POINT('Ctrl Pts',(28.0045908801237,-28.5110480063609,-18.293020318403));
#37844=CARTESIAN_POINT('Ctrl Pts',(28.5235971652406,-28.7375730360626,-18.3760345677215));
#37845=CARTESIAN_POINT('Ctrl Pts',(29.0834839543824,-28.9821227669885,-18.4629109750536));
#37846=CARTESIAN_POINT('Ctrl Pts',(29.1146288039499,-28.995750541561,-18.4676985487665));
#37847=CARTESIAN_POINT('Ctrl Pts',(29.5949306848436,-29.2050975774362,-18.5426905181125));
#37848=CARTESIAN_POINT('Ctrl Pts',(30.0492939924726,-29.3870260594868,-18.6372599535756));
#37849=CARTESIAN_POINT('Ctrl Pts',(30.5,-29.559989655385,-18.7405179110273));
#37850=CARTESIAN_POINT('Ctrl Pts',(6.45331003273164,-1.59669678622779,-10.9133179225515));
#37851=CARTESIAN_POINT('Ctrl Pts',(7.20830533428676,-2.1627262104287,-10.8283039351861));
#37852=CARTESIAN_POINT('Ctrl Pts',(7.99928962140321,-2.70879554626307,-10.7080816105349));
#37853=CARTESIAN_POINT('Ctrl Pts',(9.76164489174098,-3.82718122480732,-10.3736775708918));
#37854=CARTESIAN_POINT('Ctrl Pts',(10.7316587814816,-4.40082635509405,-10.1362456656108));
#37855=CARTESIAN_POINT('Ctrl Pts',(12.6606926111663,-5.38563263712134,-9.65961205419967));
#37856=CARTESIAN_POINT('Ctrl Pts',(13.6374431259542,-5.83915384029438,-9.38360450626091));
#37857=CARTESIAN_POINT('Ctrl Pts',(14.8679539417017,-6.32358226998235,-9.06165302613707));
#37858=CARTESIAN_POINT('Ctrl Pts',(15.8146186835336,-6.68453209751778,-8.8086769516328));
#37859=CARTESIAN_POINT('Ctrl Pts',(16.7768279789012,-7.0051694125711,-8.55011854625631));
#37860=CARTESIAN_POINT('Ctrl Pts',(18.442654946101,-7.48808598435167,-8.14533972931254));
#37861=CARTESIAN_POINT('Ctrl Pts',(19.4151948753428,-7.72973898022672,-7.90738588441825));
#37862=CARTESIAN_POINT('Ctrl Pts',(20.6328868119184,-7.97443640583061,-7.66437297695772));
#37863=CARTESIAN_POINT('Ctrl Pts',(21.1054260060187,-8.06465516157007,-7.57098863237664));
#37864=CARTESIAN_POINT('Ctrl Pts',(22.0544239964408,-8.22831938421071,-7.39387592479571));
#37865=CARTESIAN_POINT('Ctrl Pts',(22.7836594350113,-8.33397294082321,-7.27389266543022));
#37866=CARTESIAN_POINT('Ctrl Pts',(23.5025637456205,-8.42426711082603,-7.17270583388456));
#37867=CARTESIAN_POINT('Ctrl Pts',(23.9756232708729,-8.47952646912222,-7.10861034193438));
#37868=CARTESIAN_POINT('Ctrl Pts',(24.5702383273712,-8.53935462310088,-7.03666681503307));
#37869=CARTESIAN_POINT('Ctrl Pts',(25.0506812637281,-8.58189400875848,-6.98463603831063));
#37870=CARTESIAN_POINT('Ctrl Pts',(25.4117237717368,-8.61093616318064,-6.94891133994702));
#37871=CARTESIAN_POINT('Ctrl Pts',(25.7132331301511,-8.63276690479097,-6.92207219011215));
#37872=CARTESIAN_POINT('Ctrl Pts',(25.924350018954,-8.64675417662544,-6.90499555217217));
#37873=CARTESIAN_POINT('Ctrl Pts',(26.0449825351307,-8.65437719289233,-6.8957416597319));
#37874=CARTESIAN_POINT('Ctrl Pts',(26.1053107047433,-8.6580646096281,-6.89128602190967));
#37875=CARTESIAN_POINT('Ctrl Pts',(26.598286881356,-8.68771831234641,-6.85557010312598));
#37876=CARTESIAN_POINT('Ctrl Pts',(27.5414448539117,-8.72222386822184,-6.81230249083088));
#37877=CARTESIAN_POINT('Ctrl Pts',(28.5384718269747,-8.7374287400485,-6.79157348079207));
#37878=CARTESIAN_POINT('Ctrl Pts',(29.1235718011012,-8.74727658763324,-6.77903979219493));
#37879=CARTESIAN_POINT('Ctrl Pts',(29.281292582401,-8.74962231400058,-6.77610142826291));
#37880=CARTESIAN_POINT('Ctrl Pts',(29.6033746665999,-8.75316560056407,-6.77163194910168));
#37881=CARTESIAN_POINT('Ctrl Pts',(30.1682156581428,-8.7564468026045,-6.76749797708626));
#37882=CARTESIAN_POINT('Ctrl Pts',(31.3151120085301,-8.75407681716344,-6.77048174742394));
#37883=CARTESIAN_POINT('Ctrl Pts',(32.320349075554,-8.74562733267079,-6.78127046660757));
#37884=CARTESIAN_POINT('Ctrl Pts',(33.1676615322708,-8.74562186943988,-6.7812835744978));
#37885=CARTESIAN_POINT('Ctrl Pts',(33.4948723279895,-8.7456213359517,-6.78128505761795));
#37886=CARTESIAN_POINT('Ctrl Pts',(34.1541357431676,-8.74562028433968,-6.78128770533521));
#37887=CARTESIAN_POINT('Ctrl Pts',(34.9760826079903,-8.74561702798979,-6.7812961259584));
#37888=CARTESIAN_POINT('Ctrl Pts',(35.9636845487692,-8.7456156797743,-6.78129958330352));
#37889=CARTESIAN_POINT('Ctrl Pts',(37.9383132355672,-8.745613828852,-6.7813043592495));
#37890=CARTESIAN_POINT('Ctrl Pts',(39.5833333333333,-8.74560464293355,-6.7813280023926));
#37891=CARTESIAN_POINT('Ctrl Pts',(40.9,-8.74560464293355,-6.7813280023926));
#37892=CARTESIAN_POINT('Ctrl Pts',(6.63336813585096,-2.58998912169034,-14.1980521881427));
#37893=CARTESIAN_POINT('Ctrl Pts',(7.389696336477,-3.32655463912722,-14.0595388287459));
#37894=CARTESIAN_POINT('Ctrl Pts',(8.18035160561764,-4.03465273479121,-13.8764440634215));
#37895=CARTESIAN_POINT('Ctrl Pts',(9.9416314386187,-5.47986851886094,-13.3869575789582));
#37896=CARTESIAN_POINT('Ctrl Pts',(10.9109664605569,-6.21859686207519,-13.0495988183286));
#37897=CARTESIAN_POINT('Ctrl Pts',(12.8334013836927,-7.47915893423736,-12.3824387994051));
#37898=CARTESIAN_POINT('Ctrl Pts',(13.8089179831182,-8.05904353786122,-12.0008911509523));
#37899=CARTESIAN_POINT('Ctrl Pts',(15.0306778911273,-8.67329495695321,-11.5604290689694));
#37900=CARTESIAN_POINT('Ctrl Pts',(15.9745670647922,-9.13243737556314,-11.2141745075895));
#37901=CARTESIAN_POINT('Ctrl Pts',(16.9295440841729,-9.53704617981305,-10.8635736365946));
#37902=CARTESIAN_POINT('Ctrl Pts',(18.5792362231986,-10.1451076803253,-10.3171018918725));
#37903=CARTESIAN_POINT('Ctrl Pts',(19.5469773926757,-10.4493242965117,-9.99640408637918));
#37904=CARTESIAN_POINT('Ctrl Pts',(20.7474295734276,-10.754900018616,-9.67172058444863));
#37905=CARTESIAN_POINT('Ctrl Pts',(21.2167794172894,-10.8681544802446,-9.54637190554476));
#37906=CARTESIAN_POINT('Ctrl Pts',(22.1549843938464,-11.0724642143303,-9.30976886072817));
#37907=CARTESIAN_POINT('Ctrl Pts',(22.8744776078266,-11.2039970972494,-9.14996578827687));
#37908=CARTESIAN_POINT('Ctrl Pts',(23.5816077902762,-11.3162019466949,-9.01558422395417));
#37909=CARTESIAN_POINT('Ctrl Pts',(24.0500749276264,-11.3851612528794,-8.9300835935143));
#37910=CARTESIAN_POINT('Ctrl Pts',(24.6365533946126,-11.4594652258083,-8.83449183240024));
#37911=CARTESIAN_POINT('Ctrl Pts',(25.1102835291688,-11.512269915973,-8.76539275960627));
#37912=CARTESIAN_POINT('Ctrl Pts',(25.4658322439329,-11.5482688417073,-8.71801358900138));
#37913=CARTESIAN_POINT('Ctrl Pts',(25.7624874136685,-11.5753180370233,-8.68244638509938));
#37914=CARTESIAN_POINT('Ctrl Pts',(25.9700349923411,-11.5926401638759,-8.65983585467432));
#37915=CARTESIAN_POINT('Ctrl Pts',(26.0885791323129,-11.6020803597253,-8.64758737376053));
#37916=CARTESIAN_POINT('Ctrl Pts',(26.1478525996404,-11.6066467500381,-8.64169115913858));
#37917=CARTESIAN_POINT('Ctrl Pts',(26.6319130667262,-11.6433645250355,-8.59444428954215));
#37918=CARTESIAN_POINT('Ctrl Pts',(27.5577774489367,-11.6860824768893,-8.53717709311581));
#37919=CARTESIAN_POINT('Ctrl Pts',(28.5508423746857,-11.7050908260002,-8.50942828058724));
#37920=CARTESIAN_POINT('Ctrl Pts',(29.1362159539423,-11.7174369518246,-8.49263545125893));
#37921=CARTESIAN_POINT('Ctrl Pts',(29.2912819508841,-11.7203386713976,-8.48875007883417));
#37922=CARTESIAN_POINT('Ctrl Pts',(29.610052998187,-11.7247475094471,-8.4828058172773));
#37923=CARTESIAN_POINT('Ctrl Pts',(30.1693026775047,-11.728827902791,-8.47731190452095));
#37924=CARTESIAN_POINT('Ctrl Pts',(31.3098786008463,-11.7258872894481,-8.48127083805332));
#37925=CARTESIAN_POINT('Ctrl Pts',(32.3162827048883,-11.7152777874898,-8.49575357359988));
#37926=CARTESIAN_POINT('Ctrl Pts',(33.1686195735696,-11.715269078277,-8.49577523975602));
#37927=CARTESIAN_POINT('Ctrl Pts',(33.4952188807558,-11.7152682401723,-8.49577770055113));
#37928=CARTESIAN_POINT('Ctrl Pts',(34.1547734244042,-11.7152665713231,-8.49578208271196));
#37929=CARTESIAN_POINT('Ctrl Pts',(34.9764178792931,-11.7152614171757,-8.49579602915745));
#37930=CARTESIAN_POINT('Ctrl Pts',(35.9640520550922,-11.7152592814565,-8.49580175406155));
#37931=CARTESIAN_POINT('Ctrl Pts',(37.9385651163988,-11.7152563511877,-8.49580966365999));
#37932=CARTESIAN_POINT('Ctrl Pts',(39.5833333333333,-11.7152418049849,-8.49584881729847));
#37933=CARTESIAN_POINT('Ctrl Pts',(40.9,-11.7152418049849,-8.49584881729847));
#37934=CARTESIAN_POINT('Ctrl Pts',(6.84648239176542,-4.87117200494631,-21.8719108775553));
#37935=CARTESIAN_POINT('Ctrl Pts',(7.61278097593421,-6.01809391809558,-21.6080942034255));
#37936=CARTESIAN_POINT('Ctrl Pts',(8.41274152921386,-7.11297694015339,-21.2759544371052));
#37937=CARTESIAN_POINT('Ctrl Pts',(10.1879716557546,-9.3352659896486,-20.4198986989574));
#37938=CARTESIAN_POINT('Ctrl Pts',(11.1642573475929,-10.4645258845954,-19.8462357742843));
#37939=CARTESIAN_POINT('Ctrl Pts',(13.1034321172788,-12.3837514736036,-18.7228640453274));
#37940=CARTESIAN_POINT('Ctrl Pts',(14.0822646095709,-13.259092905625,-18.0925354910949));
#37941=CARTESIAN_POINT('Ctrl Pts',(15.3084001581866,-14.1807147676625,-17.369341405527));
#37942=CARTESIAN_POINT('Ctrl Pts',(16.2531227144981,-14.8695159890908,-16.8032299545452));
#37943=CARTESIAN_POINT('Ctrl Pts',(17.2084375604977,-15.4708786153412,-16.2348330754283));
#37944=CARTESIAN_POINT('Ctrl Pts',(18.8473961588578,-16.3684102669437,-15.3570672461537));
#37945=CARTESIAN_POINT('Ctrl Pts',(19.8110405035781,-16.8164458459158,-14.8437940564497));
#37946=CARTESIAN_POINT('Ctrl Pts',(20.987265500616,-17.2594998647323,-14.3329359049566));
#37947=CARTESIAN_POINT('Ctrl Pts',(21.4517346237734,-17.4254488483261,-14.1338378277511));
#37948=CARTESIAN_POINT('Ctrl Pts',(22.3727984841464,-17.72174912934,-13.7614448137587));
#37949=CARTESIAN_POINT('Ctrl Pts',(23.074354337756,-17.9111527143534,-13.5118529399621));
#37950=CARTESIAN_POINT('Ctrl Pts',(23.7582742987063,-18.0719640430561,-13.3034745440379));
#37951=CARTESIAN_POINT('Ctrl Pts',(24.2174386855894,-18.1719103336477,-13.1693266480666));
#37952=CARTESIAN_POINT('Ctrl Pts',(24.7870213943587,-18.2785218143408,-13.020703786838));
#37953=CARTESIAN_POINT('Ctrl Pts',(25.2463470121634,-18.3542161979472,-12.9133861579982));
#37954=CARTESIAN_POINT('Ctrl Pts',(25.5899787396419,-18.4056632423986,-12.8400372670538));
#37955=CARTESIAN_POINT('Ctrl Pts',(25.8759048428224,-18.444266017472,-12.7850917865304));
#37956=CARTESIAN_POINT('Ctrl Pts',(26.0755068065029,-18.4689567859641,-12.7502361709813));
#37957=CARTESIAN_POINT('Ctrl Pts',(26.1893780149128,-18.4824083304412,-12.7313725692328));
#37958=CARTESIAN_POINT('Ctrl Pts',(26.2462863876019,-18.4889145361419,-12.7222969574594));
#37959=CARTESIAN_POINT('Ctrl Pts',(26.7102722067271,-18.5411896593429,-12.6496548741737));
#37960=CARTESIAN_POINT('Ctrl Pts',(27.5960905386886,-18.6020458648121,-12.5614420302555));
#37961=CARTESIAN_POINT('Ctrl Pts',(28.5798438027286,-18.629899960324,-12.5173520665108));
#37962=CARTESIAN_POINT('Ctrl Pts',(29.1658297917577,-18.6480680632814,-12.4906249890439));
#37963=CARTESIAN_POINT('Ctrl Pts',(29.3147155528138,-18.6521962493032,-12.4846522276656));
#37964=CARTESIAN_POINT('Ctrl Pts',(29.6257654938391,-18.6585637397073,-12.4753713397182));
#37965=CARTESIAN_POINT('Ctrl Pts',(30.1719616098277,-18.6644443298454,-12.4668129248999));
#37966=CARTESIAN_POINT('Ctrl Pts',(31.2977738410334,-18.6602190141086,-12.472961188488));
#37967=CARTESIAN_POINT('Ctrl Pts',(32.3068669150108,-18.6445149503826,-12.4961463862896));
#37968=CARTESIAN_POINT('Ctrl Pts',(33.1709127040733,-18.6444874715365,-12.4962026881972));
#37969=CARTESIAN_POINT('Ctrl Pts',(33.4960830255433,-18.644484418038,-12.4962093123004));
#37970=CARTESIAN_POINT('Ctrl Pts',(34.1563135822162,-18.6444789016084,-12.4962208405723));
#37971=CARTESIAN_POINT('Ctrl Pts',(34.9772414248898,-18.6444614154564,-12.4962577684095));
#37972=CARTESIAN_POINT('Ctrl Pts',(35.964946372113,-18.6444542286038,-12.496272896639));
#37973=CARTESIAN_POINT('Ctrl Pts',(37.9391834323222,-18.6444443083029,-12.4962938290756));
#37974=CARTESIAN_POINT('Ctrl Pts',(39.5833333333333,-18.6443951831047,-12.4963973854122));
#37975=CARTESIAN_POINT('Ctrl Pts',(40.9,-18.6443951831047,-12.4963973854122));
#37976=CARTESIAN_POINT('Ctrl Pts',(6.90857970435318,-7.02038826853569,-29.5800408844791));
#37977=CARTESIAN_POINT('Ctrl Pts',(7.67983757144493,-8.58577901088989,-29.1962153577801));
#37978=CARTESIAN_POINT('Ctrl Pts',(8.4844629659692,-10.0765485557758,-28.7191114013952));
#37979=CARTESIAN_POINT('Ctrl Pts',(10.2687526859613,-13.0935628879538,-27.5023711977385));
#37980=CARTESIAN_POINT('Ctrl Pts',(11.2489627292759,-14.6224501564806,-26.6949552438923));
#37981=CARTESIAN_POINT('Ctrl Pts',(13.2065810728343,-17.2294066625499,-25.1069038454382));
#37982=CARTESIAN_POINT('Ctrl Pts',(14.188432579866,-18.4069952853951,-24.2271697832519));
#37983=CARTESIAN_POINT('Ctrl Pts',(15.4296983589676,-19.6550892131211,-23.2080338536349));
#37984=CARTESIAN_POINT('Ctrl Pts',(16.3788042670986,-20.5796860932724,-22.4189011948389));
#37985=CARTESIAN_POINT('Ctrl Pts',(17.3450159165718,-21.3903231452907,-21.6217224592711));
#37986=CARTESIAN_POINT('Ctrl Pts',(18.9999962645462,-22.5937460627634,-20.3951481814249));
#37987=CARTESIAN_POINT('Ctrl Pts',(19.9686658165165,-23.1898054127389,-19.6835411202358));
#37988=CARTESIAN_POINT('Ctrl Pts',(21.1489437168841,-23.7756910485749,-18.9783964629487));
#37989=CARTESIAN_POINT('Ctrl Pts',(21.6136662410167,-23.9949385633152,-18.7043064424585));
#37990=CARTESIAN_POINT('Ctrl Pts',(22.5341605437882,-24.3846521737583,-18.1932305660766));
#37991=CARTESIAN_POINT('Ctrl Pts',(23.2310352415763,-24.631517887271,-17.8537326154787));
#37992=CARTESIAN_POINT('Ctrl Pts',(23.904768062761,-24.8394315921367,-17.5731511638352));
#37993=CARTESIAN_POINT('Ctrl Pts',(24.3593217251593,-24.9695871891301,-17.3912549800691));
#37994=CARTESIAN_POINT('Ctrl Pts',(24.9191284505008,-25.1069751863358,-17.1917285847407));
#37995=CARTESIAN_POINT('Ctrl Pts',(25.3687829483026,-25.2041659752935,-17.0482631873592));
#37996=CARTESIAN_POINT('Ctrl Pts',(25.703880946624,-25.269917189492,-16.9507036504243));
#37997=CARTESIAN_POINT('Ctrl Pts',(25.981527527538,-25.3190677310923,-16.8779731233104));
#37998=CARTESIAN_POINT('Ctrl Pts',(26.1747255747308,-25.3504124116977,-16.832023377701));
#37999=CARTESIAN_POINT('Ctrl Pts',(26.2847430019941,-25.3674660195527,-16.8072090098453));
#38000=CARTESIAN_POINT('Ctrl Pts',(26.3396756125252,-25.3757090167854,-16.7952849898385));
#38001=CARTESIAN_POINT('Ctrl Pts',(26.7867185605548,-25.4418392909474,-16.7000344271697));
#38002=CARTESIAN_POINT('Ctrl Pts',(27.6343089133551,-25.5185659559043,-16.5847364280863));
#38003=CARTESIAN_POINT('Ctrl Pts',(28.6086204191331,-25.5552242576154,-16.5243820587323));
#38004=CARTESIAN_POINT('Ctrl Pts',(29.1952293795949,-25.5792110357046,-16.4877244301025));
#38005=CARTESIAN_POINT('Ctrl Pts',(29.3380035933319,-25.584403327273,-16.4799452423709));
#38006=CARTESIAN_POINT('Ctrl Pts',(29.6413717635321,-25.5925899885791,-16.4675695714433));
#38007=CARTESIAN_POINT('Ctrl Pts',(30.174536806517,-25.6001268754995,-16.4561967872262));
#38008=CARTESIAN_POINT('Ctrl Pts',(31.2855894033322,-25.5947346655064,-16.464330041984));
#38009=CARTESIAN_POINT('Ctrl Pts',(32.2974015084455,-25.5738307704501,-16.4964013295029));
#38010=CARTESIAN_POINT('Ctrl Pts',(33.1731651112182,-25.5737672879574,-16.4965224425527));
#38011=CARTESIAN_POINT('Ctrl Pts',(33.4969081472871,-25.57375987162,-16.4965369996129));
#38012=CARTESIAN_POINT('Ctrl Pts',(34.1578169391039,-25.5737469053194,-16.4965619872358));
#38013=CARTESIAN_POINT('Ctrl Pts',(34.9780359591179,-25.5737054251286,-16.496642344611));
#38014=CARTESIAN_POINT('Ctrl Pts',(35.9658147840134,-25.5736884251095,-16.4966752246752));
#38015=CARTESIAN_POINT('Ctrl Pts',(37.9397802282712,-25.5736649097449,-16.4967207607426));
#38016=CARTESIAN_POINT('Ctrl Pts',(39.5833333333333,-25.5735485612246,-16.4969459535258));
#38017=CARTESIAN_POINT('Ctrl Pts',(40.9,-25.5735485612246,-16.4969459535258));
#38018=CARTESIAN_POINT('Ctrl Pts',(6.93528330520032,-8.231730283379,-33.9890447223856));
#38019=CARTESIAN_POINT('Ctrl Pts',(7.70864561497005,-10.0357116563145,-33.5376786188307));
#38020=CARTESIAN_POINT('Ctrl Pts',(8.51532719250786,-11.7528338486872,-32.9786927413523));
#38021=CARTESIAN_POINT('Ctrl Pts',(10.3033707684643,-15.2242195800702,-31.5578840442132));
#38022=CARTESIAN_POINT('Ctrl Pts',(11.285359425586,-16.9818886494149,-30.6179424293771));
#38023=CARTESIAN_POINT('Ctrl Pts',(13.2503075123955,-19.9828238609275,-28.7660858779662));
#38024=CARTESIAN_POINT('Ctrl Pts',(14.2335802328307,-21.333808720003,-27.744590382611));
#38025=CARTESIAN_POINT('Ctrl Pts',(15.4809874764708,-22.7701484639683,-26.5562215055806));
#38026=CARTESIAN_POINT('Ctrl Pts',(16.4318967140332,-23.8303538982284,-25.6398645222147));
#38027=CARTESIAN_POINT('Ctrl Pts',(17.4027860882061,-24.7620955812504,-24.7114068344531));
#38028=CARTESIAN_POINT('Ctrl Pts',(19.0657008739464,-26.1438767914272,-23.2827894621994));
#38029=CARTESIAN_POINT('Ctrl Pts',(20.0370987955263,-26.8257745442827,-22.4568785783624));
#38030=CARTESIAN_POINT('Ctrl Pts',(21.2219373681819,-27.4963832022122,-21.6368752952081));
#38031=CARTESIAN_POINT('Ctrl Pts',(21.6873545199147,-27.7466423667127,-21.3192655757679));
#38032=CARTESIAN_POINT('Ctrl Pts',(22.6095407883916,-28.1914275999318,-20.7266792263566));
#38033=CARTESIAN_POINT('Ctrl Pts',(23.306319546872,-28.4721721598033,-20.33420635525));
#38034=CARTESIAN_POINT('Ctrl Pts',(23.97749158379,-28.7077527668379,-20.0111563083465));
#38035=CARTESIAN_POINT('Ctrl Pts',(24.4307021142574,-28.8553793495036,-19.8016082531842));
#38036=CARTESIAN_POINT('Ctrl Pts',(24.9871188326861,-29.0105626137836,-19.5726095610119));
#38037=CARTESIAN_POINT('Ctrl Pts',(25.4329141726814,-29.1200357132464,-19.4084486444522));
#38038=CARTESIAN_POINT('Ctrl Pts',(25.7643950554697,-29.1939083663023,-19.2971155191107));
#38039=CARTESIAN_POINT('Ctrl Pts',(26.0382972138575,-29.2489718106938,-19.2143910494173));
#38040=CARTESIAN_POINT('Ctrl Pts',(26.2284820979133,-29.2840172105126,-19.1622606931669));
#38041=CARTESIAN_POINT('Ctrl Pts',(26.336649445506,-29.3030632173394,-19.1341507449285));
#38042=CARTESIAN_POINT('Ctrl Pts',(26.3906225284364,-29.3122642693063,-19.1206543727096));
#38043=CARTESIAN_POINT('Ctrl Pts',(26.8293654116031,-29.3859982106889,-19.012988583459));
#38044=CARTESIAN_POINT('Ctrl Pts',(27.6560988760144,-29.4710985842865,-18.8833816200193));
#38045=CARTESIAN_POINT('Ctrl Pts',(28.6249317030318,-29.5127595133997,-18.8137794716615));
#38046=CARTESIAN_POINT('Ctrl Pts',(29.2119052185273,-29.5400636810177,-18.7714558506415));
#38047=CARTESIAN_POINT('Ctrl Pts',(29.351223493954,-29.5458124634024,-18.7627335234215));
#38048=CARTESIAN_POINT('Ctrl Pts',(29.6502234545151,-29.5549926880432,-18.7486685476099));
#38049=CARTESIAN_POINT('Ctrl Pts',(30.1759548990665,-29.5634265890421,-18.7357718416966));
#38050=CARTESIAN_POINT('Ctrl Pts',(31.2785766862301,-29.5574021311857,-18.7449771625331));
#38051=CARTESIAN_POINT('Ctrl Pts',(32.2919610610309,-29.5334837411524,-18.7821959068194));
#38052=CARTESIAN_POINT('Ctrl Pts',(33.1744263360525,-29.533390407254,-18.7823679845324));
#38053=CARTESIAN_POINT('Ctrl Pts',(33.4973548461808,-29.5333792377698,-18.7823889294252));
#38054=CARTESIAN_POINT('Ctrl Pts',(34.1586526208335,-29.5333600113094,-18.7824245927187));
#38055=CARTESIAN_POINT('Ctrl Pts',(34.978471543808,-29.5332982308031,-18.7825395490483));
#38056=CARTESIAN_POINT('Ctrl Pts',(35.9662945600334,-29.5332729456428,-18.782586552422));
#38057=CARTESIAN_POINT('Ctrl Pts',(37.9401075800399,-29.533237934286,-18.7826516826344));
#38058=CARTESIAN_POINT('Ctrl Pts',(39.5833333333333,-29.533064777293,-18.7829737067337));
#38059=CARTESIAN_POINT('Ctrl Pts',(40.9,-29.533064777293,-18.7829737067337));
#38060=CARTESIAN_POINT('Origin',(6.9,-30.,3.67394039744206E-15));
#38061=CARTESIAN_POINT('',(6.9,-20.5775906479515,-21.8303175223207));
#38062=CARTESIAN_POINT('Ctrl Pts',(6.9,-7.09789564133157,-8.44145532612415));
#38063=CARTESIAN_POINT('Ctrl Pts',(6.9,-9.87986401752105,-11.09468188726));
#38064=CARTESIAN_POINT('Ctrl Pts',(6.90000000166257,-12.753513475675,-13.9485622548227));
#38065=CARTESIAN_POINT('Ctrl Pts',(6.90000000166257,-16.8843019432417,-18.0885125115534));
#38066=CARTESIAN_POINT('Ctrl Pts',(6.9,-18.7449692586141,-19.9691972794379));
#38067=CARTESIAN_POINT('Ctrl Pts',(6.9,-20.5775906479515,-21.8303175223207));
#38068=CARTESIAN_POINT('Origin',(6.9,0.,0.));
#38069=CARTESIAN_POINT('Origin',(40.9,-9.,1.10218211923262E-15));
#38070=CARTESIAN_POINT('Ctrl Pts',(40.9,-34.4673758792282,-1.5));
#38071=CARTESIAN_POINT('Ctrl Pts',(40.9,-33.9668810740701,-1.5));
#38072=CARTESIAN_POINT('Ctrl Pts',(40.9,-33.466386268912,-1.5));
#38073=CARTESIAN_POINT('Ctrl Pts',(40.9,-32.9658914637539,-1.5));
#38074=CARTESIAN_POINT('Ctrl Pts',(30.5,-34.9651684126997,1.56108868151375));
#38075=CARTESIAN_POINT('Ctrl Pts',(30.5,-35.,0.780932928377884));
#38076=CARTESIAN_POINT('Ctrl Pts',(30.5,-35.,4.28626379701574E-15));
#38077=CARTESIAN_POINT('Ctrl Pts',(30.5,-35.,-35.));
#38078=CARTESIAN_POINT('Ctrl Pts',(30.5,-4.28626379701574E-15,-35.));
#38079=CARTESIAN_POINT('Ctrl Pts',(30.5,35.,-35.));
#38080=CARTESIAN_POINT('Ctrl Pts',(30.5,35.,-4.28626379701574E-15));
#38081=CARTESIAN_POINT('Ctrl Pts',(30.5,35.,35.));
#38082=CARTESIAN_POINT('Ctrl Pts',(30.5,4.28626379701574E-15,35.));
#38083=CARTESIAN_POINT('Ctrl Pts',(30.5,-33.472222479613,35.));
#38084=CARTESIAN_POINT('Ctrl Pts',(30.5,-34.9651684126997,1.56108868151375));
#38085=CARTESIAN_POINT('Ctrl Pts',(30.3311478274255,-34.8898028105656,1.55772383604588));
#38086=CARTESIAN_POINT('Ctrl Pts',(30.3311478274255,-34.924559320191,0.779249668063539));
#38087=CARTESIAN_POINT('Ctrl Pts',(30.3311478274255,-34.924559320191,4.27702497831037E-15));
#38088=CARTESIAN_POINT('Ctrl Pts',(30.3311478274255,-34.924559320191,-34.924559320191));
#38089=CARTESIAN_POINT('Ctrl Pts',(30.3311478274255,-4.27702497831037E-15,
-34.924559320191));
#38090=CARTESIAN_POINT('Ctrl Pts',(30.3311478274255,34.924559320191,-34.924559320191));
#38091=CARTESIAN_POINT('Ctrl Pts',(30.3311478274255,34.924559320191,-4.27702497831037E-15));
#38092=CARTESIAN_POINT('Ctrl Pts',(30.3311478274255,34.924559320191,34.924559320191));
#38093=CARTESIAN_POINT('Ctrl Pts',(30.3311478274255,4.27702497831037E-15,
34.924559320191));
#38094=CARTESIAN_POINT('Ctrl Pts',(30.3311478274255,-33.4000748447964,34.924559320191));
#38095=CARTESIAN_POINT('Ctrl Pts',(30.3311478274255,-34.8898028105656,1.55772383604588));
#38096=CARTESIAN_POINT('Ctrl Pts',(29.9897712690917,-34.7371408974366,1.55090794481747));
#38097=CARTESIAN_POINT('Ctrl Pts',(29.9897712690917,-34.7717453283792,0.775840025831461));
#38098=CARTESIAN_POINT('Ctrl Pts',(29.9897712690917,-34.7717453283792,4.25831066171665E-15));
#38099=CARTESIAN_POINT('Ctrl Pts',(29.9897712690917,-34.7717453283791,-34.7717453283791));
#38100=CARTESIAN_POINT('Ctrl Pts',(29.9897712690917,-4.25831066171665E-15,
-34.7717453283792));
#38101=CARTESIAN_POINT('Ctrl Pts',(29.9897712690917,34.7717453283791,-34.7717453283791));
#38102=CARTESIAN_POINT('Ctrl Pts',(29.9897712690917,34.7717453283792,-4.25831066171665E-15));
#38103=CARTESIAN_POINT('Ctrl Pts',(29.9897712690917,34.7717453283791,34.7717453283791));
#38104=CARTESIAN_POINT('Ctrl Pts',(29.9897712690917,4.25831066171665E-15,
34.7717453283792));
#38105=CARTESIAN_POINT('Ctrl Pts',(29.9897712690917,-33.2539313038843,34.7717453283791));
#38106=CARTESIAN_POINT('Ctrl Pts',(29.9897712690917,-34.7371408974366,1.55090794481747));
#38107=CARTESIAN_POINT('Ctrl Pts',(29.4666899049319,-34.5023553003819,1.54042548027394));
#38108=CARTESIAN_POINT('Ctrl Pts',(29.4666899049319,-34.5367258427036,0.770596184255047));
#38109=CARTESIAN_POINT('Ctrl Pts',(29.4666899049319,-34.5367258427036,4.22952907562966E-15));
#38110=CARTESIAN_POINT('Ctrl Pts',(29.4666899049319,-34.5367258427036,-34.5367258427036));
#38111=CARTESIAN_POINT('Ctrl Pts',(29.4666899049319,-4.22952907562966E-15,
-34.5367258427036));
#38112=CARTESIAN_POINT('Ctrl Pts',(29.4666899049319,34.5367258427036,-34.5367258427036));
#38113=CARTESIAN_POINT('Ctrl Pts',(29.4666899049319,34.5367258427036,-4.22952907562966E-15));
#38114=CARTESIAN_POINT('Ctrl Pts',(29.4666899049319,34.5367258427036,34.5367258427036));
#38115=CARTESIAN_POINT('Ctrl Pts',(29.4666899049319,4.22952907562966E-15,
34.5367258427036));
#38116=CARTESIAN_POINT('Ctrl Pts',(29.4666899049319,-33.0291706035535,34.5367258427036));
#38117=CARTESIAN_POINT('Ctrl Pts',(29.4666899049319,-34.5023553003819,1.54042548027394));
#38118=CARTESIAN_POINT('Ctrl Pts',(28.7471241621752,-34.1776802811774,1.52592972576568));
#38119=CARTESIAN_POINT('Ctrl Pts',(28.7471241621752,-34.21172738887,0.763344698704459));
#38120=CARTESIAN_POINT('Ctrl Pts',(28.7471241621752,-34.21172738887,4.18972824400814E-15));
#38121=CARTESIAN_POINT('Ctrl Pts',(28.7471241621752,-34.2117273888699,-34.2117273888699));
#38122=CARTESIAN_POINT('Ctrl Pts',(28.7471241621752,-4.18972824400814E-15,
-34.21172738887));
#38123=CARTESIAN_POINT('Ctrl Pts',(28.7471241621752,34.2117273888699,-34.2117273888699));
#38124=CARTESIAN_POINT('Ctrl Pts',(28.7471241621752,34.21172738887,-4.18972824400814E-15));
#38125=CARTESIAN_POINT('Ctrl Pts',(28.7471241621752,34.2117273888699,34.2117273888699));
#38126=CARTESIAN_POINT('Ctrl Pts',(28.7471241621752,4.18972824400814E-15,
34.21172738887));
#38127=CARTESIAN_POINT('Ctrl Pts',(28.7471241621752,-32.718358587775,34.2117273888699));
#38128=CARTESIAN_POINT('Ctrl Pts',(28.7471241621752,-34.1776802811774,1.52592972576568));
#38129=CARTESIAN_POINT('Ctrl Pts',(27.8100958442934,-33.7532520886149,1.50698029472894));
#38130=CARTESIAN_POINT('Ctrl Pts',(27.8100958442934,-33.7868763896026,0.753865266276398));
#38131=CARTESIAN_POINT('Ctrl Pts',(27.8100958442934,-33.7868763896026,4.13769900237141E-15));
#38132=CARTESIAN_POINT('Ctrl Pts',(27.8100958442934,-33.7868763896026,-33.7868763896026));
#38133=CARTESIAN_POINT('Ctrl Pts',(27.8100958442934,-4.13769900237141E-15,
-33.7868763896026));
#38134=CARTESIAN_POINT('Ctrl Pts',(27.8100958442934,33.7868763896026,-33.7868763896026));
#38135=CARTESIAN_POINT('Ctrl Pts',(27.8100958442934,33.7868763896026,-4.13769900237141E-15));
#38136=CARTESIAN_POINT('Ctrl Pts',(27.8100958442934,33.7868763896026,33.7868763896026));
#38137=CARTESIAN_POINT('Ctrl Pts',(27.8100958442934,4.13769900237141E-15,
33.7868763896026));
#38138=CARTESIAN_POINT('Ctrl Pts',(27.8100958442934,-32.3120526686846,33.7868763896026));
#38139=CARTESIAN_POINT('Ctrl Pts',(27.8100958442934,-33.7532520886149,1.50698029472894));
#38140=CARTESIAN_POINT('Ctrl Pts',(26.8343111708818,-33.3132226048841,1.48733431337754));
#38141=CARTESIAN_POINT('Ctrl Pts',(26.8343111708818,-33.3464085574791,0.74403738530507));
#38142=CARTESIAN_POINT('Ctrl Pts',(26.8343111708818,-33.3464085574791,4.08375725029767E-15));
#38143=CARTESIAN_POINT('Ctrl Pts',(26.8343111708818,-33.3464085574791,-33.3464085574791));
#38144=CARTESIAN_POINT('Ctrl Pts',(26.8343111708818,-4.08375725029767E-15,
-33.3464085574791));
#38145=CARTESIAN_POINT('Ctrl Pts',(26.8343111708818,33.3464085574791,-33.3464085574791));
#38146=CARTESIAN_POINT('Ctrl Pts',(26.8343111708818,33.3464085574791,-4.08375725029767E-15));
#38147=CARTESIAN_POINT('Ctrl Pts',(26.8343111708818,33.3464085574791,33.3464085574791));
#38148=CARTESIAN_POINT('Ctrl Pts',(26.8343111708818,4.08375725029767E-15,
33.3464085574791));
#38149=CARTESIAN_POINT('Ctrl Pts',(26.8343111708818,-31.8908116037717,33.3464085574791));
#38150=CARTESIAN_POINT('Ctrl Pts',(26.8343111708818,-33.3132226048841,1.48733431337754));
#38151=CARTESIAN_POINT('Ctrl Pts',(25.8181479469611,-32.8638045923198,1.46726916269953));
#38152=CARTESIAN_POINT('Ctrl Pts',(25.8181479469611,-32.8965428438611,0.733999815330427));
#38153=CARTESIAN_POINT('Ctrl Pts',(25.8181479469611,-32.8965428438611,4.02866458967482E-15));
#38154=CARTESIAN_POINT('Ctrl Pts',(25.8181479469611,-32.896542843861,-32.896542843861));
#38155=CARTESIAN_POINT('Ctrl Pts',(25.8181479469611,-4.02866458967482E-15,
-32.8965428438611));
#38156=CARTESIAN_POINT('Ctrl Pts',(25.8181479469611,32.896542843861,-32.896542843861));
#38157=CARTESIAN_POINT('Ctrl Pts',(25.8181479469611,32.8965428438611,-4.02866458967482E-15));
#38158=CARTESIAN_POINT('Ctrl Pts',(25.8181479469611,32.896542843861,32.896542843861));
#38159=CARTESIAN_POINT('Ctrl Pts',(25.8181479469611,4.02866458967482E-15,
32.8965428438611));
#38160=CARTESIAN_POINT('Ctrl Pts',(25.8181479469611,-31.4605828822811,32.896542843861));
#38161=CARTESIAN_POINT('Ctrl Pts',(25.8181479469611,-32.8638045923198,1.46726916269953));
#38162=CARTESIAN_POINT('Ctrl Pts',(24.7595197917227,-32.4162193763075,1.44728584082668));
#38163=CARTESIAN_POINT('Ctrl Pts',(24.7595197917227,-32.4485117525897,0.724003180127259));
#38164=CARTESIAN_POINT('Ctrl Pts',(24.7595197917227,-32.4485117525897,3.97379660549043E-15));
#38165=CARTESIAN_POINT('Ctrl Pts',(24.7595197917227,-32.4485117525897,-32.4485117525897));
#38166=CARTESIAN_POINT('Ctrl Pts',(24.7595197917227,-3.97379660549043E-15,
-32.4485117525897));
#38167=CARTESIAN_POINT('Ctrl Pts',(24.7595197917227,32.4485117525897,-32.4485117525897));
#38168=CARTESIAN_POINT('Ctrl Pts',(24.7595197917227,32.4485117525897,-3.97379660549043E-15));
#38169=CARTESIAN_POINT('Ctrl Pts',(24.7595197917227,32.4485117525897,32.4485117525897));
#38170=CARTESIAN_POINT('Ctrl Pts',(24.7595197917227,3.97379660549043E-15,
32.4485117525897));
#38171=CARTESIAN_POINT('Ctrl Pts',(24.7595197917227,-31.0321087004291,32.4485117525897));
#38172=CARTESIAN_POINT('Ctrl Pts',(24.7595197917227,-32.4162193763075,1.44728584082668));
#38173=CARTESIAN_POINT('Ctrl Pts',(23.6563574780851,-31.9852629652417,1.42804494464108));
#38174=CARTESIAN_POINT('Ctrl Pts',(23.6563574780851,-32.017126031541,0.714377942573002));
#38175=CARTESIAN_POINT('Ctrl Pts',(23.6563574780851,-32.017126031541,3.92096709124241E-15));
#38176=CARTESIAN_POINT('Ctrl Pts',(23.6563574780851,-32.017126031541,-32.017126031541));
#38177=CARTESIAN_POINT('Ctrl Pts',(23.6563574780851,-3.92096709124241E-15,
-32.017126031541));
#38178=CARTESIAN_POINT('Ctrl Pts',(23.6563574780851,32.017126031541,-32.017126031541));
#38179=CARTESIAN_POINT('Ctrl Pts',(23.6563574780851,32.017126031541,-3.92096709124241E-15));
#38180=CARTESIAN_POINT('Ctrl Pts',(23.6563574780851,32.017126031541,32.017126031541));
#38181=CARTESIAN_POINT('Ctrl Pts',(23.6563574780851,3.92096709124241E-15,
32.017126031541));
#38182=CARTESIAN_POINT('Ctrl Pts',(23.6563574780851,-30.6195533053013,32.017126031541));
#38183=CARTESIAN_POINT('Ctrl Pts',(23.6563574780851,-31.9852629652417,1.42804494464108));
#38184=CARTESIAN_POINT('Ctrl Pts',(22.5073180101405,-31.5864702700101,1.41024006077928));
#38185=CARTESIAN_POINT('Ctrl Pts',(22.5073180101405,-31.6179360671638,0.705471068634142));
#38186=CARTESIAN_POINT('Ctrl Pts',(22.5073180101405,-31.6179360671638,3.87208042002978E-15));
#38187=CARTESIAN_POINT('Ctrl Pts',(22.5073180101405,-31.6179360671638,-31.6179360671638));
#38188=CARTESIAN_POINT('Ctrl Pts',(22.5073180101405,-3.87208042002978E-15,
-31.6179360671638));
#38189=CARTESIAN_POINT('Ctrl Pts',(22.5073180101405,31.6179360671638,-31.6179360671638));
#38190=CARTESIAN_POINT('Ctrl Pts',(22.5073180101405,31.6179360671638,-3.87208042002978E-15));
#38191=CARTESIAN_POINT('Ctrl Pts',(22.5073180101405,31.6179360671638,31.6179360671638));
#38192=CARTESIAN_POINT('Ctrl Pts',(22.5073180101405,3.87208042002978E-15,
31.6179360671638));
#38193=CARTESIAN_POINT('Ctrl Pts',(22.5073180101405,-30.237788296751,31.6179360671638));
#38194=CARTESIAN_POINT('Ctrl Pts',(22.5073180101405,-31.5864702700101,1.41024006077928));
#38195=CARTESIAN_POINT('Ctrl Pts',(21.3125219557939,-31.2336232862855,1.394486513532));
#38196=CARTESIAN_POINT('Ctrl Pts',(21.3125219557939,-31.264737584474,0.697590373623125));
#38197=CARTESIAN_POINT('Ctrl Pts',(21.3125219557939,-31.264737584474,3.8288260809008E-15));
#38198=CARTESIAN_POINT('Ctrl Pts',(21.3125219557939,-31.264737584474,-31.264737584474));
#38199=CARTESIAN_POINT('Ctrl Pts',(21.3125219557939,-3.8288260809008E-15,
-31.264737584474));
#38200=CARTESIAN_POINT('Ctrl Pts',(21.3125219557939,31.264737584474,-31.264737584474));
#38201=CARTESIAN_POINT('Ctrl Pts',(21.3125219557939,31.264737584474,-3.8288260809008E-15));
#38202=CARTESIAN_POINT('Ctrl Pts',(21.3125219557939,31.264737584474,31.264737584474));
#38203=CARTESIAN_POINT('Ctrl Pts',(21.3125219557939,3.8288260809008E-15,
31.264737584474));
#38204=CARTESIAN_POINT('Ctrl Pts',(21.3125219557939,-29.9000072055494,31.264737584474));
#38205=CARTESIAN_POINT('Ctrl Pts',(21.3125219557939,-31.2336232862855,1.394486513532));
#38206=CARTESIAN_POINT('Ctrl Pts',(20.0742472323676,-30.9363148057487,1.3812125919422));
#38207=CARTESIAN_POINT('Ctrl Pts',(20.0742472323676,-30.9671329312955,0.690950108671537));
#38208=CARTESIAN_POINT('Ctrl Pts',(20.0742472323676,-30.9671329312955,3.79238002230816E-15));
#38209=CARTESIAN_POINT('Ctrl Pts',(20.0742472323676,-30.9671329312955,-30.9671329312955));
#38210=CARTESIAN_POINT('Ctrl Pts',(20.0742472323676,-3.79238002230816E-15,
-30.9671329312955));
#38211=CARTESIAN_POINT('Ctrl Pts',(20.0742472323676,30.9671329312955,-30.9671329312955));
#38212=CARTESIAN_POINT('Ctrl Pts',(20.0742472323676,30.9671329312955,-3.79238002230816E-15));
#38213=CARTESIAN_POINT('Ctrl Pts',(20.0742472323676,30.9671329312955,30.9671329312955));
#38214=CARTESIAN_POINT('Ctrl Pts',(20.0742472323676,3.79238002230816E-15,
30.9671329312955));
#38215=CARTESIAN_POINT('Ctrl Pts',(20.0742472323676,-29.6153932294878,30.9671329312955));
#38216=CARTESIAN_POINT('Ctrl Pts',(20.0742472323676,-30.9363148057487,1.3812125919422));
#38217=CARTESIAN_POINT('Ctrl Pts',(18.7979917002302,-30.6967495040754,1.3705167280896));
#38218=CARTESIAN_POINT('Ctrl Pts',(18.7979917002302,-30.727328979557,0.685599514321031));
#38219=CARTESIAN_POINT('Ctrl Pts',(18.7979917002302,-30.727328979557,3.76301250811622E-15));
#38220=CARTESIAN_POINT('Ctrl Pts',(18.7979917002302,-30.727328979557,-30.727328979557));
#38221=CARTESIAN_POINT('Ctrl Pts',(18.7979917002302,-3.76301250811622E-15,
-30.727328979557));
#38222=CARTESIAN_POINT('Ctrl Pts',(18.7979917002302,30.727328979557,-30.727328979557));
#38223=CARTESIAN_POINT('Ctrl Pts',(18.7979917002302,30.727328979557,-3.76301250811622E-15));
#38224=CARTESIAN_POINT('Ctrl Pts',(18.7979917002302,30.727328979557,30.727328979557));
#38225=CARTESIAN_POINT('Ctrl Pts',(18.7979917002302,3.76301250811622E-15,
30.727328979557));
#38226=CARTESIAN_POINT('Ctrl Pts',(18.7979917002302,-29.3860569087997,30.727328979557));
#38227=CARTESIAN_POINT('Ctrl Pts',(18.7979917002302,-30.6967495040754,1.3705167280896));
#38228=CARTESIAN_POINT('Ctrl Pts',(17.4917404060759,-30.5108523315028,1.36221698336642));
#38229=CARTESIAN_POINT('Ctrl Pts',(17.4917404060759,-30.5412466200144,0.681447575979399));
#38230=CARTESIAN_POINT('Ctrl Pts',(17.4917404060759,-30.5412466200144,3.74022399151705E-15));
#38231=CARTESIAN_POINT('Ctrl Pts',(17.4917404060759,-30.5412466200144,-30.5412466200144));
#38232=CARTESIAN_POINT('Ctrl Pts',(17.4917404060759,-3.74022399151705E-15,
-30.5412466200144));
#38233=CARTESIAN_POINT('Ctrl Pts',(17.4917404060759,30.5412466200144,-30.5412466200144));
#38234=CARTESIAN_POINT('Ctrl Pts',(17.4917404060759,30.5412466200144,-3.74022399151705E-15));
#38235=CARTESIAN_POINT('Ctrl Pts',(17.4917404060759,30.5412466200144,30.5412466200144));
#38236=CARTESIAN_POINT('Ctrl Pts',(17.4917404060759,3.74022399151705E-15,
30.5412466200144));
#38237=CARTESIAN_POINT('Ctrl Pts',(17.4917404060759,-29.2080971905671,30.5412466200144));
#38238=CARTESIAN_POINT('Ctrl Pts',(17.4917404060759,-30.5108523315028,1.36221698336642));
#38239=CARTESIAN_POINT('Ctrl Pts',(16.1647270995715,-30.3706357712668,1.35595673938413));
#38240=CARTESIAN_POINT('Ctrl Pts',(16.1647270995715,-30.4008903789023,0.678315895682606));
#38241=CARTESIAN_POINT('Ctrl Pts',(16.1647270995715,-30.4008903789023,3.72303530937522E-15));
#38242=CARTESIAN_POINT('Ctrl Pts',(16.1647270995715,-30.4008903789023,-30.4008903789023));
#38243=CARTESIAN_POINT('Ctrl Pts',(16.1647270995715,-3.72303530937522E-15,
-30.4008903789023));
#38244=CARTESIAN_POINT('Ctrl Pts',(16.1647270995715,30.4008903789023,-30.4008903789023));
#38245=CARTESIAN_POINT('Ctrl Pts',(16.1647270995715,30.4008903789023,-3.72303530937522E-15));
#38246=CARTESIAN_POINT('Ctrl Pts',(16.1647270995715,30.4008903789023,30.4008903789023));
#38247=CARTESIAN_POINT('Ctrl Pts',(16.1647270995715,3.72303530937522E-15,
30.4008903789023));
#38248=CARTESIAN_POINT('Ctrl Pts',(16.1647270995715,-29.0738676097412,30.4008903789023));
#38249=CARTESIAN_POINT('Ctrl Pts',(16.1647270995715,-30.3706357712668,1.35595673938413));
#38250=CARTESIAN_POINT('Ctrl Pts',(14.8263876417415,-30.2660684364343,1.3512881251525));
#38251=CARTESIAN_POINT('Ctrl Pts',(14.8263876417415,-30.2962188762245,0.675980426451068));
#38252=CARTESIAN_POINT('Ctrl Pts',(14.8263876417415,-30.2962188762246,3.7102167473036E-15));
#38253=CARTESIAN_POINT('Ctrl Pts',(14.8263876417415,-30.2962188762245,-30.2962188762245));
#38254=CARTESIAN_POINT('Ctrl Pts',(14.8263876417415,-3.7102167473036E-15,
-30.2962188762246));
#38255=CARTESIAN_POINT('Ctrl Pts',(14.8263876417415,30.2962188762245,-30.2962188762245));
#38256=CARTESIAN_POINT('Ctrl Pts',(14.8263876417415,30.2962188762246,-3.7102167473036E-15));
#38257=CARTESIAN_POINT('Ctrl Pts',(14.8263876417415,30.2962188762245,30.2962188762245));
#38258=CARTESIAN_POINT('Ctrl Pts',(14.8263876417415,3.7102167473036E-15,
30.2962188762246));
#38259=CARTESIAN_POINT('Ctrl Pts',(14.8263876417415,-28.9737651004582,30.2962188762245));
#38260=CARTESIAN_POINT('Ctrl Pts',(14.8263876417415,-30.2660684364343,1.3512881251525));
#38261=CARTESIAN_POINT('Ctrl Pts',(13.4853470903953,-30.186937862885,1.34775518513426));
#38262=CARTESIAN_POINT('Ctrl Pts',(13.4853470903953,-30.2170094744125,0.674213077019293));
#38263=CARTESIAN_POINT('Ctrl Pts',(13.4853470903953,-30.2170094744125,3.70051639326446E-15));
#38264=CARTESIAN_POINT('Ctrl Pts',(13.4853470903953,-30.2170094744125,-30.2170094744125));
#38265=CARTESIAN_POINT('Ctrl Pts',(13.4853470903953,-3.70051639326446E-15,
-30.2170094744125));
#38266=CARTESIAN_POINT('Ctrl Pts',(13.4853470903953,30.2170094744125,-30.2170094744125));
#38267=CARTESIAN_POINT('Ctrl Pts',(13.4853470903953,30.2170094744125,-3.70051639326446E-15));
#38268=CARTESIAN_POINT('Ctrl Pts',(13.4853470903953,30.2170094744125,30.2170094744125));
#38269=CARTESIAN_POINT('Ctrl Pts',(13.4853470903953,3.70051639326446E-15,
30.2170094744125));
#38270=CARTESIAN_POINT('Ctrl Pts',(13.4853470903953,-28.8980132513174,30.2170094744125));
#38271=CARTESIAN_POINT('Ctrl Pts',(13.4853470903953,-30.186937862885,1.34775518513426));
#38272=CARTESIAN_POINT('Ctrl Pts',(12.1482076787549,-30.1249424647305,1.34498727870743));
#38273=CARTESIAN_POINT('Ctrl Pts',(12.1482076787549,-30.1549523177074,0.672828434816078));
#38274=CARTESIAN_POINT('Ctrl Pts',(12.1482076787549,-30.1549523177074,3.69291658343215E-15));
#38275=CARTESIAN_POINT('Ctrl Pts',(12.1482076787549,-30.1549523177074,-30.1549523177074));
#38276=CARTESIAN_POINT('Ctrl Pts',(12.1482076787549,-3.69291658343215E-15,
-30.1549523177074));
#38277=CARTESIAN_POINT('Ctrl Pts',(12.1482076787549,30.1549523177074,-30.1549523177074));
#38278=CARTESIAN_POINT('Ctrl Pts',(12.1482076787549,30.1549523177074,-3.69291658343215E-15));
#38279=CARTESIAN_POINT('Ctrl Pts',(12.1482076787549,30.1549523177074,30.1549523177074));
#38280=CARTESIAN_POINT('Ctrl Pts',(12.1482076787549,3.69291658343215E-15,
30.1549523177074));
#38281=CARTESIAN_POINT('Ctrl Pts',(12.1482076787549,-28.8386649382978,30.1549523177074));
#38282=CARTESIAN_POINT('Ctrl Pts',(12.1482076787549,-30.1249424647305,1.34498727870743));
#38283=CARTESIAN_POINT('Ctrl Pts',(10.8190675759626,-30.0746904138676,1.34274367710657));
#38284=CARTESIAN_POINT('Ctrl Pts',(10.8190675759626,-30.1046502067769,0.67170607553629));
#38285=CARTESIAN_POINT('Ctrl Pts',(10.8190675759626,-30.1046502067769,3.686756351518E-15));
#38286=CARTESIAN_POINT('Ctrl Pts',(10.8190675759626,-30.1046502067769,-30.1046502067769));
#38287=CARTESIAN_POINT('Ctrl Pts',(10.8190675759626,-3.686756351518E-15,
-30.1046502067769));
#38288=CARTESIAN_POINT('Ctrl Pts',(10.8190675759626,30.1046502067769,-30.1046502067769));
#38289=CARTESIAN_POINT('Ctrl Pts',(10.8190675759626,30.1046502067769,-3.686756351518E-15));
#38290=CARTESIAN_POINT('Ctrl Pts',(10.8190675759626,30.1046502067769,30.1046502067769));
#38291=CARTESIAN_POINT('Ctrl Pts',(10.8190675759626,3.686756351518E-15,
30.1046502067769));
#38292=CARTESIAN_POINT('Ctrl Pts',(10.8190675759626,-28.7905585540618,30.1046502067769));
#38293=CARTESIAN_POINT('Ctrl Pts',(10.8190675759626,-30.0746904138676,1.34274367710657));
#38294=CARTESIAN_POINT('Ctrl Pts',(9.50027713254189,-30.032840404991,1.3408752011877));
#38295=CARTESIAN_POINT('Ctrl Pts',(9.50027713254189,-30.0627585077754,0.670771372474119));
#38296=CARTESIAN_POINT('Ctrl Pts',(9.50027713254189,-30.0627585077754,3.68162609800869E-15));
#38297=CARTESIAN_POINT('Ctrl Pts',(9.50027713254189,-30.0627585077753,-30.0627585077753));
#38298=CARTESIAN_POINT('Ctrl Pts',(9.50027713254189,-3.68162609800869E-15,
-30.0627585077754));
#38299=CARTESIAN_POINT('Ctrl Pts',(9.5002771325419,30.0627585077753,-30.0627585077753));
#38300=CARTESIAN_POINT('Ctrl Pts',(9.5002771325419,30.0627585077754,-3.68162609800869E-15));
#38301=CARTESIAN_POINT('Ctrl Pts',(9.5002771325419,30.0627585077753,30.0627585077753));
#38302=CARTESIAN_POINT('Ctrl Pts',(9.50027713254189,3.68162609800869E-15,
30.0627585077754));
#38303=CARTESIAN_POINT('Ctrl Pts',(9.50027713254189,-28.750495460661,30.0627585077754));
#38304=CARTESIAN_POINT('Ctrl Pts',(9.50027713254189,-30.032840404991,1.3408752011877));
#38305=CARTESIAN_POINT('Ctrl Pts',(8.45435372222587,-30.0047244129961,1.33961990745209));
#38306=CARTESIAN_POINT('Ctrl Pts',(8.45435372222587,-30.0346145072029,0.670143413137453));
#38307=CARTESIAN_POINT('Ctrl Pts',(8.45435372222587,-30.0346145072029,3.67817945198707E-15));
#38308=CARTESIAN_POINT('Ctrl Pts',(8.45435372222587,-30.0346145072029,-30.0346145072029));
#38309=CARTESIAN_POINT('Ctrl Pts',(8.45435372222587,-3.67817945198707E-15,
-30.0346145072029));
#38310=CARTESIAN_POINT('Ctrl Pts',(8.45435372222587,30.0346145072029,-30.0346145072029));
#38311=CARTESIAN_POINT('Ctrl Pts',(8.45435372222587,30.0346145072029,-3.67817945198707E-15));
#38312=CARTESIAN_POINT('Ctrl Pts',(8.45435372222587,30.0346145072029,30.0346145072029));
#38313=CARTESIAN_POINT('Ctrl Pts',(8.45435372222587,3.67817945198707E-15,
30.0346145072029));
#38314=CARTESIAN_POINT('Ctrl Pts',(8.45435372222587,-28.7235799678431,30.0346145072029));
#38315=CARTESIAN_POINT('Ctrl Pts',(8.45435372222587,-30.0047244129961,1.33961990745209));
#38316=CARTESIAN_POINT('Ctrl Pts',(7.67514864245731,-29.9863740491064,1.33880061938141));
#38317=CARTESIAN_POINT('Ctrl Pts',(7.67514864245731,-30.0162458630552,0.669733565164178));
#38318=CARTESIAN_POINT('Ctrl Pts',(7.67514864245731,-30.0162458630552,3.67592994186105E-15));
#38319=CARTESIAN_POINT('Ctrl Pts',(7.67514864245731,-30.0162458630552,-30.0162458630552));
#38320=CARTESIAN_POINT('Ctrl Pts',(7.67514864245731,-3.67592994186105E-15,
-30.0162458630552));
#38321=CARTESIAN_POINT('Ctrl Pts',(7.67514864245731,30.0162458630552,-30.0162458630552));
#38322=CARTESIAN_POINT('Ctrl Pts',(7.67514864245731,30.0162458630552,-3.67592994186105E-15));
#38323=CARTESIAN_POINT('Ctrl Pts',(7.67514864245731,30.0162458630552,30.0162458630552));
#38324=CARTESIAN_POINT('Ctrl Pts',(7.67514864245731,3.67592994186105E-15,
30.0162458630552));
#38325=CARTESIAN_POINT('Ctrl Pts',(7.67514864245731,-28.7060131294556,30.0162458630552));
#38326=CARTESIAN_POINT('Ctrl Pts',(7.67514864245731,-29.9863740491064,1.33880061938141));
#38327=CARTESIAN_POINT('Ctrl Pts',(7.15799654185577,-29.9753522996976,1.33830853171149));
#38328=CARTESIAN_POINT('Ctrl Pts',(7.15799654185577,-30.0052131340045,0.669487398838306));
#38329=CARTESIAN_POINT('Ctrl Pts',(7.15799654185577,-30.0052131340045,3.67457882222928E-15));
#38330=CARTESIAN_POINT('Ctrl Pts',(7.15799654185577,-30.0052131340045,-30.0052131340045));
#38331=CARTESIAN_POINT('Ctrl Pts',(7.15799654185577,-3.67457882222928E-15,
-30.0052131340045));
#38332=CARTESIAN_POINT('Ctrl Pts',(7.15799654185577,30.0052131340045,-30.0052131340045));
#38333=CARTESIAN_POINT('Ctrl Pts',(7.15799654185577,30.0052131340045,-3.67457882222928E-15));
#38334=CARTESIAN_POINT('Ctrl Pts',(7.15799654185577,30.0052131340045,30.0052131340045));
#38335=CARTESIAN_POINT('Ctrl Pts',(7.15799654185577,3.67457882222928E-15,
30.0052131340045));
#38336=CARTESIAN_POINT('Ctrl Pts',(7.15799654185577,-28.695461987703,30.0052131340045));
#38337=CARTESIAN_POINT('Ctrl Pts',(7.15799654185577,-29.9753522996976,1.33830853171149));
#38338=CARTESIAN_POINT('Ctrl Pts',(6.9,-29.9701443537426,1.33807601272607));
#38339=CARTESIAN_POINT('Ctrl Pts',(6.9,-30.,0.669371081466758));
#38340=CARTESIAN_POINT('Ctrl Pts',(6.9,-30.,3.67394039744206E-15));
#38341=CARTESIAN_POINT('Ctrl Pts',(6.9,-30.,-30.));
#38342=CARTESIAN_POINT('Ctrl Pts',(6.9,-3.67394039744206E-15,-30.));
#38343=CARTESIAN_POINT('Ctrl Pts',(6.9,30.,-30.));
#38344=CARTESIAN_POINT('Ctrl Pts',(6.9,30.,-3.67394039744206E-15));
#38345=CARTESIAN_POINT('Ctrl Pts',(6.9,30.,30.));
#38346=CARTESIAN_POINT('Ctrl Pts',(6.9,3.67394039744206E-15,30.));
#38347=CARTESIAN_POINT('Ctrl Pts',(6.9,-28.6904764110968,30.));
#38348=CARTESIAN_POINT('Ctrl Pts',(6.9,-29.9701443537426,1.33807601272607));
#38349=CARTESIAN_POINT('Ctrl Pts',(6.9,-20.5775906479515,-21.8303175223207));
#38350=CARTESIAN_POINT('Ctrl Pts',(7.85773098116326,-22.0288565043892,-20.4889265372405));
#38351=CARTESIAN_POINT('Ctrl Pts',(8.88781981167334,-23.3171626725998,-19.0414114324084));
#38352=CARTESIAN_POINT('Ctrl Pts',(10.5914578196776,-25.1150390010341,-16.6247285680552));
#38353=CARTESIAN_POINT('Ctrl Pts',(11.2365058953701,-25.7254166302984,-15.703976734769));
#38354=CARTESIAN_POINT('Ctrl Pts',(12.0558885382926,-26.3926147460599,-14.5853792872662));
#38355=CARTESIAN_POINT('Ctrl Pts',(12.1875764958397,-26.4963665374952,-14.4076425286694));
#38356=CARTESIAN_POINT('Ctrl Pts',(13.194901830313,-27.2691057169114,-13.0552778456719));
#38357=CARTESIAN_POINT('Ctrl Pts',(14.2258982134098,-27.991732600527,-11.6381637544796));
#38358=CARTESIAN_POINT('Ctrl Pts',(18.2616480823244,-29.9350198014187,-6.95587410790868));
#38359=CARTESIAN_POINT('Ctrl Pts',(21.0496416709525,-30.7693084982877,-4.29983295736293));
#38360=CARTESIAN_POINT('Ctrl Pts',(25.8000196361138,-32.8040277065106,-1.93741001991749));
#38361=CARTESIAN_POINT('Ctrl Pts',(26.8976561124457,-33.3305524688301,-1.74039351523169));
#38362=CARTESIAN_POINT('Ctrl Pts',(28.0045908801237,-33.8378020212277,-1.58669630450145));
#38363=CARTESIAN_POINT('Ctrl Pts',(28.5235971652406,-34.0754855762016,-1.54532623843658));
#38364=CARTESIAN_POINT('Ctrl Pts',(29.0834839543824,-34.3307100593381,-1.4982885487127));
#38365=CARTESIAN_POINT('Ctrl Pts',(29.1146288039499,-34.3449058451715,-1.49562082188434));
#38366=CARTESIAN_POINT('Ctrl Pts',(29.5949306848436,-34.5637016811193,-1.45589225448014));
#38367=CARTESIAN_POINT('Ctrl Pts',(30.0492939924726,-34.7685410859787,-1.44682754698748));
#38368=CARTESIAN_POINT('Ctrl Pts',(30.5,-34.9699609326822,-1.44976976333441));
#38369=CARTESIAN_POINT('Ctrl Pts',(6.45331003273164,-6.83943894028999,-8.65286216739172));
#38370=CARTESIAN_POINT('Ctrl Pts',(7.20830533428676,-7.28712780725476,-8.29622318255582));
#38371=CARTESIAN_POINT('Ctrl Pts',(7.99924796920644,-7.69991572864563,-7.91909532230128));
#38372=CARTESIAN_POINT('Ctrl Pts',(9.76163642871394,-8.50127829248443,-7.0702837202071));
#38373=CARTESIAN_POINT('Ctrl Pts',(10.7316626231511,-8.8793528128254,-6.57783879792861));
#38374=CARTESIAN_POINT('Ctrl Pts',(12.6608237755523,-9.49392179513702,-5.67260683532432));
#38375=CARTESIAN_POINT('Ctrl Pts',(13.6376935580087,-9.74868549844379,-5.20677839827646));
#38376=CARTESIAN_POINT('Ctrl Pts',(14.8683081444882,-10.0072371758851,-4.68571756497415));
#38377=CARTESIAN_POINT('Ctrl Pts',(15.814981546047,-10.1933420307132,-4.28615487511135));
#38378=CARTESIAN_POINT('Ctrl Pts',(16.7774761024725,-10.3417484740057,-3.90183726466219));
#38379=CARTESIAN_POINT('Ctrl Pts',(18.4438470226175,-10.5575964922699,-3.30966453460613));
#38380=CARTESIAN_POINT('Ctrl Pts',(19.4166260537867,-10.6478897990578,-2.98271399009539));
#38381=CARTESIAN_POINT('Ctrl Pts',(20.8624415465507,-10.7552000633454,-2.5875063027773));
#38382=CARTESIAN_POINT('Ctrl Pts',(21.8144010701944,-10.8125125199159,-2.34040933534244));
#38383=CARTESIAN_POINT('Ctrl Pts',(22.7817704456175,-10.8543372932887,-2.13286375196528));
#38384=CARTESIAN_POINT('Ctrl Pts',(23.3296603631195,-10.8753724962822,-2.03163991938108));
#38385=CARTESIAN_POINT('Ctrl Pts',(23.4469280425869,-10.8796667005723,-2.01025391532517));
#38386=CARTESIAN_POINT('Ctrl Pts',(23.6810288813553,-10.8878000542956,-1.96865773783264));
#38387=CARTESIAN_POINT('Ctrl Pts',(24.0941214149603,-10.9009272596696,-1.89824222375216));
#38388=CARTESIAN_POINT('Ctrl Pts',(24.6899984645715,-10.9167861221079,-1.80575737992305));
#38389=CARTESIAN_POINT('Ctrl Pts',(25.4117472347965,-10.9320835607493,-1.71023812556292));
#38390=CARTESIAN_POINT('Ctrl Pts',(25.8944359856997,-10.9403877892627,-1.65861072075244));
#38391=CARTESIAN_POINT('Ctrl Pts',(26.3669426319602,-10.9478841337461,-1.61476081138877));
#38392=CARTESIAN_POINT('Ctrl Pts',(27.2927605647398,-10.9593568588012,-1.54499465236548));
#38393=CARTESIAN_POINT('Ctrl Pts',(28.2852623623168,-10.9616475307267,-1.51981821556059));
#38394=CARTESIAN_POINT('Ctrl Pts',(29.2044123671999,-10.9652006081482,-1.49506529955051));
#38395=CARTESIAN_POINT('Ctrl Pts',(29.5205491106405,-10.9661656603817,-1.48868169066078));
#38396=CARTESIAN_POINT('Ctrl Pts',(30.1691034959588,-10.9670510696507,-1.48263221141176));
#38397=CARTESIAN_POINT('Ctrl Pts',(31.3134334344234,-10.9664912432219,-1.4864605825931));
#38398=CARTESIAN_POINT('Ctrl Pts',(32.3203424123247,-10.9645690748214,-1.49997009105206));
#38399=CARTESIAN_POINT('Ctrl Pts',(33.1675465322482,-10.9645713457497,-1.49998069520818));
#38400=CARTESIAN_POINT('Ctrl Pts',(33.4947519346945,-10.9645717110255,-1.49998093738942));
#38401=CARTESIAN_POINT('Ctrl Pts',(34.1540738134336,-10.9645721532421,-1.49998231763443));
#38402=CARTESIAN_POINT('Ctrl Pts',(34.81145110075,-10.9645737361772,-1.499985805429));
#38403=CARTESIAN_POINT('Ctrl Pts',(35.7991041415374,-10.9645740230236,-1.49998654292927));
#38404=CARTESIAN_POINT('Ctrl Pts',(37.7734954411133,-10.9645758157224,-1.49999064614178));
#38405=CARTESIAN_POINT('Ctrl Pts',(39.5833333333333,-10.9645797934319,-1.5));
#38406=CARTESIAN_POINT('Ctrl Pts',(40.9,-10.9645797934319,-1.5));
#38407=CARTESIAN_POINT('Ctrl Pts',(6.63336813585096,-9.34202246898051,-11.0008793183436));
#38408=CARTESIAN_POINT('Ctrl Pts',(7.389696336477,-9.9106502389341,-10.5126404716241));
#38409=CARTESIAN_POINT('Ctrl Pts',(8.18028889045472,-10.4323217834721,-10.0000669136624));
#38410=CARTESIAN_POINT('Ctrl Pts',(9.94159575574686,-11.439192222287,-8.85353468669098));
#38411=CARTESIAN_POINT('Ctrl Pts',(10.9109419422818,-11.9102705993651,-8.19201021037899));
#38412=CARTESIAN_POINT('Ctrl Pts',(12.8335218625484,-12.6683977976686,-6.98387303125937));
#38413=CARTESIAN_POINT('Ctrl Pts',(13.8091851210584,-12.9798296118147,-6.36343771133683));
#38414=CARTESIAN_POINT('Ctrl Pts',(15.0310774900381,-13.2915570052696,-5.67481209887734));
#38415=CARTESIAN_POINT('Ctrl Pts',(15.9749773134882,-13.5160612446606,-5.14536755152679));
#38416=CARTESIAN_POINT('Ctrl Pts',(16.930312943506,-13.6911692618857,-4.63930769376668));
#38417=CARTESIAN_POINT('Ctrl Pts',(18.5806860927912,-13.9445588072223,-3.86175938608204));
#38418=CARTESIAN_POINT('Ctrl Pts',(19.548719041905,-14.047648520923,-3.43185831734755));
#38419=CARTESIAN_POINT('Ctrl Pts',(20.9744115808253,-14.1690991173097,-2.91639691217872));
#38420=CARTESIAN_POINT('Ctrl Pts',(21.9189583606346,-14.2328177454448,-2.59280390983887));
#38421=CARTESIAN_POINT('Ctrl Pts',(22.8721113115929,-14.2778669302766,-2.32284159836073));
#38422=CARTESIAN_POINT('Ctrl Pts',(23.4111206282029,-14.300719458499,-2.1913240624154));
#38423=CARTESIAN_POINT('Ctrl Pts',(23.5272640974129,-14.3053783578071,-2.16340494095905));
#38424=CARTESIAN_POINT('Ctrl Pts',(23.7586042074435,-14.3141392731538,-2.10919630050476));
#38425=CARTESIAN_POINT('Ctrl Pts',(24.1668594457504,-14.3281409258012,-2.01743796447889));
#38426=CARTESIAN_POINT('Ctrl Pts',(24.7549510427126,-14.3447231768686,-1.89707890772754));
#38427=CARTESIAN_POINT('Ctrl Pts',(25.4661619742724,-14.3604369110458,-1.77296928480105));
#38428=CARTESIAN_POINT('Ctrl Pts',(25.940793652308,-14.3689791856741,-1.7060154102986));
#38429=CARTESIAN_POINT('Ctrl Pts',(26.4047985025956,-14.3768131131953,-1.64920950338615));
#38430=CARTESIAN_POINT('Ctrl Pts',(27.3109130873601,-14.3886741790609,-1.55899536298034));
#38431=CARTESIAN_POINT('Ctrl Pts',(28.2968127703991,-14.3906288624532,-1.52586579774316));
#38432=CARTESIAN_POINT('Ctrl Pts',(29.216365869052,-14.3942351181099,-1.49337715415662));
#38433=CARTESIAN_POINT('Ctrl Pts',(29.5273677411776,-14.3952146919186,-1.48510498656914));
#38434=CARTESIAN_POINT('Ctrl Pts',(30.1704748351474,-14.3961140069303,-1.47720108681953));
#38435=CARTESIAN_POINT('Ctrl Pts',(31.3076822233502,-14.3955480332033,-1.48219673215098));
#38436=CARTESIAN_POINT('Ctrl Pts',(32.3162781940781,-14.3936026936296,-1.49994928257769));
#38437=CARTESIAN_POINT('Ctrl Pts',(33.1684720644413,-14.3936066618446,-1.49996698297726));
#38438=CARTESIAN_POINT('Ctrl Pts',(33.4950641584122,-14.3936073001223,-1.49996744488463));
#38439=CARTESIAN_POINT('Ctrl Pts',(34.1546952525893,-14.3936080728485,-1.49996977575843));
#38440=CARTESIAN_POINT('Ctrl Pts',(34.811773768313,-14.3936108388537,-1.49997575137036));
#38441=CARTESIAN_POINT('Ctrl Pts',(35.7994747102212,-14.3936113400865,-1.49997700611746));
#38442=CARTESIAN_POINT('Ctrl Pts',(37.7736758948774,-14.3936144726314,-1.499984023326));
#38443=CARTESIAN_POINT('Ctrl Pts',(39.5833333333333,-14.3936214232436,-1.5));
#38444=CARTESIAN_POINT('Ctrl Pts',(40.9,-14.3936214232436,-1.5));
#38445=CARTESIAN_POINT('Ctrl Pts',(6.84643360079894,-15.1545575883324,-16.506001665025));
#38446=CARTESIAN_POINT('Ctrl Pts',(7.61273218496772,-16.0159127642118,-15.7040687667121));
#38447=CARTESIAN_POINT('Ctrl Pts',(8.4126771054426,-16.7980113101253,-14.8690272591124));
#38448=CARTESIAN_POINT('Ctrl Pts',(10.1879439641556,-18.2945580567154,-13.0164926384401));
#38449=CARTESIAN_POINT('Ctrl Pts',(11.1642689802371,-18.9856854823124,-11.9550510602025));
#38450=CARTESIAN_POINT('Ctrl Pts',(13.1036036726265,-20.0861315198186,-10.022452207883));
#38451=CARTESIAN_POINT('Ctrl Pts',(14.0826172183607,-20.5290484396469,-9.03879487952599));
#38452=CARTESIAN_POINT('Ctrl Pts',(15.3089235211201,-20.9656035967448,-7.95158583831005));
#38453=CARTESIAN_POINT('Ctrl Pts',(16.2536562498252,-21.279069264144,-7.11690983506512));
#38454=CARTESIAN_POINT('Ctrl Pts',(17.2094234535123,-21.5156901422925,-6.32372298857519));
#38455=CARTESIAN_POINT('Ctrl Pts',(18.8492103514785,-21.8541559656567,-5.11428176787038));
#38456=CARTESIAN_POINT('Ctrl Pts',(19.8132789859546,-21.9855288021884,-4.44555314736778));
#38457=CARTESIAN_POINT('Ctrl Pts',(21.2105274130183,-22.1378650260475,-3.65671370764623));
#38458=CARTESIAN_POINT('Ctrl Pts',(22.1435262947165,-22.2155499994866,-3.15760868632205));
#38459=CARTESIAN_POINT('Ctrl Pts',(23.0712019161591,-22.2672966100825,-2.74759983583376));
#38460=CARTESIAN_POINT('Ctrl Pts',(23.5926643019347,-22.2940508574536,-2.54861011877026));
#38461=CARTESIAN_POINT('Ctrl Pts',(23.7065967589747,-22.2995097248263,-2.50584172092975));
#38462=CARTESIAN_POINT('Ctrl Pts',(23.9324349207315,-22.3096292230893,-2.42316535684894));
#38463=CARTESIAN_POINT('Ctrl Pts',(24.3308966188196,-22.3255066595418,-2.28324508302851));
#38464=CARTESIAN_POINT('Ctrl Pts',(24.9027307486989,-22.3435822260678,-2.10031694390082));
#38465=CARTESIAN_POINT('Ctrl Pts',(25.5912058020402,-22.3601136597686,-1.91242242103885));
#38466=CARTESIAN_POINT('Ctrl Pts',(26.0479116166522,-22.3691489781576,-1.81155274261716));
#38467=CARTESIAN_POINT('Ctrl Pts',(26.4927766852066,-22.3777261422415,-1.72621142470537));
#38468=CARTESIAN_POINT('Ctrl Pts',(27.3538144829414,-22.3904445374985,-1.59133675559696));
#38469=CARTESIAN_POINT('Ctrl Pts',(28.3239440765631,-22.3916143651133,-1.5395372712982));
#38470=CARTESIAN_POINT('Ctrl Pts',(29.2444087331683,-22.3953365265065,-1.48903537353034));
#38471=CARTESIAN_POINT('Ctrl Pts',(29.5434413064006,-22.3963491807022,-1.4765958448865));
#38472=CARTESIAN_POINT('Ctrl Pts',(30.1738228526165,-22.3972793088217,-1.46445321166482));
#38473=CARTESIAN_POINT('Ctrl Pts',(31.2943937060125,-22.3966964278384,-1.47211763918551));
#38474=CARTESIAN_POINT('Ctrl Pts',(32.3068807810285,-22.394691709999,-1.49983279134388));
#38475=CARTESIAN_POINT('Ctrl Pts',(33.1706991860564,-22.3946974029307,-1.49988437406509));
#38476=CARTESIAN_POINT('Ctrl Pts',(33.495857312607,-22.3946983171245,-1.49988713027318));
#38477=CARTESIAN_POINT('Ctrl Pts',(34.1562063695874,-22.394699425001,-1.49989458266054));
#38478=CARTESIAN_POINT('Ctrl Pts',(34.8125750960603,-22.3947033892012,-1.49991575825724));
#38479=CARTESIAN_POINT('Ctrl Pts',(35.8003855127833,-22.3947041076693,-1.49991999484082));
#38480=CARTESIAN_POINT('Ctrl Pts',(37.7741287617181,-22.394708597346,-1.49994455667285));
#38481=CARTESIAN_POINT('Ctrl Pts',(39.5833333333333,-22.394718559471,-1.5));
#38482=CARTESIAN_POINT('Ctrl Pts',(40.9,-22.394718559471,-1.5));
#38483=CARTESIAN_POINT('Ctrl Pts',(6.90857970435319,-20.8698550272217,-22.1068727166734));
#38484=CARTESIAN_POINT('Ctrl Pts',(7.67983757144493,-22.0336104135999,-20.991774688754));
#38485=CARTESIAN_POINT('Ctrl Pts',(8.48444928201916,-23.0860770683301,-19.8332461961107));
#38486=CARTESIAN_POINT('Ctrl Pts',(10.2687663769551,-25.0905346149111,-17.2709888357559));
#38487=CARTESIAN_POINT('Ctrl Pts',(11.2490111943913,-26.0108786577409,-15.8072894822424));
#38488=CARTESIAN_POINT('Ctrl Pts',(13.2067599054631,-27.4745835397,-13.1283892637642));
#38489=CARTESIAN_POINT('Ctrl Pts',(14.1887708824687,-28.0545611646472,-11.7775873547894));
#38490=CARTESIAN_POINT('Ctrl Pts',(15.4301927253883,-28.6258871350548,-10.2708149751555));
#38491=CARTESIAN_POINT('Ctrl Pts',(16.3793034376203,-29.0320485193235,-9.12509880827948));
#38492=CARTESIAN_POINT('Ctrl Pts',(17.3459407209746,-29.335531334809,-8.0290538541365));
#38493=CARTESIAN_POINT('Ctrl Pts',(19.0016786397101,-29.764530122403,-6.36442803225958));
#38494=CARTESIAN_POINT('Ctrl Pts',(19.9708024570658,-29.9249381814107,-5.44984750618438));
#38495=CARTESIAN_POINT('Ctrl Pts',(21.3726541621532,-30.1088343166975,-4.37628680649797));
#38496=CARTESIAN_POINT('Ctrl Pts',(22.305997327355,-30.2002109026539,-3.69883691082954));
#38497=CARTESIAN_POINT('Ctrl Pts',(23.2278577930096,-30.2581794306256,-3.14826448808768));
#38498=CARTESIAN_POINT('Ctrl Pts',(23.7415516356673,-30.2885183156943,-2.88362049576681));
#38499=CARTESIAN_POINT('Ctrl Pts',(23.8544946510481,-30.2947200062415,-2.82623659223923));
#38500=CARTESIAN_POINT('Ctrl Pts',(24.0777274663499,-30.3060802342181,-2.71573667925153));
#38501=CARTESIAN_POINT('Ctrl Pts',(24.4711727956187,-30.32363513723,-2.52895535356898));
#38502=CARTESIAN_POINT('Ctrl Pts',(25.0334457271175,-30.3429441514165,-2.28601411482693));
#38503=CARTESIAN_POINT('Ctrl Pts',(25.706214488466,-30.3600503901637,-2.03835403030808));
#38504=CARTESIAN_POINT('Ctrl Pts',(26.1486936133439,-30.3694723684124,-1.90670660027133));
#38505=CARTESIAN_POINT('Ctrl Pts',(26.5774366289031,-30.3787139799022,-1.79594947825408));
#38506=CARTESIAN_POINT('Ctrl Pts',(27.3975110717084,-30.392198133447,-1.62272694197858));
#38507=CARTESIAN_POINT('Ctrl Pts',(28.3508259392473,-30.3926064111246,-1.55227638555955));
#38508=CARTESIAN_POINT('Ctrl Pts',(29.2723062856311,-30.3964396342324,-1.48380439950634));
#38509=CARTESIAN_POINT('Ctrl Pts',(29.5594622066961,-30.3974855836748,-1.46775103384065));
#38510=CARTESIAN_POINT('Ctrl Pts',(30.1771168569175,-30.3984465770315,-1.45157152773897));
#38511=CARTESIAN_POINT('Ctrl Pts',(31.281071177308,-30.3978463334884,-1.46177125475314));
#38512=CARTESIAN_POINT('Ctrl Pts',(32.297455993961,-30.3957818406259,-1.49958178095819));
#38513=CARTESIAN_POINT('Ctrl Pts',(33.1729044426911,-30.395789026338,-1.49970257782127));
#38514=CARTESIAN_POINT('Ctrl Pts',(33.4966295876142,-30.3957901777219,-1.4997109685702));
#38515=CARTESIAN_POINT('Ctrl Pts',(34.1576977268014,-30.3957915749198,-1.49972932651149));
#38516=CARTESIAN_POINT('Ctrl Pts',(34.813360769929,-30.3957965718591,-1.4997840805116));
#38517=CARTESIAN_POINT('Ctrl Pts',(35.8012813983216,-30.3957974776821,-1.49979479816102));
#38518=CARTESIAN_POINT('Ctrl Pts',(37.7745713511015,-30.395803137258,-1.49985796376524));
#38519=CARTESIAN_POINT('Ctrl Pts',(39.5833333333333,-30.3958156956984,-1.5));
#38520=CARTESIAN_POINT('Ctrl Pts',(40.9,-30.3958156956984,-1.5));
#38521=CARTESIAN_POINT('Ctrl Pts',(6.93528330520032,-24.1234099037007,-25.3195110382618));
#38522=CARTESIAN_POINT('Ctrl Pts',(7.70864561497005,-25.4600205488393,-24.0266258397084));
#38523=CARTESIAN_POINT('Ctrl Pts',(8.51531156164573,-26.6675788409114,-22.6840056101462));
#38524=CARTESIAN_POINT('Ctrl Pts',(10.3033767345502,-28.9634999585434,-19.7178334181139));
#38525=CARTESIAN_POINT('Ctrl Pts',(11.2853975328499,-30.0157138764656,-18.024966824446));
#38526=CARTESIAN_POINT('Ctrl Pts',(13.2504656206425,-31.6887121402305,-14.920608256729));
#38527=CARTESIAN_POINT('Ctrl Pts',(14.2338911783743,-32.3479754973602,-13.360326515741));
#38528=CARTESIAN_POINT('Ctrl Pts',(15.4814489736579,-32.9977120049688,-11.6128587845954));
#38529=CARTESIAN_POINT('Ctrl Pts',(16.4323633322631,-33.457701559807,-10.2891584164032));
#38530=CARTESIAN_POINT('Ctrl Pts',(17.4036580739675,-33.8004278805126,-9.0188416170732));
#38531=CARTESIAN_POINT('Ctrl Pts',(19.0672887678302,-34.2828730898379,-7.09001985912387));
#38532=CARTESIAN_POINT('Ctrl Pts',(20.0391149919151,-34.4604737318843,-6.03348815316117));
#38533=CARTESIAN_POINT('Ctrl Pts',(21.4462778487112,-34.6632929668281,-4.79159535501523));
#38534=CARTESIAN_POINT('Ctrl Pts',(22.3811728101678,-34.7627792680187,-4.01020122074909));
#38535=CARTESIAN_POINT('Ctrl Pts',(23.3032595484893,-34.8244923190156,-3.37635643636738));
#38536=CARTESIAN_POINT('Ctrl Pts',(23.8149974822583,-34.8569118346709,-3.07312481135076));
#38537=CARTESIAN_POINT('Ctrl Pts',(23.9276845297173,-34.8635414236987,-3.00725282827683));
#38538=CARTESIAN_POINT('Ctrl Pts',(24.1501932465709,-34.8756163196444,-2.88055633977638));
#38539=CARTESIAN_POINT('Ctrl Pts',(24.5421106234083,-34.8941314993696,-2.66656979475214));
#38540=CARTESIAN_POINT('Ctrl Pts',(25.1010166003946,-34.9141289755492,-2.38896069563579));
#38541=CARTESIAN_POINT('Ctrl Pts',(25.7673676623321,-34.9315307898229,-2.10719515267299));
#38542=CARTESIAN_POINT('Ctrl Pts',(26.2032614590243,-34.9411502230501,-1.95837832513291));
#38543=CARTESIAN_POINT('Ctrl Pts',(26.6241220770206,-34.9507523611205,-1.83365744353249));
#38544=CARTESIAN_POINT('Ctrl Pts',(27.4227877709103,-34.9646463474546,-1.64008822157604));
#38545=CARTESIAN_POINT('Ctrl Pts',(28.3660425122777,-34.9646178111257,-1.55920845841384));
#38546=CARTESIAN_POINT('Ctrl Pts',(29.288154079426,-34.9685099768711,-1.48047877405357));
#38547=CARTESIAN_POINT('Ctrl Pts',(29.5685743108623,-34.9695745039167,-1.46254110097229));
#38548=CARTESIAN_POINT('Ctrl Pts',(30.1789566228709,-34.9705522790041,-1.44412472938078));
#38549=CARTESIAN_POINT('Ctrl Pts',(31.273428633048,-34.9699406754865,-1.45573528147979));
#38550=CARTESIAN_POINT('Ctrl Pts',(32.2920480078111,-34.9678391394653,-1.49937027232428));
#38551=CARTESIAN_POINT('Ctrl Pts',(33.1741467941405,-34.9678459524317,-1.4995472544355));
#38552=CARTESIAN_POINT('Ctrl Pts',(33.4970538821705,-34.9678470414555,-1.49956078207587));
#38553=CARTESIAN_POINT('Ctrl Pts',(34.1585338443542,-34.9678483649439,-1.49958825610693));
#38554=CARTESIAN_POINT('Ctrl Pts',(34.8137969787743,-34.9678530956496,-1.49967176946748));
#38555=CARTESIAN_POINT('Ctrl Pts',(35.8017811867034,-34.9678539534013,-1.49968797974803));
#38556=CARTESIAN_POINT('Ctrl Pts',(37.7748158892396,-34.9678593117153,-1.49978412416472));
#38557=CARTESIAN_POINT('Ctrl Pts',(39.5833333333333,-34.967871202114,-1.5));
#38558=CARTESIAN_POINT('Ctrl Pts',(40.9,-34.967871202114,-1.5));
#38559=CARTESIAN_POINT('Origin',(6.9,-25.9807621135332,15.));
#38560=CARTESIAN_POINT('',(6.9,-28.7358750109634,-8.61681422303452));
#38561=CARTESIAN_POINT('Ctrl Pts',(6.9,-10.3676856018661,-3.76156693666918));
#38562=CARTESIAN_POINT('Ctrl Pts',(6.9,-14.103554168739,-4.66834435251375));
#38563=CARTESIAN_POINT('Ctrl Pts',(6.90000000166257,-18.0191477848531,-5.7030525211077));
#38564=CARTESIAN_POINT('Ctrl Pts',(6.90000000166257,-23.666490663791,-7.22296038005705));
#38565=CARTESIAN_POINT('Ctrl Pts',(6.9,-26.2182182108371,-7.92134750786925));
#38566=CARTESIAN_POINT('Ctrl Pts',(6.9,-28.7358750109634,-8.61681422303452));
#38567=CARTESIAN_POINT('Origin',(6.9,0.,0.));
#38568=CARTESIAN_POINT('Origin',(40.9,-7.79422863405995,4.5));
#38569=CARTESIAN_POINT('Ctrl Pts',(40.9,-30.5996231131986,15.9346498339374));
#38570=CARTESIAN_POINT('Ctrl Pts',(40.9,-30.1661818974695,15.6844024313584));
#38571=CARTESIAN_POINT('Ctrl Pts',(40.9,-29.7327406817405,15.4341550287793));
#38572=CARTESIAN_POINT('Ctrl Pts',(40.9,-29.2992994660114,15.1839076262003));
#38573=CARTESIAN_POINT('Ctrl Pts',(30.5,-29.5001797522422,18.8345266621011));
#38574=CARTESIAN_POINT('Ctrl Pts',(30.5,-29.9204226682664,18.176307754627));
#38575=CARTESIAN_POINT('Ctrl Pts',(30.5,-30.3108891324553,17.5));
#38576=CARTESIAN_POINT('Ctrl Pts',(30.5,-47.8108891324553,-12.8108891324553));
#38577=CARTESIAN_POINT('Ctrl Pts',(30.5,-17.5,-30.3108891324553));
#38578=CARTESIAN_POINT('Ctrl Pts',(30.5,12.8108891324553,-47.8108891324553));
#38579=CARTESIAN_POINT('Ctrl Pts',(30.5,30.3108891324553,-17.5));
#38580=CARTESIAN_POINT('Ctrl Pts',(30.5,47.8108891324553,12.8108891324553));
#38581=CARTESIAN_POINT('Ctrl Pts',(30.5,17.5,30.3108891324553));
#38582=CARTESIAN_POINT('Ctrl Pts',(30.5,-11.4877949884694,47.0470003722618));
#38583=CARTESIAN_POINT('Ctrl Pts',(30.5,-29.5001797522422,18.8345266621011));
#38584=CARTESIAN_POINT('Ctrl Pts',(30.3311478274255,-29.4365936489566,18.7939298193791));
#38585=CARTESIAN_POINT('Ctrl Pts',(30.3311478274255,-29.8559307532302,18.1371296685291));
#38586=CARTESIAN_POINT('Ctrl Pts',(30.3311478274255,-30.245555587262,17.4622796600955));
#38587=CARTESIAN_POINT('Ctrl Pts',(30.3311478274255,-47.7078352473574,-12.7832759271665));
#38588=CARTESIAN_POINT('Ctrl Pts',(30.3311478274255,-17.4622796600955,-30.245555587262));
#38589=CARTESIAN_POINT('Ctrl Pts',(30.3311478274255,12.7832759271665,-47.7078352473574));
#38590=CARTESIAN_POINT('Ctrl Pts',(30.3311478274255,30.245555587262,-17.4622796600955));
#38591=CARTESIAN_POINT('Ctrl Pts',(30.3311478274255,47.7078352473574,12.7832759271665));
#38592=CARTESIAN_POINT('Ctrl Pts',(30.3311478274255,17.4622796600955,30.245555587262));
#38593=CARTESIAN_POINT('Ctrl Pts',(30.3311478274255,-11.4630336437997,46.9455930096601));
#38594=CARTESIAN_POINT('Ctrl Pts',(30.3311478274255,-29.4365936489566,18.7939298193791));
#38595=CARTESIAN_POINT('Ctrl Pts',(29.9897712690917,-29.3077924996107,18.7116961278613));
#38596=CARTESIAN_POINT('Ctrl Pts',(29.9897712690917,-29.7252947753835,18.0577698358324));
#38597=CARTESIAN_POINT('Ctrl Pts',(29.9897712690917,-30.1132147882992,17.3858726641896));
#38598=CARTESIAN_POINT('Ctrl Pts',(29.9897712690917,-47.4990874524888,-12.7273421241096));
#38599=CARTESIAN_POINT('Ctrl Pts',(29.9897712690917,-17.3858726641896,-30.1132147882992));
#38600=CARTESIAN_POINT('Ctrl Pts',(29.9897712690917,12.7273421241096,-47.4990874524888));
#38601=CARTESIAN_POINT('Ctrl Pts',(29.9897712690917,30.1132147882992,-17.3858726641896));
#38602=CARTESIAN_POINT('Ctrl Pts',(29.9897712690917,47.4990874524888,12.7273421241096));
#38603=CARTESIAN_POINT('Ctrl Pts',(29.9897712690917,17.3858726641896,30.1132147882992));
#38604=CARTESIAN_POINT('Ctrl Pts',(29.9897712690917,-11.4128766206768,46.7401804402414));
#38605=CARTESIAN_POINT('Ctrl Pts',(29.9897712690917,-29.3077924996107,18.7116961278613));
#38606=CARTESIAN_POINT('Ctrl Pts',(29.4666899049319,-29.1097034403905,18.5852252487451));
#38607=CARTESIAN_POINT('Ctrl Pts',(29.4666899049319,-29.5243838511923,17.935718792976));
#38608=CARTESIAN_POINT('Ctrl Pts',(29.4666899049319,-29.9096819433198,17.2683629213518));
#38609=CARTESIAN_POINT('Ctrl Pts',(29.4666899049319,-47.1780448646716,-12.641319021968));
#38610=CARTESIAN_POINT('Ctrl Pts',(29.4666899049319,-17.2683629213518,-29.9096819433198));
#38611=CARTESIAN_POINT('Ctrl Pts',(29.4666899049319,12.641319021968,-47.1780448646716));
#38612=CARTESIAN_POINT('Ctrl Pts',(29.4666899049319,29.9096819433198,-17.2683629213518));
#38613=CARTESIAN_POINT('Ctrl Pts',(29.4666899049319,47.1780448646716,12.641319021968));
#38614=CARTESIAN_POINT('Ctrl Pts',(29.4666899049319,17.2683629213518,29.9096819433198));
#38615=CARTESIAN_POINT('Ctrl Pts',(29.4666899049319,-11.3357378872557,46.4242672450966));
#38616=CARTESIAN_POINT('Ctrl Pts',(29.4666899049319,-29.1097034403905,18.5852252487451));
#38617=CARTESIAN_POINT('Ctrl Pts',(28.7471241621752,-28.8357745030392,18.4103340474916));
#38618=CARTESIAN_POINT('Ctrl Pts',(28.7471241621752,-29.246552676757,17.7669395953572));
#38619=CARTESIAN_POINT('Ctrl Pts',(28.7471241621752,-29.6282250261092,17.105863694435));
#38620=CARTESIAN_POINT('Ctrl Pts',(28.7471241621752,-46.7340887205442,-12.5223613316742));
#38621=CARTESIAN_POINT('Ctrl Pts',(28.7471241621752,-17.105863694435,-29.6282250261092));
#38622=CARTESIAN_POINT('Ctrl Pts',(28.7471241621752,12.5223613316742,-46.7340887205442));
#38623=CARTESIAN_POINT('Ctrl Pts',(28.7471241621752,29.6282250261092,-17.105863694435));
#38624=CARTESIAN_POINT('Ctrl Pts',(28.7471241621752,46.7340887205442,12.5223613316742));
#38625=CARTESIAN_POINT('Ctrl Pts',(28.7471241621752,17.105863694435,29.6282250261092));
#38626=CARTESIAN_POINT('Ctrl Pts',(28.7471241621752,-11.2290660127069,45.9874043199967));
#38627=CARTESIAN_POINT('Ctrl Pts',(28.7471241621752,-28.8357745030392,18.4103340474916));
#38628=CARTESIAN_POINT('Ctrl Pts',(27.8100958442934,-28.4776836217162,18.1817092625453));
#38629=CARTESIAN_POINT('Ctrl Pts',(27.8100958442934,-28.8833606347823,17.5463046664274));
#38630=CARTESIAN_POINT('Ctrl Pts',(27.8100958442934,-29.2602932679205,16.8934381948013));
#38631=CARTESIAN_POINT('Ctrl Pts',(27.8100958442934,-46.1537314627218,-12.3668550731192));
#38632=CARTESIAN_POINT('Ctrl Pts',(27.8100958442934,-16.8934381948013,-29.2602932679205));
#38633=CARTESIAN_POINT('Ctrl Pts',(27.8100958442934,12.3668550731192,-46.1537314627218));
#38634=CARTESIAN_POINT('Ctrl Pts',(27.8100958442934,29.2602932679205,-16.8934381948013));
#38635=CARTESIAN_POINT('Ctrl Pts',(27.8100958442934,46.1537314627218,12.3668550731192));
#38636=CARTESIAN_POINT('Ctrl Pts',(27.8100958442934,16.8934381948013,29.2602932679205));
#38637=CARTESIAN_POINT('Ctrl Pts',(27.8100958442934,-11.0896202647003,45.4163196022628));
#38638=CARTESIAN_POINT('Ctrl Pts',(27.8100958442934,-28.4776836217162,18.1817092625453));
#38639=CARTESIAN_POINT('Ctrl Pts',(26.8343111708818,-28.1064299010669,17.9446806017473));
#38640=CARTESIAN_POINT('Ctrl Pts',(26.8343111708818,-28.5068182430991,17.3175595557791));
#38641=CARTESIAN_POINT('Ctrl Pts',(26.8343111708818,-28.8788369357517,16.6732042787396));
#38642=CARTESIAN_POINT('Ctrl Pts',(26.8343111708818,-45.5520412144912,-12.2056326570121));
#38643=CARTESIAN_POINT('Ctrl Pts',(26.8343111708818,-16.6732042787396,-28.8788369357517));
#38644=CARTESIAN_POINT('Ctrl Pts',(26.8343111708818,12.2056326570121,-45.5520412144912));
#38645=CARTESIAN_POINT('Ctrl Pts',(26.8343111708818,28.8788369357517,-16.6732042787396));
#38646=CARTESIAN_POINT('Ctrl Pts',(26.8343111708818,45.5520412144912,12.2056326570121));
#38647=CARTESIAN_POINT('Ctrl Pts',(26.8343111708818,16.6732042787396,28.8788369357517));
#38648=CARTESIAN_POINT('Ctrl Pts',(26.8343111708818,-10.9450487174303,44.8242427376375));
#38649=CARTESIAN_POINT('Ctrl Pts',(26.8343111708818,-28.1064299010669,17.9446806017473));
#38650=CARTESIAN_POINT('Ctrl Pts',(25.8181479469611,-27.7272550606068,17.7025946652472));
#38651=CARTESIAN_POINT('Ctrl Pts',(25.8181479469611,-28.1222418918016,17.0839339083798));
#38652=CARTESIAN_POINT('Ctrl Pts',(25.8181479469611,-28.4892417994668,16.4482714219305));
#38653=CARTESIAN_POINT('Ctrl Pts',(25.8181479469611,-44.9375132213974,-12.0409703775363));
#38654=CARTESIAN_POINT('Ctrl Pts',(25.8181479469611,-16.4482714219305,-28.4892417994668));
#38655=CARTESIAN_POINT('Ctrl Pts',(25.8181479469611,12.0409703775363,-44.9375132213974));
#38656=CARTESIAN_POINT('Ctrl Pts',(25.8181479469611,28.4892417994668,-16.4482714219305));
#38657=CARTESIAN_POINT('Ctrl Pts',(25.8181479469611,44.9375132213974,12.0409703775363));
#38658=CARTESIAN_POINT('Ctrl Pts',(25.8181479469611,16.4482714219305,28.4892417994668));
#38659=CARTESIAN_POINT('Ctrl Pts',(25.8181479469611,-10.7973925719907,44.2195332406074));
#38660=CARTESIAN_POINT('Ctrl Pts',(25.8181479469611,-27.7272550606068,17.7025946652472));
#38661=CARTESIAN_POINT('Ctrl Pts',(24.7595197917227,-27.3496265541183,17.4614959928472));
#38662=CARTESIAN_POINT('Ctrl Pts',(24.7595197917227,-27.739233902677,16.8512610227058));
#38663=CARTESIAN_POINT('Ctrl Pts',(24.7595197917227,-28.1012354927406,16.2242558762949));
#38664=CARTESIAN_POINT('Ctrl Pts',(24.7595197917227,-44.3254913690355,-11.8769796164457));
#38665=CARTESIAN_POINT('Ctrl Pts',(24.7595197917227,-16.2242558762949,-28.1012354927406));
#38666=CARTESIAN_POINT('Ctrl Pts',(24.7595197917227,11.8769796164457,-44.3254913690355));
#38667=CARTESIAN_POINT('Ctrl Pts',(24.7595197917227,28.1012354927406,-16.2242558762949));
#38668=CARTESIAN_POINT('Ctrl Pts',(24.7595197917227,44.3254913690355,11.8769796164457));
#38669=CARTESIAN_POINT('Ctrl Pts',(24.7595197917227,16.2242558762949,28.1012354927406));
#38670=CARTESIAN_POINT('Ctrl Pts',(24.7595197917227,-10.6503385912768,43.6172898429552));
#38671=CARTESIAN_POINT('Ctrl Pts',(24.7595197917227,-27.3496265541183,17.4614959928472));
#38672=CARTESIAN_POINT('Ctrl Pts',(23.6563574780851,-26.9860278023044,17.229354682426));
#38673=CARTESIAN_POINT('Ctrl Pts',(23.6563574780851,-27.370455528196,16.627232461942));
#38674=CARTESIAN_POINT('Ctrl Pts',(23.6563574780851,-27.7276444994825,16.0085630157705));
#38675=CARTESIAN_POINT('Ctrl Pts',(23.6563574780851,-43.736207515253,-11.719081483712));
#38676=CARTESIAN_POINT('Ctrl Pts',(23.6563574780851,-16.0085630157705,-27.7276444994825));
#38677=CARTESIAN_POINT('Ctrl Pts',(23.6563574780851,11.719081483712,-43.736207515253));
#38678=CARTESIAN_POINT('Ctrl Pts',(23.6563574780851,27.7276444994825,-16.0085630157705));
#38679=CARTESIAN_POINT('Ctrl Pts',(23.6563574780851,43.736207515253,11.719081483712));
#38680=CARTESIAN_POINT('Ctrl Pts',(23.6563574780851,16.0085630157705,27.7276444994825));
#38681=CARTESIAN_POINT('Ctrl Pts',(23.6563574780851,-10.5087479991522,43.0374211521332));
#38682=CARTESIAN_POINT('Ctrl Pts',(23.6563574780851,-26.9860278023044,17.229354682426));
#38683=CARTESIAN_POINT('Ctrl Pts',(22.5073180101405,-26.649565639321,17.0145388530744));
#38684=CARTESIAN_POINT('Ctrl Pts',(22.5073180101405,-27.029200315079,16.419923900654));
#38685=CARTESIAN_POINT('Ctrl Pts',(22.5073180101405,-27.3819358493961,15.8089680335819));
#38686=CARTESIAN_POINT('Ctrl Pts',(22.5073180101405,-43.190903882978,-11.5729678158142));
#38687=CARTESIAN_POINT('Ctrl Pts',(22.5073180101405,-15.8089680335819,-27.3819358493961));
#38688=CARTESIAN_POINT('Ctrl Pts',(22.5073180101405,11.5729678158142,-43.190903882978));
#38689=CARTESIAN_POINT('Ctrl Pts',(22.5073180101405,27.3819358493961,-15.8089680335819));
#38690=CARTESIAN_POINT('Ctrl Pts',(22.5073180101405,43.190903882978,11.5729678158142));
#38691=CARTESIAN_POINT('Ctrl Pts',(22.5073180101405,15.8089680335819,27.3819358493961));
#38692=CARTESIAN_POINT('Ctrl Pts',(22.5073180101405,-10.3777247856603,42.5008299977716));
#38693=CARTESIAN_POINT('Ctrl Pts',(22.5073180101405,-26.649565639321,17.0145388530744));
#38694=CARTESIAN_POINT('Ctrl Pts',(21.3125219557939,-26.3518679613905,16.8244723890963));
#38695=CARTESIAN_POINT('Ctrl Pts',(21.3125219557939,-26.727261803997,16.2364997772301));
#38696=CARTESIAN_POINT('Ctrl Pts',(21.3125219557939,-27.0760569908086,15.632368792237));
#38697=CARTESIAN_POINT('Ctrl Pts',(21.3125219557939,-42.7084257830456,-11.4436881985716));
#38698=CARTESIAN_POINT('Ctrl Pts',(21.3125219557939,-15.632368792237,-27.0760569908086));
#38699=CARTESIAN_POINT('Ctrl Pts',(21.3125219557939,11.4436881985716,-42.7084257830456));
#38700=CARTESIAN_POINT('Ctrl Pts',(21.3125219557939,27.0760569908086,-15.632368792237));
#38701=CARTESIAN_POINT('Ctrl Pts',(21.3125219557939,42.7084257830456,11.4436881985716));
#38702=CARTESIAN_POINT('Ctrl Pts',(21.3125219557939,15.632368792237,27.0760569908086));
#38703=CARTESIAN_POINT('Ctrl Pts',(21.3125219557939,-10.2617970211066,42.0260605935833));
#38704=CARTESIAN_POINT('Ctrl Pts',(21.3125219557939,-26.3518679613905,16.8244723890963));
#38705=CARTESIAN_POINT('Ctrl Pts',(20.0742472323676,-26.1010282252799,16.6643225955232));
#38706=CARTESIAN_POINT('Ctrl Pts',(20.0742472323676,-26.4728487465358,16.0819468125049));
#38707=CARTESIAN_POINT('Ctrl Pts',(20.0742472323676,-26.8183238008715,15.4835664656478));
#38708=CARTESIAN_POINT('Ctrl Pts',(20.0742472323676,-42.3018902665193,-11.3347573352238));
#38709=CARTESIAN_POINT('Ctrl Pts',(20.0742472323676,-15.4835664656478,-26.8183238008715));
#38710=CARTESIAN_POINT('Ctrl Pts',(20.0742472323676,11.3347573352238,-42.3018902665193));
#38711=CARTESIAN_POINT('Ctrl Pts',(20.0742472323676,26.8183238008715,-15.4835664656478));
#38712=CARTESIAN_POINT('Ctrl Pts',(20.0742472323676,42.3018902665193,11.3347573352238));
#38713=CARTESIAN_POINT('Ctrl Pts',(20.0742472323676,15.4835664656478,26.8183238008715));
#38714=CARTESIAN_POINT('Ctrl Pts',(20.0742472323676,-10.1641164141543,41.6260204156154));
#38715=CARTESIAN_POINT('Ctrl Pts',(20.0742472323676,-26.1010282252799,16.6643225955232));
#38716=CARTESIAN_POINT('Ctrl Pts',(18.7979917002302,-25.8989065200918,16.5352770548748));
#38717=CARTESIAN_POINT('Ctrl Pts',(18.7979917002302,-26.2678477295776,15.9574110860028));
#38718=CARTESIAN_POINT('Ctrl Pts',(18.7979917002302,-26.6106474867381,15.3636644897785));
#38719=CARTESIAN_POINT('Ctrl Pts',(18.7979917002302,-41.9743119765166,-11.2469829969596));
#38720=CARTESIAN_POINT('Ctrl Pts',(18.7979917002302,-15.3636644897785,-26.6106474867381));
#38721=CARTESIAN_POINT('Ctrl Pts',(18.7979917002302,11.2469829969596,-41.9743119765166));
#38722=CARTESIAN_POINT('Ctrl Pts',(18.7979917002302,26.6106474867381,-15.3636644897785));
#38723=CARTESIAN_POINT('Ctrl Pts',(18.7979917002302,41.9743119765166,11.2469829969596));
#38724=CARTESIAN_POINT('Ctrl Pts',(18.7979917002302,15.3636644897785,26.6106474867381));
#38725=CARTESIAN_POINT('Ctrl Pts',(18.7979917002302,-10.0854073102973,41.303675941138));
#38726=CARTESIAN_POINT('Ctrl Pts',(18.7979917002302,-25.8989065200918,16.5352770548748));
#38727=CARTESIAN_POINT('Ctrl Pts',(17.4917404060759,-25.7420647185138,16.4351406788133));
#38728=CARTESIAN_POINT('Ctrl Pts',(17.4917404060759,-26.1087716481884,15.8607742221527));
#38729=CARTESIAN_POINT('Ctrl Pts',(17.4917404060759,-26.4494954361781,15.2706233100072));
#38730=CARTESIAN_POINT('Ctrl Pts',(17.4917404060759,-41.7201187461852,-11.1788721261709));
#38731=CARTESIAN_POINT('Ctrl Pts',(17.4917404060759,-15.2706233100072,-26.4494954361781));
#38732=CARTESIAN_POINT('Ctrl Pts',(17.4917404060759,11.1788721261709,-41.7201187461852));
#38733=CARTESIAN_POINT('Ctrl Pts',(17.4917404060759,26.4494954361781,-15.2706233100072));
#38734=CARTESIAN_POINT('Ctrl Pts',(17.4917404060759,41.7201187461852,11.1788721261709));
#38735=CARTESIAN_POINT('Ctrl Pts',(17.4917404060759,15.2706233100072,26.4494954361781));
#38736=CARTESIAN_POINT('Ctrl Pts',(17.4917404060759,-10.0243308532288,41.0535440314616));
#38737=CARTESIAN_POINT('Ctrl Pts',(17.4917404060759,-25.7420647185138,16.4351406788133));
#38738=CARTESIAN_POINT('Ctrl Pts',(16.1647270995715,-25.6237637373094,16.3596108683728));
#38739=CARTESIAN_POINT('Ctrl Pts',(16.1647270995715,-25.988785417954,15.7878839869031));
#38740=CARTESIAN_POINT('Ctrl Pts',(16.1647270995715,-26.3279433657953,15.2004451894512));
#38741=CARTESIAN_POINT('Ctrl Pts',(16.1647270995715,-41.5283885552464,-11.1274981763441));
#38742=CARTESIAN_POINT('Ctrl Pts',(16.1647270995715,-15.2004451894512,-26.3279433657953));
#38743=CARTESIAN_POINT('Ctrl Pts',(16.1647270995715,11.1274981763441,-41.5283885552464));
#38744=CARTESIAN_POINT('Ctrl Pts',(16.1647270995715,26.3279433657953,-15.2004451894512));
#38745=CARTESIAN_POINT('Ctrl Pts',(16.1647270995715,41.5283885552464,11.1274981763441));
#38746=CARTESIAN_POINT('Ctrl Pts',(16.1647270995715,15.2004451894512,26.3279433657953));
#38747=CARTESIAN_POINT('Ctrl Pts',(16.1647270995715,-9.97826274685029,40.8648771706659));
#38748=CARTESIAN_POINT('Ctrl Pts',(16.1647270995715,-25.6237637373094,16.3596108683728));
#38749=CARTESIAN_POINT('Ctrl Pts',(14.8263876417415,-25.5355400760542,16.3032840624315));
#38750=CARTESIAN_POINT('Ctrl Pts',(14.8263876417415,-25.8993049721986,15.7335256598799));
#38751=CARTESIAN_POINT('Ctrl Pts',(14.8263876417415,-26.2372951854241,15.1481094381123));
#38752=CARTESIAN_POINT('Ctrl Pts',(14.8263876417415,-41.3854046235364,-11.0891857473118));
#38753=CARTESIAN_POINT('Ctrl Pts',(14.8263876417415,-15.1481094381123,-26.2372951854241));
#38754=CARTESIAN_POINT('Ctrl Pts',(14.8263876417415,11.0891857473118,-41.3854046235364));
#38755=CARTESIAN_POINT('Ctrl Pts',(14.8263876417415,26.2372951854241,-15.1481094381123));
#38756=CARTESIAN_POINT('Ctrl Pts',(14.8263876417415,41.3854046235364,11.0891857473118));
#38757=CARTESIAN_POINT('Ctrl Pts',(14.8263876417415,15.1481094381123,26.2372951854241));
#38758=CARTESIAN_POINT('Ctrl Pts',(14.8263876417415,-9.94390718216752,40.7241777356532));
#38759=CARTESIAN_POINT('Ctrl Pts',(14.8263876417415,-25.5355400760542,16.3032840624315));
#38760=CARTESIAN_POINT('Ctrl Pts',(13.4853470903953,-25.4687774591536,16.260659159851));
#38761=CARTESIAN_POINT('Ctrl Pts',(13.4853470903953,-25.8315912927267,15.6923903894687));
#38762=CARTESIAN_POINT('Ctrl Pts',(13.4853470903953,-26.1686978312363,15.1085047372063));
#38763=CARTESIAN_POINT('Ctrl Pts',(13.4853470903953,-41.2772025684426,-11.06019309403));
#38764=CARTESIAN_POINT('Ctrl Pts',(13.4853470903953,-15.1085047372063,-26.1686978312363));
#38765=CARTESIAN_POINT('Ctrl Pts',(13.4853470903953,11.06019309403,-41.2772025684426));
#38766=CARTESIAN_POINT('Ctrl Pts',(13.4853470903953,26.1686978312363,-15.1085047372063));
#38767=CARTESIAN_POINT('Ctrl Pts',(13.4853470903953,41.2772025684426,11.06019309403));
#38768=CARTESIAN_POINT('Ctrl Pts',(13.4853470903953,15.1085047372063,26.1686978312363));
#38769=CARTESIAN_POINT('Ctrl Pts',(13.4853470903953,-9.91790885733393,40.617704456895));
#38770=CARTESIAN_POINT('Ctrl Pts',(13.4853470903953,-25.4687774591536,16.260659159851));
#38771=CARTESIAN_POINT('Ctrl Pts',(12.1482076787549,-25.4164718226475,16.2272643834928));
#38772=CARTESIAN_POINT('Ctrl Pts',(12.1482076787549,-25.778540539635,15.660162675793));
#38773=CARTESIAN_POINT('Ctrl Pts',(12.1482076787549,-26.1149547570431,15.0774761588537));
#38774=CARTESIAN_POINT('Ctrl Pts',(12.1482076787549,-41.1924309158968,-11.0374785981893));
#38775=CARTESIAN_POINT('Ctrl Pts',(12.1482076787549,-15.0774761588537,-26.1149547570431));
#38776=CARTESIAN_POINT('Ctrl Pts',(12.1482076787549,11.0374785981893,-41.1924309158968));
#38777=CARTESIAN_POINT('Ctrl Pts',(12.1482076787549,26.1149547570431,-15.0774761588537));
#38778=CARTESIAN_POINT('Ctrl Pts',(12.1482076787549,41.1924309158968,11.0374785981893));
#38779=CARTESIAN_POINT('Ctrl Pts',(12.1482076787549,15.0774761588537,26.1149547570431));
#38780=CARTESIAN_POINT('Ctrl Pts',(12.1482076787549,-9.89754028893977,40.534287226192));
#38781=CARTESIAN_POINT('Ctrl Pts',(12.1482076787549,-25.4164718226475,16.2272643834928));
#38782=CARTESIAN_POINT('Ctrl Pts',(10.8190675759626,-25.3740740708084,16.200195342079));
#38783=CARTESIAN_POINT('Ctrl Pts',(10.8190675759626,-25.7355388133451,15.6340396286792));
#38784=CARTESIAN_POINT('Ctrl Pts',(10.8190675759626,-26.0713918511132,15.0523251033885));
#38785=CARTESIAN_POINT('Ctrl Pts',(10.8190675759626,-41.1237169545017,-11.0190667477248));
#38786=CARTESIAN_POINT('Ctrl Pts',(10.8190675759626,-15.0523251033885,-26.0713918511132));
#38787=CARTESIAN_POINT('Ctrl Pts',(10.8190675759626,11.0190667477248,-41.1237169545017));
#38788=CARTESIAN_POINT('Ctrl Pts',(10.8190675759626,26.0713918511132,-15.0523251033885));
#38789=CARTESIAN_POINT('Ctrl Pts',(10.8190675759626,41.1237169545017,11.0190667477248));
#38790=CARTESIAN_POINT('Ctrl Pts',(10.8190675759626,15.0523251033885,26.0713918511132));
#38791=CARTESIAN_POINT('Ctrl Pts',(10.8190675759626,-9.88102999357242,40.4666711281441));
#38792=CARTESIAN_POINT('Ctrl Pts',(10.8190675759626,-25.3740740708084,16.200195342079));
#38793=CARTESIAN_POINT('Ctrl Pts',(9.50027713254189,-25.3387651379321,16.1776521900286));
#38794=CARTESIAN_POINT('Ctrl Pts',(9.50027713254189,-25.6997268893332,15.6122843025816));
#38795=CARTESIAN_POINT('Ctrl Pts',(9.50027713254189,-26.0351125755702,15.0313792538877));
#38796=CARTESIAN_POINT('Ctrl Pts',(9.50027713254189,-41.0664918294579,-11.0037333216825));
#38797=CARTESIAN_POINT('Ctrl Pts',(9.50027713254189,-15.0313792538877,-26.0351125755702));
#38798=CARTESIAN_POINT('Ctrl Pts',(9.5002771325419,11.0037333216825,-41.0664918294579));
#38799=CARTESIAN_POINT('Ctrl Pts',(9.5002771325419,26.0351125755702,-15.0313792538877));
#38800=CARTESIAN_POINT('Ctrl Pts',(9.5002771325419,41.0664918294579,11.0037333216825));
#38801=CARTESIAN_POINT('Ctrl Pts',(9.50027713254189,15.0313792538877,26.0351125755702));
#38802=CARTESIAN_POINT('Ctrl Pts',(9.50027713254189,-9.8672801864339,40.4103603059007));
#38803=CARTESIAN_POINT('Ctrl Pts',(9.50027713254189,-25.3387651379321,16.1776521900286));
#38804=CARTESIAN_POINT('Ctrl Pts',(8.45435372222587,-25.3150436214797,16.1625070777669));
#38805=CARTESIAN_POINT('Ctrl Pts',(8.45435372222587,-25.6756674495416,15.5976684735573));
#38806=CARTESIAN_POINT('Ctrl Pts',(8.45435372222587,-26.0107391561104,15.0173072536015));
#38807=CARTESIAN_POINT('Ctrl Pts',(8.45435372222587,-41.0280464097118,-10.9934319025089));
#38808=CARTESIAN_POINT('Ctrl Pts',(8.45435372222587,-15.0173072536015,-26.0107391561104));
#38809=CARTESIAN_POINT('Ctrl Pts',(8.45435372222587,10.9934319025089,-41.0280464097118));
#38810=CARTESIAN_POINT('Ctrl Pts',(8.45435372222587,26.0107391561104,-15.0173072536015));
#38811=CARTESIAN_POINT('Ctrl Pts',(8.45435372222587,41.0280464097118,10.9934319025089));
#38812=CARTESIAN_POINT('Ctrl Pts',(8.45435372222587,15.0173072536015,26.0107391561104));
#38813=CARTESIAN_POINT('Ctrl Pts',(8.45435372222587,-9.85804268618443,40.3725291400319));
#38814=CARTESIAN_POINT('Ctrl Pts',(8.45435372222587,-25.3150436214797,16.1625070777669));
#38815=CARTESIAN_POINT('Ctrl Pts',(7.67514864245731,-25.2995613842179,16.1526223715399));
#38816=CARTESIAN_POINT('Ctrl Pts',(7.67514864245731,-25.6599646610633,15.5881292127269));
#38817=CARTESIAN_POINT('Ctrl Pts',(7.67514864245731,-25.9948314436454,15.0081229315276));
#38818=CARTESIAN_POINT('Ctrl Pts',(7.67514864245731,-41.0029543751729,-10.9867085121177));
#38819=CARTESIAN_POINT('Ctrl Pts',(7.67514864245731,-15.0081229315276,-25.9948314436454));
#38820=CARTESIAN_POINT('Ctrl Pts',(7.67514864245731,10.9867085121177,-41.0029543751729));
#38821=CARTESIAN_POINT('Ctrl Pts',(7.67514864245731,25.9948314436454,-15.0081229315276));
#38822=CARTESIAN_POINT('Ctrl Pts',(7.67514864245731,41.0029543751729,10.9867085121177));
#38823=CARTESIAN_POINT('Ctrl Pts',(7.67514864245731,15.0081229315276,25.9948314436454));
#38824=CARTESIAN_POINT('Ctrl Pts',(7.67514864245731,-9.85201367995056,40.3478380083732));
#38825=CARTESIAN_POINT('Ctrl Pts',(7.67514864245731,-25.2995613842179,16.1526223715399));
#38826=CARTESIAN_POINT('Ctrl Pts',(7.15799654185577,-25.2902623130707,16.1466853364124));
#38827=CARTESIAN_POINT('Ctrl Pts',(7.15799654185577,-25.6505331205953,15.5823996619098));
#38828=CARTESIAN_POINT('Ctrl Pts',(7.15799654185577,-25.9852768200144,15.0026065670023));
#38829=CARTESIAN_POINT('Ctrl Pts',(7.15799654185577,-40.9878833870167,-10.9826702530121));
#38830=CARTESIAN_POINT('Ctrl Pts',(7.15799654185577,-15.0026065670023,-25.9852768200144));
#38831=CARTESIAN_POINT('Ctrl Pts',(7.15799654185577,10.9826702530121,-40.9878833870167));
#38832=CARTESIAN_POINT('Ctrl Pts',(7.15799654185577,25.9852768200144,-15.0026065670023));
#38833=CARTESIAN_POINT('Ctrl Pts',(7.15799654185577,40.9878833870167,10.9826702530121));
#38834=CARTESIAN_POINT('Ctrl Pts',(7.15799654185577,15.0026065670023,25.9852768200144));
#38835=CARTESIAN_POINT('Ctrl Pts',(7.15799654185577,-9.84839248767922,40.3330078138659));
#38836=CARTESIAN_POINT('Ctrl Pts',(7.15799654185577,-25.2902623130707,16.1466853364124));
#38837=CARTESIAN_POINT('Ctrl Pts',(6.9,-25.2858683590648,16.1438799960867));
#38838=CARTESIAN_POINT('Ctrl Pts',(6.9,-25.6460765727998,15.5796923611089));
#38839=CARTESIAN_POINT('Ctrl Pts',(6.9,-25.9807621135332,15.));
#38840=CARTESIAN_POINT('Ctrl Pts',(6.9,-40.9807621135332,-10.9807621135331));
#38841=CARTESIAN_POINT('Ctrl Pts',(6.9,-15.,-25.9807621135332));
#38842=CARTESIAN_POINT('Ctrl Pts',(6.9,10.9807621135331,-40.9807621135332));
#38843=CARTESIAN_POINT('Ctrl Pts',(6.9,25.9807621135332,-15.));
#38844=CARTESIAN_POINT('Ctrl Pts',(6.9,40.9807621135332,10.9807621135331));
#38845=CARTESIAN_POINT('Ctrl Pts',(6.9,15.,25.9807621135332));
#38846=CARTESIAN_POINT('Ctrl Pts',(6.9,-9.84668141868803,40.3260003190816));
#38847=CARTESIAN_POINT('Ctrl Pts',(6.9,-25.2858683590648,16.1438799960867));
#38848=CARTESIAN_POINT('Ctrl Pts',(6.9,-28.7358750109634,-8.61681422303452));
#38849=CARTESIAN_POINT('Ctrl Pts',(7.85773098116326,-29.3220126177434,-6.72950262532883));
#38850=CARTESIAN_POINT('Ctrl Pts',(8.88781981167334,-29.7139609348499,-4.83176468807716));
#38851=CARTESIAN_POINT('Ctrl Pts',(10.5914578196776,-30.0626260759601,-1.83991777043967));
#38852=CARTESIAN_POINT('Ctrl Pts',(11.2365058953701,-30.1308526921615,-0.737334477600522));
#38853=CARTESIAN_POINT('Ctrl Pts',(12.0558885382926,-30.1493644860168,0.56499838642607));
#38854=CARTESIAN_POINT('Ctrl Pts',(12.1875764958397,-30.1503477937894,0.770798830274837));
#38855=CARTESIAN_POINT('Ctrl Pts',(13.194901830313,-30.1433772121647,2.3283505906396));
#38856=CARTESIAN_POINT('Ctrl Pts',(14.2258982134098,-30.0606334052373,3.91692083548089));
#38857=CARTESIAN_POINT('Ctrl Pts',(18.2616480823244,-29.4024246647732,8.94354621773404));
#38858=CARTESIAN_POINT('Ctrl Pts',(21.0496416709525,-28.796919295079,11.660889676038));
#38859=CARTESIAN_POINT('Ctrl Pts',(25.8000196361138,-29.3778263502455,14.7241675584603));
#38860=CARTESIAN_POINT('Ctrl Pts',(26.8976561124457,-29.7353019177929,15.1580512376427));
#38861=CARTESIAN_POINT('Ctrl Pts',(28.0045908801237,-30.0977443108623,15.5447817028247));
#38862=CARTESIAN_POINT('Ctrl Pts',(28.5235971652406,-30.2828992744991,15.6994510084801));
#38863=CARTESIAN_POINT('Ctrl Pts',(29.0834839543824,-30.4804113157012,15.8677990842846));
#38864=CARTESIAN_POINT('Ctrl Pts',(29.1146288039499,-30.4913713634453,15.877207296405));
#38865=CARTESIAN_POINT('Ctrl Pts',(29.5949306848436,-30.6609898319163,16.0210111630069));
#38866=CARTESIAN_POINT('Ctrl Pts',(30.0492939924726,-30.8338536064743,16.1312811324031));
#38867=CARTESIAN_POINT('Ctrl Pts',(30.5,-31.0097594187194,16.229443021655));
#38868=CARTESIAN_POINT('Ctrl Pts',(6.45331003273164,-10.2495589536195,-4.07387898226151));
#38869=CARTESIAN_POINT('Ctrl Pts',(7.20830533428676,-10.4589493929845,-3.54117612793134));
#38870=CARTESIAN_POINT('Ctrl Pts',(7.99943720515023,-10.6278530262204,-3.00808536723907));
#38871=CARTESIAN_POINT('Ctrl Pts',(9.76195392812149,-10.8974188156737,-1.87226624217412));
#38872=CARTESIAN_POINT('Ctrl Pts',(10.7319699357145,-10.978614804603,-1.2567580486118));
#38873=CARTESIAN_POINT('Ctrl Pts',(12.6618070777417,-11.0581512103982,-0.165209663835397));
#38874=CARTESIAN_POINT('Ctrl Pts',(13.6366888866736,-11.0460663569154,0.364704064273057));
#38875=CARTESIAN_POINT('Ctrl Pts',(15.55636942495,-10.9884970038505,1.27025231764748));
#38876=CARTESIAN_POINT('Ctrl Pts',(16.5294822240035,-10.9232664847119,1.69980161462952));
#38877=CARTESIAN_POINT('Ctrl Pts',(18.4405353898674,-10.79829507883,2.41132585012623));
#38878=CARTESIAN_POINT('Ctrl Pts',(19.4148048972757,-10.7128845485964,2.74047342809725));
#38879=CARTESIAN_POINT('Ctrl Pts',(20.6320159197514,-10.6248232626626,3.07372863623311));
#38880=CARTESIAN_POINT('Ctrl Pts',(21.1045081958651,-10.5890632628362,3.19855905527616));
#38881=CARTESIAN_POINT('Ctrl Pts',(22.0534615877,-10.517515820459,3.42883778652053));
#38882=CARTESIAN_POINT('Ctrl Pts',(22.7823820470183,-10.4664588970829,3.58029681662344));
#38883=CARTESIAN_POINT('Ctrl Pts',(23.3297776630268,-10.4341170945838,3.67835397010646));
#38884=CARTESIAN_POINT('Ctrl Pts',(23.4470599317459,-10.4271412460568,3.69902619132828));
#38885=CARTESIAN_POINT('Ctrl Pts',(23.6811266122301,-10.4133903945396,3.73910834650872));
#38886=CARTESIAN_POINT('Ctrl Pts',(24.094173095085,-10.3895545652129,3.80664723977494));
#38887=CARTESIAN_POINT('Ctrl Pts',(24.6899146335616,-10.3570603924452,3.8946407511));
#38888=CARTESIAN_POINT('Ctrl Pts',(25.2912361170961,-10.3283061836388,3.96994444386569));
#38889=CARTESIAN_POINT('Ctrl Pts',(25.7735285180352,-10.3085973054881,4.02162740546583));
#38890=CARTESIAN_POINT('Ctrl Pts',(26.0148283477101,-10.3000025859218,4.04448759176681));
#38891=CARTESIAN_POINT('Ctrl Pts',(26.5981242438445,-10.2809495486037,4.09600397233593));
#38892=CARTESIAN_POINT('Ctrl Pts',(27.5413774795631,-10.2607319091994,4.14752077886532));
#38893=CARTESIAN_POINT('Ctrl Pts',(28.5384263877915,-10.2503835882544,4.17105255246829));
#38894=CARTESIAN_POINT('Ctrl Pts',(29.123550305837,-10.2444533826691,4.18584784382928));
#38895=CARTESIAN_POINT('Ctrl Pts',(29.2812719873802,-10.2430815653884,4.18934848102512));
#38896=CARTESIAN_POINT('Ctrl Pts',(29.6033573831701,-10.2409825864506,4.19465178436656));
#38897=CARTESIAN_POINT('Ctrl Pts',(30.1682075695061,-10.2390432854401,4.19956029863434));
#38898=CARTESIAN_POINT('Ctrl Pts',(31.3151152846709,-10.2404426493562,4.19601580459667));
#38899=CARTESIAN_POINT('Ctrl Pts',(32.3203773995797,-10.2455622764132,4.18330340731803));
#38900=CARTESIAN_POINT('Ctrl Pts',(33.1677006908683,-10.245571342205,4.18329188254759));
#38901=CARTESIAN_POINT('Ctrl Pts',(33.4949132850991,-10.2455724350351,4.18329063364476));
#38902=CARTESIAN_POINT('Ctrl Pts',(34.1541785734607,-10.2455743198855,4.18328832445807));
#38903=CARTESIAN_POINT('Ctrl Pts',(34.976129104799,-10.2455804319184,4.18328098024987));
#38904=CARTESIAN_POINT('Ctrl Pts',(35.9637295000903,-10.2455829874647,4.18327789132127));
#38905=CARTESIAN_POINT('Ctrl Pts',(37.938359040684,-10.2455864680815,4.1832737025367));
#38906=CARTESIAN_POINT('Ctrl Pts',(39.5833333333333,-10.2456046429336,4.18325179103929));
#38907=CARTESIAN_POINT('Ctrl Pts',(40.9,-10.2456046429336,4.18325179103929));
#38908=CARTESIAN_POINT('Ctrl Pts',(6.63336813585096,-13.590868440034,-4.85602971916216));
#38909=CARTESIAN_POINT('Ctrl Pts',(7.389696336477,-13.8391951107513,-4.14888858981181));
#38910=CARTESIAN_POINT('Ctrl Pts',(8.18053946683774,-14.0346488726453,-3.44401143686367));
#38911=CARTESIAN_POINT('Ctrl Pts',(9.94201947683641,-14.3333081335907,-1.94757748540838));
#38912=CARTESIAN_POINT('Ctrl Pts',(10.9113717350149,-14.4104989873604,-1.13915583855168));
#38913=CARTESIAN_POINT('Ctrl Pts',(12.8347397322171,-14.4628660834127,0.286629408466327));
#38914=CARTESIAN_POINT('Ctrl Pts',(13.808142871698,-14.4226409916871,0.978270473832921));
#38915=CARTESIAN_POINT('Ctrl Pts',(15.7151185916567,-14.3061107665235,2.15221389622412));
#38916=CARTESIAN_POINT('Ctrl Pts',(16.6852254797785,-14.2015789338064,2.70962741922244));
#38917=CARTESIAN_POINT('Ctrl Pts',(18.5768226767694,-14.0076819635675,3.62608620812781));
#38918=CARTESIAN_POINT('Ctrl Pts',(19.5464729449597,-13.8818273075211,4.05120533415429));
#38919=CARTESIAN_POINT('Ctrl Pts',(20.7463406818481,-13.7535017581768,4.47793026920172));
#38920=CARTESIAN_POINT('Ctrl Pts',(21.2156214332097,-13.7015810566901,4.63869318435445));
#38921=CARTESIAN_POINT('Ctrl Pts',(22.1537708528638,-13.5988388255709,4.9339087652619));
#38922=CARTESIAN_POINT('Ctrl Pts',(22.8728508922897,-13.5262523639447,5.12767073297799));
#38923=CARTESIAN_POINT('Ctrl Pts',(23.4112391022538,-13.48036797944,5.25280074041754));
#38924=CARTESIAN_POINT('Ctrl Pts',(23.5274006995054,-13.4704404449522,5.27931561824266));
#38925=CARTESIAN_POINT('Ctrl Pts',(23.75869759757,-13.4509289072634,5.3306297071107));
#38926=CARTESIAN_POINT('Ctrl Pts',(24.1668938536999,-13.4171810922989,5.41708560365397));
#38927=CARTESIAN_POINT('Ctrl Pts',(24.7548128660958,-13.3713845002052,5.52956305821883));
#38928=CARTESIAN_POINT('Ctrl Pts',(25.3473131502197,-13.3310219589392,5.62567073595883));
#38929=CARTESIAN_POINT('Ctrl Pts',(25.8218041556281,-13.3034028562425,5.69154378511353));
#38930=CARTESIAN_POINT('Ctrl Pts',(26.0589587666352,-13.2913640661324,5.72065900880548));
#38931=CARTESIAN_POINT('Ctrl Pts',(26.6316948383761,-13.2646759506016,5.78623492045644));
#38932=CARTESIAN_POINT('Ctrl Pts',(27.5576851463966,-13.236440987388,5.85186367837989));
#38933=CARTESIAN_POINT('Ctrl Pts',(28.5507795710394,-13.2219159498841,5.88219883517421));
#38934=CARTESIAN_POINT('Ctrl Pts',(29.1361849357887,-13.2135466774645,5.90128718803104));
#38935=CARTESIAN_POINT('Ctrl Pts',(29.2912521292177,-13.211632738116,5.90574282943922));
#38936=CARTESIAN_POINT('Ctrl Pts',(29.6100275770339,-13.2086893874642,5.91253309751288));
#38937=CARTESIAN_POINT('Ctrl Pts',(30.1692894984413,-13.2059721234291,5.91881362945886));
#38938=CARTESIAN_POINT('Ctrl Pts',(31.3098805820073,-13.2079309635128,5.91428725204102));
#38939=CARTESIAN_POINT('Ctrl Pts',(32.3163182251692,-13.215170536538,5.89785677449482));
#38940=CARTESIAN_POINT('Ctrl Pts',(33.1686695899412,-13.2151857432769,5.89783797451692));
#38941=CARTESIAN_POINT('Ctrl Pts',(33.4952713010558,-13.2151875891279,5.89783593918779));
#38942=CARTESIAN_POINT('Ctrl Pts',(34.1548283685118,-13.2151907586342,5.8978321735044));
#38943=CARTESIAN_POINT('Ctrl Pts',(34.9764778638342,-13.2152010495211,5.89782019909883));
#38944=CARTESIAN_POINT('Ctrl Pts',(35.9641101124161,-13.2152053506642,5.89781516246843));
#38945=CARTESIAN_POINT('Ctrl Pts',(37.9386244259607,-13.2152112104218,5.89780833274506));
#38946=CARTESIAN_POINT('Ctrl Pts',(39.5833333333333,-13.2152418049849,5.89777260594516));
#38947=CARTESIAN_POINT('Ctrl Pts',(40.9,-13.2152418049849,5.89777260594516));
#38948=CARTESIAN_POINT('Ctrl Pts',(6.84649785567288,-21.377211306072,-6.71741536412573));
#38949=CARTESIAN_POINT('Ctrl Pts',(7.61279643984166,-21.7222003209083,-5.59224351411651));
#38950=CARTESIAN_POINT('Ctrl Pts',(8.41290239278216,-21.9819683115275,-4.4778139915129));
#38951=CARTESIAN_POINT('Ctrl Pts',(10.1883118359637,-22.351694214315,-2.12504829883047));
#38952=CARTESIAN_POINT('Ctrl Pts',(11.1645908932198,-22.4195115822635,-0.860235293933496));
#38953=CARTESIAN_POINT('Ctrl Pts',(13.104616539894,-22.4060524143024,1.36442582505286));
#38954=CARTESIAN_POINT('Ctrl Pts',(14.0814329274866,-22.2982732069865,2.43568052201622));
#38955=CARTESIAN_POINT('Ctrl Pts',(15.9946796213894,-22.0394507048972,4.24582169215594));
#38956=CARTESIAN_POINT('Ctrl Pts',(16.9653275559585,-21.84127820419,5.10151618176833));
#38957=CARTESIAN_POINT('Ctrl Pts',(18.8448710605557,-21.4842569534398,6.49486940232067));
#38958=CARTESIAN_POINT('Ctrl Pts',(19.8101236302159,-21.2634255374822,7.14150804350577));
#38959=CARTESIAN_POINT('Ctrl Pts',(20.9856903475787,-21.0426589820635,7.78021164720302));
#38960=CARTESIAN_POINT('Ctrl Pts',(21.4500377829479,-20.9532273635236,8.0234729107848));
#38961=CARTESIAN_POINT('Ctrl Pts',(22.3710393802638,-20.7788884454096,8.46623345546781));
#38962=CARTESIAN_POINT('Ctrl Pts',(23.0719693188992,-20.6575298272077,8.75491470148121));
#38963=CARTESIAN_POINT('Ctrl Pts',(23.5926347936586,-20.5813719818061,8.94023465873173));
#38964=CARTESIAN_POINT('Ctrl Pts',(23.7065892332644,-20.5647099449239,8.98001571960571));
#38965=CARTESIAN_POINT('Ctrl Pts',(23.9323706520527,-20.5321468576875,9.0566499549595));
#38966=CARTESIAN_POINT('Ctrl Pts',(24.3307466212143,-20.4759485784751,9.1857404907663));
#38967=CARTESIAN_POINT('Ctrl Pts',(24.9023508233185,-20.4001844372317,9.35309964749801));
#38968=CARTESIAN_POINT('Ctrl Pts',(25.4757972573111,-20.3338472412531,9.49555868076779));
#38969=CARTESIAN_POINT('Ctrl Pts',(25.9330914993694,-20.28864648982,9.59288697707771));
#38970=CARTESIAN_POINT('Ctrl Pts',(26.1609781823311,-20.2689918009898,9.63581705245677));
#38971=CARTESIAN_POINT('Ctrl Pts',(26.709932241435,-20.2254900271807,9.73235004955936));
#38972=CARTESIAN_POINT('Ctrl Pts',(27.5959509089719,-20.1795241403997,9.82915847887795));
#38973=CARTESIAN_POINT('Ctrl Pts',(28.579749560637,-20.155272253243,9.87532060641945));
#38974=CARTESIAN_POINT('Ctrl Pts',(29.1657855350677,-20.1412111689925,9.90441669946595));
#38975=CARTESIAN_POINT('Ctrl Pts',(29.3146731630637,-20.1381027603739,9.91097811975321));
#38976=CARTESIAN_POINT('Ctrl Pts',(29.6257300067643,-20.1332492263269,9.92113271524804));
#38977=CARTESIAN_POINT('Ctrl Pts',(30.1719452394076,-20.1287785103479,9.93050366138696));
#38978=CARTESIAN_POINT('Ctrl Pts',(31.2977811219682,-20.1319916124711,9.92376874726301));
#38979=CARTESIAN_POINT('Ctrl Pts',(32.306925911767,-20.1442225454146,9.8985708956696));
#38980=CARTESIAN_POINT('Ctrl Pts',(33.1709940314752,-20.1442592438603,9.89851679451552));
#38981=CARTESIAN_POINT('Ctrl Pts',(33.4961680489761,-20.1442637388651,9.89851046735387));
#38982=CARTESIAN_POINT('Ctrl Pts',(34.1564024558335,-20.1442714128624,9.89849933968833));
#38983=CARTESIAN_POINT('Ctrl Pts',(34.9773378017947,-20.1442963704308,9.89846345509219));
#38984=CARTESIAN_POINT('Ctrl Pts',(35.9650395265661,-20.1443067963913,9.89844842592582));
#38985=CARTESIAN_POINT('Ctrl Pts',(37.9392783163648,-20.1443210056784,9.8984279817608));
#38986=CARTESIAN_POINT('Ctrl Pts',(39.5833333333333,-20.1443951831047,9.89832117405885));
#38987=CARTESIAN_POINT('Ctrl Pts',(40.9,-20.1443951831047,9.89832117405885));
#38988=CARTESIAN_POINT('Ctrl Pts',(6.90857970435319,-29.1272609852091,-8.7101858572574));
#38989=CARTESIAN_POINT('Ctrl Pts',(7.67983757144493,-29.5775536996439,-7.16260494418019));
#38990=CARTESIAN_POINT('Ctrl Pts',(8.48457055999567,-29.9097225030882,-5.63283520142948));
#38991=CARTESIAN_POINT('Ctrl Pts',(10.2689932185249,-30.3644487697131,-2.41146069737717));
#38992=CARTESIAN_POINT('Ctrl Pts',(11.2491988139072,-30.4296414097155,-0.683672158318401));
#38993=CARTESIAN_POINT('Ctrl Pts',(13.2074449203971,-30.3576235761244,2.36894751212039));
#38994=CARTESIAN_POINT('Ctrl Pts',(14.1878085217557,-30.184965998838,3.82665309566743));
#38995=CARTESIAN_POINT('Ctrl Pts',(16.1228140255812,-29.7814752498472,6.30658851121945));
#38996=CARTESIAN_POINT('Ctrl Pts',(17.0983171044692,-29.4886591763938,7.46839135174002));
#38997=CARTESIAN_POINT('Ctrl Pts',(18.9977376700381,-28.960082872958,9.36704911481261));
#38998=CARTESIAN_POINT('Ctrl Pts',(19.9674462816337,-28.6415548808293,10.2409515663328));
#38999=CARTESIAN_POINT('Ctrl Pts',(21.1471060032309,-28.3239820751165,11.1004135437216));
#39000=CARTESIAN_POINT('Ctrl Pts',(21.6116736136674,-28.1962714220824,11.4272945418467));
#39001=CARTESIAN_POINT('Ctrl Pts',(22.5321107331754,-27.9485409607959,12.020283834991));
#39002=CARTESIAN_POINT('Ctrl Pts',(23.2282372947769,-27.7781185470828,12.4035528917693));
#39003=CARTESIAN_POINT('Ctrl Pts',(23.7411423015336,-27.6723004799183,12.6473785079706));
#39004=CARTESIAN_POINT('Ctrl Pts',(23.8541050059083,-27.6489722597556,12.7001926206312));
#39005=CARTESIAN_POINT('Ctrl Pts',(24.0772792343329,-27.603576753781,12.8015323632731));
#39006=CARTESIAN_POINT('Ctrl Pts',(24.4706231308706,-27.5254067801747,12.9720321690745));
#39007=CARTESIAN_POINT('Ctrl Pts',(25.0326506601034,-27.4207276483819,13.1919318242548));
#39008=CARTESIAN_POINT('Ctrl Pts',(25.5929166162092,-27.3299203180183,13.3777331675809));
#39009=CARTESIAN_POINT('Ctrl Pts',(26.036986986334,-27.2685418388,13.5038445845534));
#39010=CARTESIAN_POINT('Ctrl Pts',(26.257289284528,-27.2420133361897,13.5592118403736));
#39011=CARTESIAN_POINT('Ctrl Pts',(26.7861809172635,-27.1835476308027,13.6833062419416));
#39012=CARTESIAN_POINT('Ctrl Pts',(27.6340630276978,-27.1220525704358,13.8074117592232));
#39013=CARTESIAN_POINT('Ctrl Pts',(28.6084466264574,-27.0881176443602,13.8693290201703));
#39014=CARTESIAN_POINT('Ctrl Pts',(29.1951297895239,-27.0683644245336,13.908430904103));
#39015=CARTESIAN_POINT('Ctrl Pts',(29.3379067795074,-27.0642236253566,13.9168171018367));
#39016=CARTESIAN_POINT('Ctrl Pts',(29.6412852452592,-27.0575993546201,13.9300946799831));
#39017=CARTESIAN_POINT('Ctrl Pts',(30.1744790744102,-27.0515191755617,13.9423073235085));
#39018=CARTESIAN_POINT('Ctrl Pts',(31.285567721335,-27.0558675796336,13.933569334585));
#39019=CARTESIAN_POINT('Ctrl Pts',(32.2974599236722,-27.0731946134563,13.8994232817537));
#39020=CARTESIAN_POINT('Ctrl Pts',(33.1732579076352,-27.0732696672436,13.8993047075201));
#39021=CARTESIAN_POINT('Ctrl Pts',(33.4970065888605,-27.0732789151667,13.8992904506871));
#39022=CARTESIAN_POINT('Ctrl Pts',(34.1579215418455,-27.0732946436725,13.8992658208367));
#39023=CARTESIAN_POINT('Ctrl Pts',(34.9781539333149,-27.0733458523266,13.8991859907804));
#39024=CARTESIAN_POINT('Ctrl Pts',(35.9659297143336,-27.0733672375489,13.8991526077107));
#39025=CARTESIAN_POINT('Ctrl Pts',(37.9398993196362,-27.0733963900547,13.8991071452309));
#39026=CARTESIAN_POINT('Ctrl Pts',(39.5833333333333,-27.0735485612246,13.8988697421725));
#39027=CARTESIAN_POINT('Ctrl Pts',(40.9,-27.0735485612246,13.8988697421725));
#39028=CARTESIAN_POINT('Ctrl Pts',(6.93528330520032,-33.5512413216408,-9.86563481868489));
#39029=CARTESIAN_POINT('Ctrl Pts',(7.70864561497005,-34.0623374960229,-8.07765806999139));
#39030=CARTESIAN_POINT('Ctrl Pts',(8.51541871352369,-34.4367698578613,-6.31093086144101));
#39031=CARTESIAN_POINT('Ctrl Pts',(10.3035747340621,-34.941954951338,-2.59403255178488));
#39032=CARTESIAN_POINT('Ctrl Pts',(11.2855474597114,-35.0067705115655,-0.601863607331424));
#39033=CARTESIAN_POINT('Ctrl Pts',(13.2510271399958,-34.9032893217431,2.92382891559037));
#39034=CARTESIAN_POINT('Ctrl Pts',(14.2329608248363,-34.6945593989858,4.60257161238985));
#39035=CARTESIAN_POINT('Ctrl Pts',(16.1768697182175,-34.2095752766376,7.46747574760142));
#39036=CARTESIAN_POINT('Ctrl Pts',(17.1545233971705,-33.863251175018,8.80499374792142));
#39037=CARTESIAN_POINT('Ctrl Pts',(19.0635787323924,-33.2359528227277,10.9976618314205));
#39038=CARTESIAN_POINT('Ctrl Pts',(20.0357940514507,-32.8613840028834,12.0029926013879));
#39039=CARTESIAN_POINT('Ctrl Pts',(21.2200273744511,-32.4867165469276,12.9932317593815));
#39040=CARTESIAN_POINT('Ctrl Pts',(21.6852779128344,-32.3368305207217,13.3687144259959));
#39041=CARTESIAN_POINT('Ctrl Pts',(22.6074094382987,-32.0460468583651,14.0501505350056));
#39042=CARTESIAN_POINT('Ctrl Pts',(23.303404556016,-31.8467199720656,14.4891819334101));
#39043=CARTESIAN_POINT('Ctrl Pts',(23.8143672767891,-31.7234333079366,14.7674149360666));
#39044=CARTESIAN_POINT('Ctrl Pts',(23.9270724954075,-31.6962311639846,14.8277950271988));
#39045=CARTESIAN_POINT('Ctrl Pts',(24.1495225469484,-31.6433583861176,14.9435144746797));
#39046=CARTESIAN_POINT('Ctrl Pts',(24.5413305977736,-31.5524212197087,15.1380475804187));
#39047=CARTESIAN_POINT('Ctrl Pts',(25.0999889357199,-31.4310156375917,15.3882930140602));
#39048=CARTESIAN_POINT('Ctrl Pts',(25.6548568854792,-31.3262265443364,15.5988027583032));
#39049=CARTESIAN_POINT('Ctrl Pts',(26.0929602492094,-31.2557376661541,15.741087693316));
#39050=CARTESIAN_POINT('Ctrl Pts',(26.3096479269533,-31.2253935968531,15.8033473177939));
#39051=CARTESIAN_POINT('Ctrl Pts',(26.8287121638341,-31.1587088311854,15.9425694431084));
#39052=CARTESIAN_POINT('Ctrl Pts',(27.6557884297532,-31.0890012981156,16.0810926132799));
#39053=CARTESIAN_POINT('Ctrl Pts',(28.624709126668,-31.0495586097517,16.1519656805034));
#39054=CARTESIAN_POINT('Ctrl Pts',(29.2117706203409,-31.0265558099781,16.1967753671696));
#39055=CARTESIAN_POINT('Ctrl Pts',(29.351092195488,-31.021876437373,16.2061151113191));
#39056=CARTESIAN_POINT('Ctrl Pts',(29.6501043905816,-31.014285796168,16.2210980111665));
#39057=CARTESIAN_POINT('Ctrl Pts',(30.175870201979,-31.0073340046886,16.2348498398373));
#39058=CARTESIAN_POINT('Ctrl Pts',(31.278535210342,-31.0122942956317,16.2250286703999));
#39059=CARTESIAN_POINT('Ctrl Pts',(32.2920164760145,-31.0325718136052,16.1856975481828));
#39060=CARTESIAN_POINT('Ctrl Pts',(33.174523274163,-31.0326760798738,16.1855272745483));
#39061=CARTESIAN_POINT('Ctrl Pts',(33.4974585875216,-31.0326890056742,16.1855064782319));
#39062=CARTESIAN_POINT('Ctrl Pts',(34.158763915549,-31.0327109045834,16.1854709093049));
#39063=CARTESIAN_POINT('Ctrl Pts',(34.9785998474407,-31.0327822824583,16.1853552918984));
#39064=CARTESIAN_POINT('Ctrl Pts',(35.9664200829455,-31.0328120805002,16.1853069853609));
#39065=CARTESIAN_POINT('Ctrl Pts',(37.9402388284556,-31.0328527115371,16.185241157271));
#39066=CARTESIAN_POINT('Ctrl Pts',(39.5833333333333,-31.033064777293,16.1848974953804));
#39067=CARTESIAN_POINT('Ctrl Pts',(40.9,-31.033064777293,16.1848974953804));
#39068=CARTESIAN_POINT('Origin',(6.9,-15.,25.9807621135332));
#39069=CARTESIAN_POINT('',(6.9,-29.194404870986,6.90555748864273));
#39070=CARTESIAN_POINT('Ctrl Pts',(6.9,-10.8594625780008,1.92623027574191));
#39071=CARTESIAN_POINT('Ctrl Pts',(6.9,-14.5482083700348,3.00887228147899));
#39072=CARTESIAN_POINT('Ctrl Pts',(6.90000000166257,-18.4565659967827,4.07058553003038));
#39073=CARTESIAN_POINT('Ctrl Pts',(6.90000000166257,-24.1072623232988,5.57797815223758));
#39074=CARTESIAN_POINT('Ctrl Pts',(6.9,-26.6663167664834,6.24902093139924));
#39075=CARTESIAN_POINT('Ctrl Pts',(6.9,-29.194404870986,6.90555748864272));
#39076=CARTESIAN_POINT('Origin',(6.9,0.,0.));
#39077=CARTESIAN_POINT('Origin',(40.9,-4.5,7.79422863405995));
#39078=CARTESIAN_POINT('Ctrl Pts',(40.9,-18.5327260452907,29.0996231131986));
#39079=CARTESIAN_POINT('Ctrl Pts',(40.9,-18.2824786427117,28.6661818974695));
#39080=CARTESIAN_POINT('Ctrl Pts',(40.9,-18.0322312401326,28.2327406817405));
#39081=CARTESIAN_POINT('Ctrl Pts',(40.9,-17.7819838375536,27.7992994660114));
#39082=CARTESIAN_POINT('Ctrl Pts',(30.5,-16.1306417505986,31.061268433756));
#39083=CARTESIAN_POINT('Ctrl Pts',(30.5,-16.823692245373,30.7013555966443));
#39084=CARTESIAN_POINT('Ctrl Pts',(30.5,-17.5,30.3108891324554));
#39085=CARTESIAN_POINT('Ctrl Pts',(30.5,-47.8108891324553,12.8108891324554));
#39086=CARTESIAN_POINT('Ctrl Pts',(30.5,-30.3108891324554,-17.5));
#39087=CARTESIAN_POINT('Ctrl Pts',(30.5,-12.8108891324554,-47.8108891324553));
#39088=CARTESIAN_POINT('Ctrl Pts',(30.5,17.5,-30.3108891324554));
#39089=CARTESIAN_POINT('Ctrl Pts',(30.5,47.8108891324553,-12.8108891324554));
#39090=CARTESIAN_POINT('Ctrl Pts',(30.5,30.3108891324554,17.5));
#39091=CARTESIAN_POINT('Ctrl Pts',(30.5,13.5747778926489,46.4877949884694));
#39092=CARTESIAN_POINT('Ctrl Pts',(30.5,-16.1306417505986,31.061268433756));
#39093=CARTESIAN_POINT('Ctrl Pts',(30.3311478274255,-16.0958729911865,30.9943174850025));
#39094=CARTESIAN_POINT('Ctrl Pts',(30.3311478274255,-16.7874296516619,30.6351804212937));
#39095=CARTESIAN_POINT('Ctrl Pts',(30.3311478274255,-17.4622796600955,30.245555587262));
#39096=CARTESIAN_POINT('Ctrl Pts',(30.3311478274255,-47.7078352473574,12.7832759271665));
#39097=CARTESIAN_POINT('Ctrl Pts',(30.3311478274255,-30.245555587262,-17.4622796600955));
#39098=CARTESIAN_POINT('Ctrl Pts',(30.3311478274255,-12.7832759271665,-47.7078352473574));
#39099=CARTESIAN_POINT('Ctrl Pts',(30.3311478274255,17.4622796600955,-30.245555587262));
#39100=CARTESIAN_POINT('Ctrl Pts',(30.3311478274255,47.7078352473574,-12.7832759271665));
#39101=CARTESIAN_POINT('Ctrl Pts',(30.3311478274255,30.245555587262,17.4622796600955));
#39102=CARTESIAN_POINT('Ctrl Pts',(30.3311478274255,13.5455181648638,46.3875929639907));
#39103=CARTESIAN_POINT('Ctrl Pts',(30.3311478274255,-16.0958729911865,30.9943174850025));
#39104=CARTESIAN_POINT('Ctrl Pts',(29.9897712690917,-16.0254447695752,30.8587004444282));
#39105=CARTESIAN_POINT('Ctrl Pts',(29.9897712690917,-16.7139754925468,30.501134801215));
#39106=CARTESIAN_POINT('Ctrl Pts',(29.9897712690917,-17.3858726641896,30.1132147882992));
#39107=CARTESIAN_POINT('Ctrl Pts',(29.9897712690917,-47.4990874524888,12.7273421241097));
#39108=CARTESIAN_POINT('Ctrl Pts',(29.9897712690917,-30.1132147882992,-17.3858726641896));
#39109=CARTESIAN_POINT('Ctrl Pts',(29.9897712690917,-12.7273421241097,-47.4990874524888));
#39110=CARTESIAN_POINT('Ctrl Pts',(29.9897712690917,17.3858726641896,-30.1132147882992));
#39111=CARTESIAN_POINT('Ctrl Pts',(29.9897712690917,47.4990874524888,-12.7273421241097));
#39112=CARTESIAN_POINT('Ctrl Pts',(29.9897712690917,30.1132147882992,17.3858726641896));
#39113=CARTESIAN_POINT('Ctrl Pts',(29.9897712690917,13.4862491363571,46.1846219490559));
#39114=CARTESIAN_POINT('Ctrl Pts',(29.9897712690917,-16.0254447695752,30.8587004444282));
#39115=CARTESIAN_POINT('Ctrl Pts',(29.4666899049319,-15.9171300516369,30.6501289206644));
#39116=CARTESIAN_POINT('Ctrl Pts',(29.4666899049319,-16.6010070497276,30.2949800354474));
#39117=CARTESIAN_POINT('Ctrl Pts',(29.4666899049319,-17.2683629213518,29.9096819433198));
#39118=CARTESIAN_POINT('Ctrl Pts',(29.4666899049319,-47.1780448646716,12.6413190219681));
#39119=CARTESIAN_POINT('Ctrl Pts',(29.4666899049319,-29.9096819433198,-17.2683629213518));
#39120=CARTESIAN_POINT('Ctrl Pts',(29.4666899049319,-12.6413190219681,-47.1780448646716));
#39121=CARTESIAN_POINT('Ctrl Pts',(29.4666899049319,17.2683629213518,-29.9096819433198));
#39122=CARTESIAN_POINT('Ctrl Pts',(29.4666899049319,47.1780448646716,-12.6413190219681));
#39123=CARTESIAN_POINT('Ctrl Pts',(29.4666899049319,29.9096819433198,17.2683629213518));
#39124=CARTESIAN_POINT('Ctrl Pts',(29.4666899049319,13.3950966415431,45.8724637299593));
#39125=CARTESIAN_POINT('Ctrl Pts',(29.4666899049319,-15.9171300516369,30.6501289206644));
#39126=CARTESIAN_POINT('Ctrl Pts',(28.7471241621752,-15.7673462336858,30.3617042288049));
#39127=CARTESIAN_POINT('Ctrl Pts',(28.7471241621752,-16.4447877935127,30.0098973754615));
#39128=CARTESIAN_POINT('Ctrl Pts',(28.7471241621752,-17.105863694435,29.6282250261092));
#39129=CARTESIAN_POINT('Ctrl Pts',(28.7471241621752,-46.7340887205442,12.5223613316743));
#39130=CARTESIAN_POINT('Ctrl Pts',(28.7471241621752,-29.6282250261092,-17.105863694435));
#39131=CARTESIAN_POINT('Ctrl Pts',(28.7471241621752,-12.5223613316743,-46.7340887205442));
#39132=CARTESIAN_POINT('Ctrl Pts',(28.7471241621752,17.105863694435,-29.6282250261092));
#39133=CARTESIAN_POINT('Ctrl Pts',(28.7471241621752,46.7340887205442,-12.5223613316743));
#39134=CARTESIAN_POINT('Ctrl Pts',(28.7471241621752,29.6282250261092,17.105863694435));
#39135=CARTESIAN_POINT('Ctrl Pts',(28.7471241621752,13.2690457322218,45.4407934015768));
#39136=CARTESIAN_POINT('Ctrl Pts',(28.7471241621752,-15.7673462336858,30.3617042288049));
#39137=CARTESIAN_POINT('Ctrl Pts',(27.8100958442934,-15.5715428260696,29.9846639164451));
#39138=CARTESIAN_POINT('Ctrl Pts',(27.8100958442934,-16.2405717231752,29.6372259010587));
#39139=CARTESIAN_POINT('Ctrl Pts',(27.8100958442934,-16.8934381948013,29.2602932679205));
#39140=CARTESIAN_POINT('Ctrl Pts',(27.8100958442934,-46.1537314627218,12.3668550731192));
#39141=CARTESIAN_POINT('Ctrl Pts',(27.8100958442934,-29.2602932679205,-16.8934381948013));
#39142=CARTESIAN_POINT('Ctrl Pts',(27.8100958442934,-12.3668550731192,-46.1537314627218));
#39143=CARTESIAN_POINT('Ctrl Pts',(27.8100958442934,16.8934381948013,-29.2602932679205));
#39144=CARTESIAN_POINT('Ctrl Pts',(27.8100958442934,46.1537314627218,-12.3668550731192));
#39145=CARTESIAN_POINT('Ctrl Pts',(27.8100958442934,29.2602932679205,16.8934381948013));
#39146=CARTESIAN_POINT('Ctrl Pts',(27.8100958442934,13.1042669335782,44.8764966543029));
#39147=CARTESIAN_POINT('Ctrl Pts',(27.8100958442934,-15.5715428260696,29.9846639164451));
#39148=CARTESIAN_POINT('Ctrl Pts',(26.8343111708818,-15.3685420031368,29.5937642144445));
#39149=CARTESIAN_POINT('Ctrl Pts',(26.8343111708818,-16.0288490017,29.2508556284042));
#39150=CARTESIAN_POINT('Ctrl Pts',(26.8343111708818,-16.6732042787395,28.8788369357517));
#39151=CARTESIAN_POINT('Ctrl Pts',(26.8343111708818,-45.5520412144912,12.2056326570122));
#39152=CARTESIAN_POINT('Ctrl Pts',(26.8343111708818,-28.8788369357517,-16.6732042787395));
#39153=CARTESIAN_POINT('Ctrl Pts',(26.8343111708818,-12.2056326570122,-45.5520412144912));
#39154=CARTESIAN_POINT('Ctrl Pts',(26.8343111708818,16.6732042787395,-28.8788369357517));
#39155=CARTESIAN_POINT('Ctrl Pts',(26.8343111708818,45.5520412144912,-12.2056326570122));
#39156=CARTESIAN_POINT('Ctrl Pts',(26.8343111708818,28.8788369357517,16.6732042787395));
#39157=CARTESIAN_POINT('Ctrl Pts',(26.8343111708818,12.9334311338658,44.2914572749094));
#39158=CARTESIAN_POINT('Ctrl Pts',(26.8343111708818,-15.3685420031368,29.5937642144445));
#39159=CARTESIAN_POINT('Ctrl Pts',(25.8181479469611,-15.1612099270726,29.1945242233064));
#39160=CARTESIAN_POINT('Ctrl Pts',(25.8181479469611,-15.8126089354813,28.8562417071321));
#39161=CARTESIAN_POINT('Ctrl Pts',(25.8181479469611,-16.4482714219305,28.4892417994669));
#39162=CARTESIAN_POINT('Ctrl Pts',(25.8181479469611,-44.9375132213974,12.0409703775363));
#39163=CARTESIAN_POINT('Ctrl Pts',(25.8181479469611,-28.4892417994669,-16.4482714219305));
#39164=CARTESIAN_POINT('Ctrl Pts',(25.8181479469611,-12.0409703775363,-44.9375132213974));
#39165=CARTESIAN_POINT('Ctrl Pts',(25.8181479469611,16.4482714219305,-28.4892417994669));
#39166=CARTESIAN_POINT('Ctrl Pts',(25.8181479469611,44.9375132213974,-12.0409703775363));
#39167=CARTESIAN_POINT('Ctrl Pts',(25.8181479469611,28.4892417994669,16.4482714219305));
#39168=CARTESIAN_POINT('Ctrl Pts',(25.8181479469611,12.7589503583263,43.6939354158518));
#39169=CARTESIAN_POINT('Ctrl Pts',(25.8181479469611,-15.1612099270726,29.1945242233064));
#39170=CARTESIAN_POINT('Ctrl Pts',(24.7595197917227,-14.9547233834603,28.796912394945));
#39171=CARTESIAN_POINT('Ctrl Pts',(24.7595197917227,-15.5972507298839,28.4632370828042));
#39172=CARTESIAN_POINT('Ctrl Pts',(24.7595197917227,-16.2242558762949,28.1012354927406));
#39173=CARTESIAN_POINT('Ctrl Pts',(24.7595197917227,-44.3254913690355,11.8769796164458));
#39174=CARTESIAN_POINT('Ctrl Pts',(24.7595197917227,-28.1012354927406,-16.2242558762949));
#39175=CARTESIAN_POINT('Ctrl Pts',(24.7595197917227,-11.8769796164458,-44.3254913690355));
#39176=CARTESIAN_POINT('Ctrl Pts',(24.7595197917227,16.2242558762949,-28.1012354927406));
#39177=CARTESIAN_POINT('Ctrl Pts',(24.7595197917227,44.3254913690355,-11.8769796164458));
#39178=CARTESIAN_POINT('Ctrl Pts',(24.7595197917227,28.1012354927406,16.2242558762949));
#39179=CARTESIAN_POINT('Ctrl Pts',(24.7595197917227,12.5851811425261,43.0988503438666));
#39180=CARTESIAN_POINT('Ctrl Pts',(24.7595197917227,-14.9547233834603,28.796912394945));
#39181=CARTESIAN_POINT('Ctrl Pts',(23.6563574780851,-14.7559082828157,28.4140727469455));
#39182=CARTESIAN_POINT('Ctrl Pts',(23.6563574780851,-15.389893569599,28.084833470769));
#39183=CARTESIAN_POINT('Ctrl Pts',(23.6563574780851,-16.0085630157705,27.7276444994825));
#39184=CARTESIAN_POINT('Ctrl Pts',(23.6563574780851,-43.736207515253,11.7190814837121));
#39185=CARTESIAN_POINT('Ctrl Pts',(23.6563574780851,-27.7276444994825,-16.0085630157705));
#39186=CARTESIAN_POINT('Ctrl Pts',(23.6563574780851,-11.7190814837121,-43.736207515253));
#39187=CARTESIAN_POINT('Ctrl Pts',(23.6563574780851,16.0085630157705,-27.7276444994825));
#39188=CARTESIAN_POINT('Ctrl Pts',(23.6563574780851,43.736207515253,-11.7190814837121));
#39189=CARTESIAN_POINT('Ctrl Pts',(23.6563574780851,27.7276444994825,16.0085630157705));
#39190=CARTESIAN_POINT('Ctrl Pts',(23.6563574780851,12.4178678468319,42.5258740306932));
#39191=CARTESIAN_POINT('Ctrl Pts',(23.6563574780851,-14.7559082828157,28.4140727469455));
#39192=CARTESIAN_POINT('Ctrl Pts',(22.5073180101405,-14.5719314169357,28.0598057001003));
#39193=CARTESIAN_POINT('Ctrl Pts',(22.5073180101405,-15.1980121665098,27.7346713837132));
#39194=CARTESIAN_POINT('Ctrl Pts',(22.5073180101405,-15.8089680335819,27.3819358493961));
#39195=CARTESIAN_POINT('Ctrl Pts',(22.5073180101405,-43.190903882978,11.5729678158142));
#39196=CARTESIAN_POINT('Ctrl Pts',(22.5073180101405,-27.3819358493961,-15.8089680335819));
#39197=CARTESIAN_POINT('Ctrl Pts',(22.5073180101405,-11.5729678158142,-43.190903882978));
#39198=CARTESIAN_POINT('Ctrl Pts',(22.5073180101405,15.8089680335819,-27.3819358493961));
#39199=CARTESIAN_POINT('Ctrl Pts',(22.5073180101405,43.190903882978,-11.5729678158142));
#39200=CARTESIAN_POINT('Ctrl Pts',(22.5073180101405,27.3819358493961,15.8089680335819));
#39201=CARTESIAN_POINT('Ctrl Pts',(22.5073180101405,12.2630417010206,41.9956608528241));
#39202=CARTESIAN_POINT('Ctrl Pts',(22.5073180101405,-14.5719314169357,28.0598057001003));
#39203=CARTESIAN_POINT('Ctrl Pts',(21.3125219557939,-14.4091508971893,27.7463544749225));
#39204=CARTESIAN_POINT('Ctrl Pts',(21.3125219557939,-15.0282378072439,27.4248521776202));
#39205=CARTESIAN_POINT('Ctrl Pts',(21.3125219557939,-15.632368792237,27.0760569908086));
#39206=CARTESIAN_POINT('Ctrl Pts',(21.3125219557939,-42.7084257830456,11.4436881985716));
#39207=CARTESIAN_POINT('Ctrl Pts',(21.3125219557939,-27.0760569908086,-15.632368792237));
#39208=CARTESIAN_POINT('Ctrl Pts',(21.3125219557939,-11.4436881985716,-42.7084257830456));
#39209=CARTESIAN_POINT('Ctrl Pts',(21.3125219557939,15.632368792237,-27.0760569908086));
#39210=CARTESIAN_POINT('Ctrl Pts',(21.3125219557939,42.7084257830456,-11.4436881985716));
#39211=CARTESIAN_POINT('Ctrl Pts',(21.3125219557939,27.0760569908086,15.632368792237));
#39212=CARTESIAN_POINT('Ctrl Pts',(21.3125219557939,12.1260533880339,41.5265346055806));
#39213=CARTESIAN_POINT('Ctrl Pts',(21.3125219557939,-14.4091508971893,27.7463544749225));
#39214=CARTESIAN_POINT('Ctrl Pts',(20.0742472323676,-14.2719922102254,27.4822408172221));
#39215=CARTESIAN_POINT('Ctrl Pts',(20.0742472323676,-14.8851861187906,27.1637988552073));
#39216=CARTESIAN_POINT('Ctrl Pts',(20.0742472323676,-15.4835664656477,26.8183238008716));
#39217=CARTESIAN_POINT('Ctrl Pts',(20.0742472323676,-42.3018902665193,11.3347573352238));
#39218=CARTESIAN_POINT('Ctrl Pts',(20.0742472323676,-26.8183238008716,-15.4835664656477));
#39219=CARTESIAN_POINT('Ctrl Pts',(20.0742472323676,-11.3347573352238,-42.3018902665193));
#39220=CARTESIAN_POINT('Ctrl Pts',(20.0742472323676,15.4835664656477,-26.8183238008716));
#39221=CARTESIAN_POINT('Ctrl Pts',(20.0742472323676,42.3018902665193,-11.3347573352238));
#39222=CARTESIAN_POINT('Ctrl Pts',(20.0742472323676,26.8183238008716,15.4835664656477));
#39223=CARTESIAN_POINT('Ctrl Pts',(20.0742472323676,12.0106271861277,41.1312493454498));
#39224=CARTESIAN_POINT('Ctrl Pts',(20.0742472323676,-14.2719922102254,27.4822408172221));
#39225=CARTESIAN_POINT('Ctrl Pts',(18.7979917002302,-14.1614724492006,27.2694232481814));
#39226=CARTESIAN_POINT('Ctrl Pts',(18.7979917002302,-14.7699178935542,26.9534472438987));
#39227=CARTESIAN_POINT('Ctrl Pts',(18.7979917002302,-15.3636644897785,26.6106474867381));
#39228=CARTESIAN_POINT('Ctrl Pts',(18.7979917002302,-41.9743119765166,11.2469829969596));
#39229=CARTESIAN_POINT('Ctrl Pts',(18.7979917002302,-26.6106474867381,-15.3636644897785));
#39230=CARTESIAN_POINT('Ctrl Pts',(18.7979917002302,-11.2469829969596,-41.9743119765166));
#39231=CARTESIAN_POINT('Ctrl Pts',(18.7979917002302,15.3636644897785,-26.6106474867381));
#39232=CARTESIAN_POINT('Ctrl Pts',(18.7979917002302,41.9743119765166,-11.2469829969596));
#39233=CARTESIAN_POINT('Ctrl Pts',(18.7979917002302,26.6106474867381,15.3636644897785));
#39234=CARTESIAN_POINT('Ctrl Pts',(18.7979917002302,11.9176190323383,40.8127362898543));
#39235=CARTESIAN_POINT('Ctrl Pts',(18.7979917002302,-14.1614724492006,27.2694232481814));
#39236=CARTESIAN_POINT('Ctrl Pts',(17.4917404060759,-14.0757116526895,27.1042817018803));
#39237=CARTESIAN_POINT('Ctrl Pts',(17.4917404060759,-14.6804723978617,26.7902192241678));
#39238=CARTESIAN_POINT('Ctrl Pts',(17.4917404060759,-15.2706233100072,26.4494954361781));
#39239=CARTESIAN_POINT('Ctrl Pts',(17.4917404060759,-41.7201187461852,11.1788721261709));
#39240=CARTESIAN_POINT('Ctrl Pts',(17.4917404060759,-26.4494954361781,-15.2706233100072));
#39241=CARTESIAN_POINT('Ctrl Pts',(17.4917404060759,-11.1788721261709,-41.7201187461852));
#39242=CARTESIAN_POINT('Ctrl Pts',(17.4917404060759,15.2706233100072,-26.4494954361781));
#39243=CARTESIAN_POINT('Ctrl Pts',(17.4917404060759,41.7201187461852,-11.1788721261709));
#39244=CARTESIAN_POINT('Ctrl Pts',(17.4917404060759,26.4494954361781,15.2706233100072));
#39245=CARTESIAN_POINT('Ctrl Pts',(17.4917404060759,11.8454468408945,40.5655774732432));
#39246=CARTESIAN_POINT('Ctrl Pts',(17.4917404060759,-14.0757116526895,27.1042817018803));
#39247=CARTESIAN_POINT('Ctrl Pts',(16.1647270995715,-14.011024902894,26.9797204766935));
#39248=CARTESIAN_POINT('Ctrl Pts',(16.1647270995715,-14.6130063919992,26.6671013136366));
#39249=CARTESIAN_POINT('Ctrl Pts',(16.1647270995715,-15.2004451894511,26.3279433657953));
#39250=CARTESIAN_POINT('Ctrl Pts',(16.1647270995715,-41.5283885552464,11.1274981763442));
#39251=CARTESIAN_POINT('Ctrl Pts',(16.1647270995715,-26.3279433657953,-15.2004451894511));
#39252=CARTESIAN_POINT('Ctrl Pts',(16.1647270995715,-11.1274981763442,-41.5283885552464));
#39253=CARTESIAN_POINT('Ctrl Pts',(16.1647270995715,15.2004451894511,-26.3279433657953));
#39254=CARTESIAN_POINT('Ctrl Pts',(16.1647270995715,41.5283885552464,-11.1274981763442));
#39255=CARTESIAN_POINT('Ctrl Pts',(16.1647270995715,26.3279433657953,15.2004451894511));
#39256=CARTESIAN_POINT('Ctrl Pts',(16.1647270995715,11.7910095609247,40.3791531257526));
#39257=CARTESIAN_POINT('Ctrl Pts',(16.1647270995715,-14.011024902894,26.9797204766935));
#39258=CARTESIAN_POINT('Ctrl Pts',(14.8263876417415,-13.9627843740029,26.8868282012068));
#39259=CARTESIAN_POINT('Ctrl Pts',(14.8263876417415,-14.5626932163446,26.5752853986496));
#39260=CARTESIAN_POINT('Ctrl Pts',(14.8263876417415,-15.1481094381123,26.2372951854241));
#39261=CARTESIAN_POINT('Ctrl Pts',(14.8263876417415,-41.3854046235364,11.0891857473118));
#39262=CARTESIAN_POINT('Ctrl Pts',(14.8263876417415,-26.2372951854241,-15.1481094381123));
#39263=CARTESIAN_POINT('Ctrl Pts',(14.8263876417415,-11.0891857473118,-41.3854046235364));
#39264=CARTESIAN_POINT('Ctrl Pts',(14.8263876417415,15.1481094381123,-26.2372951854241));
#39265=CARTESIAN_POINT('Ctrl Pts',(14.8263876417415,41.3854046235364,-11.0891857473118));
#39266=CARTESIAN_POINT('Ctrl Pts',(14.8263876417415,26.2372951854241,15.1481094381123));
#39267=CARTESIAN_POINT('Ctrl Pts',(14.8263876417415,11.750412635195,40.2401260583921));
#39268=CARTESIAN_POINT('Ctrl Pts',(14.8263876417415,-13.9627843740029,26.8868282012068));
#39269=CARTESIAN_POINT('Ctrl Pts',(13.4853470903953,-13.926278703034,26.8165326442879));
#39270=CARTESIAN_POINT('Ctrl Pts',(13.4853470903953,-14.5246190849439,26.505804369746));
#39271=CARTESIAN_POINT('Ctrl Pts',(13.4853470903953,-15.1085047372063,26.1686978312363));
#39272=CARTESIAN_POINT('Ctrl Pts',(13.4853470903953,-41.2772025684426,11.0601930940301));
#39273=CARTESIAN_POINT('Ctrl Pts',(13.4853470903953,-26.1686978312363,-15.1085047372063));
#39274=CARTESIAN_POINT('Ctrl Pts',(13.4853470903953,-11.0601930940301,-41.2772025684426));
#39275=CARTESIAN_POINT('Ctrl Pts',(13.4853470903953,15.1085047372063,-26.1686978312363));
#39276=CARTESIAN_POINT('Ctrl Pts',(13.4853470903953,41.2772025684426,-11.0601930940301));
#39277=CARTESIAN_POINT('Ctrl Pts',(13.4853470903953,26.1686978312363,15.1085047372063));
#39278=CARTESIAN_POINT('Ctrl Pts',(13.4853470903953,11.7196912055776,40.1349183317465));
#39279=CARTESIAN_POINT('Ctrl Pts',(13.4853470903953,-13.926278703034,26.8165326442879));
#39280=CARTESIAN_POINT('Ctrl Pts',(12.1482076787549,-13.8976780812377,26.7614591013549));
#39281=CARTESIAN_POINT('Ctrl Pts',(12.1482076787549,-14.4947896419145,26.4513689744511));
#39282=CARTESIAN_POINT('Ctrl Pts',(12.1482076787549,-15.0774761588537,26.1149547570431));
#39283=CARTESIAN_POINT('Ctrl Pts',(12.1482076787549,-41.1924309158968,11.0374785981894));
#39284=CARTESIAN_POINT('Ctrl Pts',(12.1482076787549,-26.1149547570431,-15.0774761588537));
#39285=CARTESIAN_POINT('Ctrl Pts',(12.1482076787549,-11.0374785981894,-41.1924309158968));
#39286=CARTESIAN_POINT('Ctrl Pts',(12.1482076787549,15.0774761588537,-26.1149547570431));
#39287=CARTESIAN_POINT('Ctrl Pts',(12.1482076787549,41.1924309158968,-11.0374785981894));
#39288=CARTESIAN_POINT('Ctrl Pts',(12.1482076787549,26.1149547570431,15.0774761588537));
#39289=CARTESIAN_POINT('Ctrl Pts',(12.1482076787549,11.6956222878942,40.0524926066472));
#39290=CARTESIAN_POINT('Ctrl Pts',(12.1482076787549,-13.8976780812377,26.7614591013549));
#39291=CARTESIAN_POINT('Ctrl Pts',(10.8190675759626,-13.8744950717886,26.716817747915));
#39292=CARTESIAN_POINT('Ctrl Pts',(10.8190675759626,-14.4706105780977,26.4072448888814));
#39293=CARTESIAN_POINT('Ctrl Pts',(10.8190675759626,-15.0523251033884,26.0713918511132));
#39294=CARTESIAN_POINT('Ctrl Pts',(10.8190675759626,-41.1237169545017,11.0190667477248));
#39295=CARTESIAN_POINT('Ctrl Pts',(10.8190675759626,-26.0713918511132,-15.0523251033884));
#39296=CARTESIAN_POINT('Ctrl Pts',(10.8190675759626,-11.0190667477248,-41.1237169545017));
#39297=CARTESIAN_POINT('Ctrl Pts',(10.8190675759626,15.0523251033884,-26.0713918511132));
#39298=CARTESIAN_POINT('Ctrl Pts',(10.8190675759626,41.1237169545017,-11.0190667477248));
#39299=CARTESIAN_POINT('Ctrl Pts',(10.8190675759626,26.0713918511132,15.0523251033884));
#39300=CARTESIAN_POINT('Ctrl Pts',(10.8190675759626,11.6761125740823,39.9856802003493));
#39301=CARTESIAN_POINT('Ctrl Pts',(10.8190675759626,-13.8744950717886,26.716817747915));
#39302=CARTESIAN_POINT('Ctrl Pts',(9.50027713254189,-13.8551882149624,26.6796403391198));
#39303=CARTESIAN_POINT('Ctrl Pts',(9.50027713254189,-14.4504742051937,26.3704982618073));
#39304=CARTESIAN_POINT('Ctrl Pts',(9.50027713254189,-15.0313792538877,26.0351125755702));
#39305=CARTESIAN_POINT('Ctrl Pts',(9.50027713254189,-41.0664918294579,11.0037333216825));
#39306=CARTESIAN_POINT('Ctrl Pts',(9.50027713254189,-26.0351125755702,-15.0313792538877));
#39307=CARTESIAN_POINT('Ctrl Pts',(9.5002771325419,-11.0037333216825,-41.0664918294579));
#39308=CARTESIAN_POINT('Ctrl Pts',(9.5002771325419,15.0313792538877,-26.0351125755702));
#39309=CARTESIAN_POINT('Ctrl Pts',(9.5002771325419,41.0664918294579,-11.0037333216825));
#39310=CARTESIAN_POINT('Ctrl Pts',(9.50027713254189,26.0351125755702,15.0313792538877));
#39311=CARTESIAN_POINT('Ctrl Pts',(9.50027713254189,11.6598648452397,39.9300386942093));
#39312=CARTESIAN_POINT('Ctrl Pts',(9.50027713254189,-13.8551882149624,26.6796403391198));
#39313=CARTESIAN_POINT('Ctrl Pts',(8.45435372222587,-13.8422173352292,26.6546635289318));
#39314=CARTESIAN_POINT('Ctrl Pts',(8.45435372222587,-14.4369460336456,26.3458108626791));
#39315=CARTESIAN_POINT('Ctrl Pts',(8.45435372222587,-15.0173072536015,26.0107391561104));
#39316=CARTESIAN_POINT('Ctrl Pts',(8.45435372222587,-41.0280464097118,10.9934319025089));
#39317=CARTESIAN_POINT('Ctrl Pts',(8.45435372222587,-26.0107391561104,-15.0173072536015));
#39318=CARTESIAN_POINT('Ctrl Pts',(8.45435372222587,-10.9934319025089,-41.0280464097118));
#39319=CARTESIAN_POINT('Ctrl Pts',(8.45435372222587,15.0173072536015,-26.0107391561104));
#39320=CARTESIAN_POINT('Ctrl Pts',(8.45435372222587,41.0280464097118,-10.9934319025089));
#39321=CARTESIAN_POINT('Ctrl Pts',(8.45435372222587,26.0107391561104,15.0173072536015));
#39322=CARTESIAN_POINT('Ctrl Pts',(8.45435372222587,11.6489491721888,39.8926571933874));
#39323=CARTESIAN_POINT('Ctrl Pts',(8.45435372222587,-13.8422173352292,26.6546635289318));
#39324=CARTESIAN_POINT('Ctrl Pts',(7.67514864245731,-13.8337516775666,26.6383620035993));
#39325=CARTESIAN_POINT('Ctrl Pts',(7.67514864245731,-14.4281166503283,26.3296982262274));
#39326=CARTESIAN_POINT('Ctrl Pts',(7.67514864245731,-15.0081229315276,25.9948314436454));
#39327=CARTESIAN_POINT('Ctrl Pts',(7.67514864245731,-41.0029543751729,10.9867085121178));
#39328=CARTESIAN_POINT('Ctrl Pts',(7.67514864245731,-25.9948314436454,-15.0081229315276));
#39329=CARTESIAN_POINT('Ctrl Pts',(7.67514864245731,-10.9867085121178,-41.0029543751729));
#39330=CARTESIAN_POINT('Ctrl Pts',(7.67514864245731,15.0081229315276,-25.9948314436454));
#39331=CARTESIAN_POINT('Ctrl Pts',(7.67514864245731,41.0029543751729,-10.9867085121178));
#39332=CARTESIAN_POINT('Ctrl Pts',(7.67514864245731,25.9948314436454,15.0081229315276));
#39333=CARTESIAN_POINT('Ctrl Pts',(7.67514864245731,11.6418248789176,39.8682595430058));
#39334=CARTESIAN_POINT('Ctrl Pts',(7.67514864245731,-13.8337516775666,26.6383620035993));
#39335=CARTESIAN_POINT('Ctrl Pts',(7.15799654185577,-13.8286669632852,26.6285708447822));
#39336=CARTESIAN_POINT('Ctrl Pts',(7.15799654185577,-14.4228134720947,26.3200205194336));
#39337=CARTESIAN_POINT('Ctrl Pts',(7.15799654185577,-15.0026065670023,25.9852768200144));
#39338=CARTESIAN_POINT('Ctrl Pts',(7.15799654185577,-40.9878833870167,10.9826702530122));
#39339=CARTESIAN_POINT('Ctrl Pts',(7.15799654185577,-25.9852768200144,-15.0026065670023));
#39340=CARTESIAN_POINT('Ctrl Pts',(7.15799654185577,-10.9826702530122,-40.9878833870167));
#39341=CARTESIAN_POINT('Ctrl Pts',(7.15799654185577,15.0026065670023,-25.9852768200144));
#39342=CARTESIAN_POINT('Ctrl Pts',(7.15799654185577,40.9878833870167,-10.9826702530122));
#39343=CARTESIAN_POINT('Ctrl Pts',(7.15799654185577,25.9852768200144,15.0026065670023));
#39344=CARTESIAN_POINT('Ctrl Pts',(7.15799654185577,11.6375458261629,39.8536056216838));
#39345=CARTESIAN_POINT('Ctrl Pts',(7.15799654185577,-13.8286669632852,26.6285708447822));
#39346=CARTESIAN_POINT('Ctrl Pts',(6.9,-13.8262643576559,26.6239443717909));
#39347=CARTESIAN_POINT('Ctrl Pts',(6.9,-14.4203076388911,26.3154476542665));
#39348=CARTESIAN_POINT('Ctrl Pts',(6.9,-15.,25.9807621135332));
#39349=CARTESIAN_POINT('Ctrl Pts',(6.9,-40.9807621135331,10.9807621135332));
#39350=CARTESIAN_POINT('Ctrl Pts',(6.9,-25.9807621135332,-15.));
#39351=CARTESIAN_POINT('Ctrl Pts',(6.9,-10.9807621135332,-40.9807621135331));
#39352=CARTESIAN_POINT('Ctrl Pts',(6.9,15.,-25.9807621135332));
#39353=CARTESIAN_POINT('Ctrl Pts',(6.9,40.9807621135331,-10.9807621135332));
#39354=CARTESIAN_POINT('Ctrl Pts',(6.9,25.9807621135332,15.));
#39355=CARTESIAN_POINT('Ctrl Pts',(6.9,11.6355239079847,39.846681418688));
#39356=CARTESIAN_POINT('Ctrl Pts',(6.9,-13.8262643576559,26.6239443717909));
#39357=CARTESIAN_POINT('Ctrl Pts',(6.9,-29.194404870986,6.90555748864273));
#39358=CARTESIAN_POINT('Ctrl Pts',(7.85773098116326,-28.7583591297181,8.83308608050287));
#39359=CARTESIAN_POINT('Ctrl Pts',(8.88781981167334,-28.148927360677,10.6725495024415));
#39360=CARTESIAN_POINT('Ctrl Pts',(10.5914578196776,-26.9549567714738,13.4378975079049));
#39361=CARTESIAN_POINT('Ctrl Pts',(11.2365058953701,-26.4627511078989,14.4268759573926));
#39362=CARTESIAN_POINT('Ctrl Pts',(12.0558885382926,-25.8276163596339,15.5639851987506));
#39363=CARTESIAN_POINT('Ctrl Pts',(12.1875764958397,-25.7255677072203,15.7427052651201));
#39364=CARTESIAN_POINT('Ctrl Pts',(13.194901830313,-24.9407551262718,17.0880993664927));
#39365=CARTESIAN_POINT('Ctrl Pts',(14.2258982134098,-24.0748117650462,18.4224696507577));
#39366=CARTESIAN_POINT('Ctrl Pts',(18.2616480823244,-20.9914735836847,22.4465505568645));
#39367=CARTESIAN_POINT('Ctrl Pts',(21.0496416709525,-19.1084188222497,24.4970863377161));
#39368=CARTESIAN_POINT('Ctrl Pts',(25.8000196361138,-18.0798601480504,27.440416330328));
#39369=CARTESIAN_POINT('Ctrl Pts',(26.8976561124457,-18.1725012311874,27.9949084025612));
#39370=CARTESIAN_POINT('Ctrl Pts',(28.0045908801237,-18.293020318403,28.5110480063609));
#39371=CARTESIAN_POINT('Ctrl Pts',(28.5235971652406,-18.3760345677215,28.7375730360626));
#39372=CARTESIAN_POINT('Ctrl Pts',(29.0834839543824,-18.4629109750536,28.9821227669885));
#39373=CARTESIAN_POINT('Ctrl Pts',(29.1146288039499,-18.4676985487665,28.995750541561));
#39374=CARTESIAN_POINT('Ctrl Pts',(29.5949306848436,-18.5426905181125,29.2050975774362));
#39375=CARTESIAN_POINT('Ctrl Pts',(30.0492939924726,-18.6372599535756,29.3870260594868));
#39376=CARTESIAN_POINT('Ctrl Pts',(30.5,-18.7405179110273,29.559989655385));
#39377=CARTESIAN_POINT('Ctrl Pts',(6.45331003273164,-10.9133179225515,1.59669678622779));
#39378=CARTESIAN_POINT('Ctrl Pts',(7.20830533428676,-10.8283039351861,2.1627262104287));
#39379=CARTESIAN_POINT('Ctrl Pts',(7.99928962140321,-10.7080816105349,2.70879554626307));
#39380=CARTESIAN_POINT('Ctrl Pts',(9.76164489174099,-10.3736775708918,3.82718122480732));
#39381=CARTESIAN_POINT('Ctrl Pts',(10.7316587814816,-10.1362456656108,4.40082635509405));
#39382=CARTESIAN_POINT('Ctrl Pts',(12.6606926111663,-9.65961205419967,5.38563263712135));
#39383=CARTESIAN_POINT('Ctrl Pts',(13.6374431259542,-9.38360450626092,5.83915384029438));
#39384=CARTESIAN_POINT('Ctrl Pts',(14.8679539417017,-9.06165302613707,6.32358226998235));
#39385=CARTESIAN_POINT('Ctrl Pts',(15.8146186835336,-8.8086769516328,6.68453209751778));
#39386=CARTESIAN_POINT('Ctrl Pts',(16.7768279789013,-8.55011854625632,7.00516941257112));
#39387=CARTESIAN_POINT('Ctrl Pts',(18.442654946101,-8.14533972931256,7.48808598435168));
#39388=CARTESIAN_POINT('Ctrl Pts',(19.4151948753429,-7.90738588441827,7.72973898022675));
#39389=CARTESIAN_POINT('Ctrl Pts',(20.6328868119185,-7.66437297695775,7.97443640583065));
#39390=CARTESIAN_POINT('Ctrl Pts',(21.1054260060188,-7.57098863237667,8.06465516157011));
#39391=CARTESIAN_POINT('Ctrl Pts',(22.0544239964409,-7.39387592479574,8.22831938421076));
#39392=CARTESIAN_POINT('Ctrl Pts',(22.7836594350115,-7.27389266543028,8.33397294082328));
#39393=CARTESIAN_POINT('Ctrl Pts',(23.5025637456207,-7.17270583388463,8.42426711082611));
#39394=CARTESIAN_POINT('Ctrl Pts',(23.9756232708732,-7.10861034193446,8.47952646912231));
#39395=CARTESIAN_POINT('Ctrl Pts',(24.5702383273715,-7.03666681503315,8.53935462310099));
#39396=CARTESIAN_POINT('Ctrl Pts',(25.0506812637285,-6.98463603831072,8.58189400875859));
#39397=CARTESIAN_POINT('Ctrl Pts',(25.4117237717371,-6.94891133994711,8.61093616318075));
#39398=CARTESIAN_POINT('Ctrl Pts',(25.7132331301515,-6.92207219011225,8.63276690479109));
#39399=CARTESIAN_POINT('Ctrl Pts',(25.9243500189544,-6.90499555217227,8.64675417662557));
#39400=CARTESIAN_POINT('Ctrl Pts',(26.0449825351311,-6.895741659732,8.65437719289245));
#39401=CARTESIAN_POINT('Ctrl Pts',(26.1053107047437,-6.89128602190977,8.65806460962823));
#39402=CARTESIAN_POINT('Ctrl Pts',(26.5982868813563,-6.85557010312607,8.68771831234652));
#39403=CARTESIAN_POINT('Ctrl Pts',(27.5414448539119,-6.81230249083092,8.7222238682219));
#39404=CARTESIAN_POINT('Ctrl Pts',(28.5384718269748,-6.79157348079209,8.73742874004852));
#39405=CARTESIAN_POINT('Ctrl Pts',(29.1235718011012,-6.77903979219494,8.74727658763325));
#39406=CARTESIAN_POINT('Ctrl Pts',(29.281292582401,-6.77610142826291,8.74962231400058));
#39407=CARTESIAN_POINT('Ctrl Pts',(29.6033746665999,-6.77163194910168,8.75316560056408));
#39408=CARTESIAN_POINT('Ctrl Pts',(30.1682156581428,-6.76749797708627,8.75644680260451));
#39409=CARTESIAN_POINT('Ctrl Pts',(31.3151120085301,-6.77048174742394,8.75407681716344));
#39410=CARTESIAN_POINT('Ctrl Pts',(32.3203490755541,-6.78127046660758,8.7456273326708));
#39411=CARTESIAN_POINT('Ctrl Pts',(33.1676615322708,-6.78128357449781,8.7456218694399));
#39412=CARTESIAN_POINT('Ctrl Pts',(33.4948723279895,-6.78128505761796,8.74562133595171));
#39413=CARTESIAN_POINT('Ctrl Pts',(34.1541357431677,-6.78128770533522,8.74562028433969));
#39414=CARTESIAN_POINT('Ctrl Pts',(34.9760826079904,-6.78129612595841,8.7456170279898));
#39415=CARTESIAN_POINT('Ctrl Pts',(35.9636845487692,-6.78129958330353,8.74561567977431));
#39416=CARTESIAN_POINT('Ctrl Pts',(37.9383132355672,-6.7813043592495,8.745613828852));
#39417=CARTESIAN_POINT('Ctrl Pts',(39.5833333333333,-6.7813280023926,8.74560464293355));
#39418=CARTESIAN_POINT('Ctrl Pts',(40.9,-6.7813280023926,8.74560464293355));
#39419=CARTESIAN_POINT('Ctrl Pts',(6.63336813585096,-14.1980521881427,2.58998912169033));
#39420=CARTESIAN_POINT('Ctrl Pts',(7.389696336477,-14.0595388287459,3.32655463912721));
#39421=CARTESIAN_POINT('Ctrl Pts',(8.18035160561763,-13.8764440634215,4.03465273479121));
#39422=CARTESIAN_POINT('Ctrl Pts',(9.94163143861871,-13.3869575789582,5.47986851886094));
#39423=CARTESIAN_POINT('Ctrl Pts',(10.9109664605569,-13.0495988183286,6.21859686207519));
#39424=CARTESIAN_POINT('Ctrl Pts',(12.8334013836927,-12.3824387994051,7.47915893423736));
#39425=CARTESIAN_POINT('Ctrl Pts',(13.8089179831182,-12.0008911509523,8.05904353786122));
#39426=CARTESIAN_POINT('Ctrl Pts',(15.0306778911273,-11.5604290689694,8.67329495695322));
#39427=CARTESIAN_POINT('Ctrl Pts',(15.9745670647922,-11.2141745075895,9.13243737556315));
#39428=CARTESIAN_POINT('Ctrl Pts',(16.929544084173,-10.8635736365946,9.53704617981306));
#39429=CARTESIAN_POINT('Ctrl Pts',(18.5792362231986,-10.3171018918725,10.1451076803253));
#39430=CARTESIAN_POINT('Ctrl Pts',(19.5469773926758,-9.99640408637921,10.4493242965117));
#39431=CARTESIAN_POINT('Ctrl Pts',(20.7474295734277,-9.67172058444866,10.7549000186161));
#39432=CARTESIAN_POINT('Ctrl Pts',(21.2167794172895,-9.54637190554481,10.8681544802447));
#39433=CARTESIAN_POINT('Ctrl Pts',(22.1549843938465,-9.30976886072822,11.0724642143303));
#39434=CARTESIAN_POINT('Ctrl Pts',(22.8744776078269,-9.14996578827694,11.2039970972495));
#39435=CARTESIAN_POINT('Ctrl Pts',(23.5816077902765,-9.01558422395426,11.316201946695));
#39436=CARTESIAN_POINT('Ctrl Pts',(24.0500749276267,-8.9300835935144,11.3851612528795));
#39437=CARTESIAN_POINT('Ctrl Pts',(24.6365533946129,-8.83449183240035,11.4594652258085));
#39438=CARTESIAN_POINT('Ctrl Pts',(25.1102835291691,-8.76539275960638,11.5122699159732));
#39439=CARTESIAN_POINT('Ctrl Pts',(25.4658322439333,-8.71801358900149,11.5482688417074));
#39440=CARTESIAN_POINT('Ctrl Pts',(25.7624874136689,-8.6824463850995,11.5753180370235));
#39441=CARTESIAN_POINT('Ctrl Pts',(25.9700349923415,-8.65983585467444,11.592640163876));
#39442=CARTESIAN_POINT('Ctrl Pts',(26.0885791323133,-8.64758737376065,11.6020803597254));
#39443=CARTESIAN_POINT('Ctrl Pts',(26.1478525996408,-8.64169115913871,11.6066467500382));
#39444=CARTESIAN_POINT('Ctrl Pts',(26.6319130667266,-8.59444428954226,11.6433645250357));
#39445=CARTESIAN_POINT('Ctrl Pts',(27.5577774489369,-8.53717709311587,11.6860824768893));
#39446=CARTESIAN_POINT('Ctrl Pts',(28.5508423746858,-8.50942828058727,11.7050908260002));
#39447=CARTESIAN_POINT('Ctrl Pts',(29.1362159539423,-8.49263545125894,11.7174369518246));
#39448=CARTESIAN_POINT('Ctrl Pts',(29.2912819508841,-8.48875007883417,11.7203386713976));
#39449=CARTESIAN_POINT('Ctrl Pts',(29.610052998187,-8.48280581727731,11.7247475094471));
#39450=CARTESIAN_POINT('Ctrl Pts',(30.1693026775047,-8.47731190452096,11.728827902791));
#39451=CARTESIAN_POINT('Ctrl Pts',(31.3098786008463,-8.48127083805332,11.7258872894481));
#39452=CARTESIAN_POINT('Ctrl Pts',(32.3162827048883,-8.49575357359989,11.7152777874899));
#39453=CARTESIAN_POINT('Ctrl Pts',(33.1686195735697,-8.49577523975603,11.715269078277));
#39454=CARTESIAN_POINT('Ctrl Pts',(33.4952188807558,-8.49577770055114,11.7152682401723));
#39455=CARTESIAN_POINT('Ctrl Pts',(34.1547734244042,-8.49578208271197,11.7152665713231));
#39456=CARTESIAN_POINT('Ctrl Pts',(34.9764178792931,-8.49579602915746,11.7152614171757));
#39457=CARTESIAN_POINT('Ctrl Pts',(35.9640520550922,-8.49580175406157,11.7152592814565));
#39458=CARTESIAN_POINT('Ctrl Pts',(37.9385651163988,-8.49580966366,11.7152563511877));
#39459=CARTESIAN_POINT('Ctrl Pts',(39.5833333333333,-8.49584881729847,11.7152418049849));
#39460=CARTESIAN_POINT('Ctrl Pts',(40.9,-8.49584881729847,11.7152418049849));
#39461=CARTESIAN_POINT('Ctrl Pts',(6.84648239176542,-21.8719108775553,4.8711720049463));
#39462=CARTESIAN_POINT('Ctrl Pts',(7.61278097593421,-21.6080942034255,6.01809391809558));
#39463=CARTESIAN_POINT('Ctrl Pts',(8.41274152921387,-21.2759544371052,7.1129769401534));
#39464=CARTESIAN_POINT('Ctrl Pts',(10.1879716557546,-20.4198986989574,9.33526598964861));
#39465=CARTESIAN_POINT('Ctrl Pts',(11.1642573475929,-19.8462357742843,10.4645258845954));
#39466=CARTESIAN_POINT('Ctrl Pts',(13.1034321172788,-18.7228640453274,12.3837514736036));
#39467=CARTESIAN_POINT('Ctrl Pts',(14.0822646095709,-18.0925354910949,13.259092905625));
#39468=CARTESIAN_POINT('Ctrl Pts',(15.3084001581867,-17.369341405527,14.1807147676625));
#39469=CARTESIAN_POINT('Ctrl Pts',(16.2531227144981,-16.8032299545452,14.8695159890908));
#39470=CARTESIAN_POINT('Ctrl Pts',(17.2084375604977,-16.2348330754283,15.4708786153412));
#39471=CARTESIAN_POINT('Ctrl Pts',(18.8473961588579,-15.3570672461537,16.3684102669437));
#39472=CARTESIAN_POINT('Ctrl Pts',(19.8110405035782,-14.8437940564497,16.8164458459158));
#39473=CARTESIAN_POINT('Ctrl Pts',(20.9872655006161,-14.3329359049567,17.2594998647324));
#39474=CARTESIAN_POINT('Ctrl Pts',(21.4517346237735,-14.1338378277512,17.4254488483262));
#39475=CARTESIAN_POINT('Ctrl Pts',(22.3727984841465,-13.7614448137588,17.72174912934));
#39476=CARTESIAN_POINT('Ctrl Pts',(23.0743543377562,-13.5118529399622,17.9111527143536));
#39477=CARTESIAN_POINT('Ctrl Pts',(23.7582742987066,-13.3034745440381,18.0719640430563));
#39478=CARTESIAN_POINT('Ctrl Pts',(24.2174386855896,-13.1693266480668,18.1719103336479));
#39479=CARTESIAN_POINT('Ctrl Pts',(24.787021394359,-13.0207037868382,18.278521814341));
#39480=CARTESIAN_POINT('Ctrl Pts',(25.2463470121637,-12.9133861579984,18.3542161979474));
#39481=CARTESIAN_POINT('Ctrl Pts',(25.5899787396422,-12.840037267054,18.4056632423989));
#39482=CARTESIAN_POINT('Ctrl Pts',(25.8759048428227,-12.7850917865306,18.4442660174723));
#39483=CARTESIAN_POINT('Ctrl Pts',(26.0755068065032,-12.7502361709815,18.4689567859643));
#39484=CARTESIAN_POINT('Ctrl Pts',(26.1893780149132,-12.7313725692329,18.4824083304414));
#39485=CARTESIAN_POINT('Ctrl Pts',(26.2462863876023,-12.7222969574596,18.4889145361422));
#39486=CARTESIAN_POINT('Ctrl Pts',(26.7102722067275,-12.6496548741739,18.5411896593431));
#39487=CARTESIAN_POINT('Ctrl Pts',(27.5960905386888,-12.5614420302556,18.6020458648122));
#39488=CARTESIAN_POINT('Ctrl Pts',(28.5798438027286,-12.5173520665108,18.629899960324));
#39489=CARTESIAN_POINT('Ctrl Pts',(29.1658297917577,-12.4906249890439,18.6480680632814));
#39490=CARTESIAN_POINT('Ctrl Pts',(29.3147155528138,-12.4846522276656,18.6521962493032));
#39491=CARTESIAN_POINT('Ctrl Pts',(29.6257654938391,-12.4753713397182,18.6585637397073));
#39492=CARTESIAN_POINT('Ctrl Pts',(30.1719616098277,-12.4668129248999,18.6644443298454));
#39493=CARTESIAN_POINT('Ctrl Pts',(31.2977738410334,-12.472961188488,18.6602190141086));
#39494=CARTESIAN_POINT('Ctrl Pts',(32.3068669150108,-12.4961463862897,18.6445149503826));
#39495=CARTESIAN_POINT('Ctrl Pts',(33.1709127040733,-12.4962026881972,18.6444874715366));
#39496=CARTESIAN_POINT('Ctrl Pts',(33.4960830255434,-12.4962093123004,18.644484418038));
#39497=CARTESIAN_POINT('Ctrl Pts',(34.1563135822162,-12.4962208405724,18.6444789016084));
#39498=CARTESIAN_POINT('Ctrl Pts',(34.9772414248899,-12.4962577684095,18.6444614154564));
#39499=CARTESIAN_POINT('Ctrl Pts',(35.964946372113,-12.496272896639,18.6444542286038));
#39500=CARTESIAN_POINT('Ctrl Pts',(37.9391834323222,-12.4962938290757,18.6444443083029));
#39501=CARTESIAN_POINT('Ctrl Pts',(39.5833333333333,-12.4963973854122,18.6443951831047));
#39502=CARTESIAN_POINT('Ctrl Pts',(40.9,-12.4963973854122,18.6443951831047));
#39503=CARTESIAN_POINT('Ctrl Pts',(6.90857970435318,-29.5800408844791,7.02038826853569));
#39504=CARTESIAN_POINT('Ctrl Pts',(7.67983757144493,-29.1962153577801,8.58577901088989));
#39505=CARTESIAN_POINT('Ctrl Pts',(8.4844629659692,-28.7191114013952,10.0765485557758));
#39506=CARTESIAN_POINT('Ctrl Pts',(10.2687526859613,-27.5023711977385,13.0935628879538));
#39507=CARTESIAN_POINT('Ctrl Pts',(11.2489627292759,-26.6949552438923,14.6224501564806));
#39508=CARTESIAN_POINT('Ctrl Pts',(13.2065810728343,-25.1069038454383,17.2294066625499));
#39509=CARTESIAN_POINT('Ctrl Pts',(14.188432579866,-24.2271697832519,18.4069952853951));
#39510=CARTESIAN_POINT('Ctrl Pts',(15.4296983589676,-23.2080338536349,19.6550892131211));
#39511=CARTESIAN_POINT('Ctrl Pts',(16.3788042670987,-22.4189011948389,20.5796860932724));
#39512=CARTESIAN_POINT('Ctrl Pts',(17.3450159165718,-21.6217224592711,21.3903231452907));
#39513=CARTESIAN_POINT('Ctrl Pts',(18.9999962645463,-20.3951481814249,22.5937460627635));
#39514=CARTESIAN_POINT('Ctrl Pts',(19.9686658165166,-19.6835411202359,23.189805412739));
#39515=CARTESIAN_POINT('Ctrl Pts',(21.1489437168842,-18.9783964629487,23.775691048575));
#39516=CARTESIAN_POINT('Ctrl Pts',(21.6136662410168,-18.7043064424586,23.9949385633154));
#39517=CARTESIAN_POINT('Ctrl Pts',(22.5341605437883,-18.1932305660767,24.3846521737584));
#39518=CARTESIAN_POINT('Ctrl Pts',(23.2310352415765,-17.8537326154788,24.6315178872712));
#39519=CARTESIAN_POINT('Ctrl Pts',(23.9047680627613,-17.5731511638353,24.839431592137));
#39520=CARTESIAN_POINT('Ctrl Pts',(24.3593217251596,-17.3912549800692,24.9695871891304));
#39521=CARTESIAN_POINT('Ctrl Pts',(24.9191284505011,-17.1917285847409,25.1069751863361));
#39522=CARTESIAN_POINT('Ctrl Pts',(25.3687829483029,-17.0482631873595,25.2041659752938));
#39523=CARTESIAN_POINT('Ctrl Pts',(25.7038809466243,-16.9507036504245,25.2699171894924));
#39524=CARTESIAN_POINT('Ctrl Pts',(25.9815275275383,-16.8779731233106,25.3190677310926));
#39525=CARTESIAN_POINT('Ctrl Pts',(26.1747255747312,-16.8320233777013,25.3504124116981));
#39526=CARTESIAN_POINT('Ctrl Pts',(26.2847430019944,-16.8072090098455,25.367466019553));
#39527=CARTESIAN_POINT('Ctrl Pts',(26.3396756125256,-16.7952849898387,25.3757090167857));
#39528=CARTESIAN_POINT('Ctrl Pts',(26.7867185605552,-16.7000344271699,25.4418392909477));
#39529=CARTESIAN_POINT('Ctrl Pts',(27.6343089133552,-16.5847364280864,25.5185659559044));
#39530=CARTESIAN_POINT('Ctrl Pts',(28.6086204191332,-16.5243820587324,25.5552242576155));
#39531=CARTESIAN_POINT('Ctrl Pts',(29.1952293795949,-16.4877244301025,25.5792110357046));
#39532=CARTESIAN_POINT('Ctrl Pts',(29.3380035933319,-16.4799452423709,25.584403327273));
#39533=CARTESIAN_POINT('Ctrl Pts',(29.6413717635321,-16.4675695714433,25.5925899885791));
#39534=CARTESIAN_POINT('Ctrl Pts',(30.174536806517,-16.4561967872262,25.6001268754995));
#39535=CARTESIAN_POINT('Ctrl Pts',(31.2855894033322,-16.464330041984,25.5947346655064));
#39536=CARTESIAN_POINT('Ctrl Pts',(32.2974015084455,-16.4964013295029,25.5738307704501));
#39537=CARTESIAN_POINT('Ctrl Pts',(33.1731651112183,-16.4965224425527,25.5737672879574));
#39538=CARTESIAN_POINT('Ctrl Pts',(33.4969081472872,-16.4965369996129,25.5737598716201));
#39539=CARTESIAN_POINT('Ctrl Pts',(34.157816939104,-16.4965619872359,25.5737469053195));
#39540=CARTESIAN_POINT('Ctrl Pts',(34.9780359591179,-16.496642344611,25.5737054251287));
#39541=CARTESIAN_POINT('Ctrl Pts',(35.9658147840134,-16.4966752246753,25.5736884251096));
#39542=CARTESIAN_POINT('Ctrl Pts',(37.9397802282712,-16.4967207607426,25.5736649097449));
#39543=CARTESIAN_POINT('Ctrl Pts',(39.5833333333333,-16.4969459535258,25.5735485612246));
#39544=CARTESIAN_POINT('Ctrl Pts',(40.9,-16.4969459535258,25.5735485612246));
#39545=CARTESIAN_POINT('Ctrl Pts',(6.93528330520032,-33.9890447223856,8.231730283379));
#39546=CARTESIAN_POINT('Ctrl Pts',(7.70864561497005,-33.5376786188307,10.0357116563145));
#39547=CARTESIAN_POINT('Ctrl Pts',(8.51532719250786,-32.9786927413523,11.7528338486872));
#39548=CARTESIAN_POINT('Ctrl Pts',(10.3033707684643,-31.5578840442132,15.2242195800702));
#39549=CARTESIAN_POINT('Ctrl Pts',(11.285359425586,-30.6179424293772,16.9818886494149));
#39550=CARTESIAN_POINT('Ctrl Pts',(13.2503075123955,-28.7660858779662,19.9828238609275));
#39551=CARTESIAN_POINT('Ctrl Pts',(14.2335802328307,-27.744590382611,21.333808720003));
#39552=CARTESIAN_POINT('Ctrl Pts',(15.4809874764708,-26.5562215055806,22.7701484639684));
#39553=CARTESIAN_POINT('Ctrl Pts',(16.4318967140333,-25.6398645222148,23.8303538982284));
#39554=CARTESIAN_POINT('Ctrl Pts',(17.4027860882062,-24.7114068344531,24.7620955812504));
#39555=CARTESIAN_POINT('Ctrl Pts',(19.0657008739464,-23.2827894621994,26.1438767914272));
#39556=CARTESIAN_POINT('Ctrl Pts',(20.0370987955264,-22.4568785783625,26.8257745442828));
#39557=CARTESIAN_POINT('Ctrl Pts',(21.221937368182,-21.6368752952082,27.4963832022123));
#39558=CARTESIAN_POINT('Ctrl Pts',(21.6873545199149,-21.319265575768,27.7466423667128));
#39559=CARTESIAN_POINT('Ctrl Pts',(22.6095407883917,-20.7266792263567,28.1914275999319));
#39560=CARTESIAN_POINT('Ctrl Pts',(23.3063195468722,-20.3342063552501,28.4721721598035));
#39561=CARTESIAN_POINT('Ctrl Pts',(23.9774915837903,-20.0111563083467,28.7077527668382));
#39562=CARTESIAN_POINT('Ctrl Pts',(24.4307021142577,-19.8016082531844,28.8553793495039));
#39563=CARTESIAN_POINT('Ctrl Pts',(24.9871188326864,-19.5726095610121,29.010562613784));
#39564=CARTESIAN_POINT('Ctrl Pts',(25.4329141726817,-19.4084486444525,29.1200357132468));
#39565=CARTESIAN_POINT('Ctrl Pts',(25.76439505547,-19.2971155191109,29.1939083663027));
#39566=CARTESIAN_POINT('Ctrl Pts',(26.0382972138579,-19.2143910494176,29.2489718106942));
#39567=CARTESIAN_POINT('Ctrl Pts',(26.2284820979137,-19.1622606931672,29.284017210513));
#39568=CARTESIAN_POINT('Ctrl Pts',(26.3366494455064,-19.1341507449288,29.3030632173398));
#39569=CARTESIAN_POINT('Ctrl Pts',(26.3906225284368,-19.1206543727099,29.3122642693068));
#39570=CARTESIAN_POINT('Ctrl Pts',(26.8293654116034,-19.0129885834593,29.3859982106892));
#39571=CARTESIAN_POINT('Ctrl Pts',(27.6560988760145,-18.8833816200194,29.4710985842867));
#39572=CARTESIAN_POINT('Ctrl Pts',(28.6249317030318,-18.8137794716616,29.5127595133998));
#39573=CARTESIAN_POINT('Ctrl Pts',(29.2119052185273,-18.7714558506415,29.5400636810177));
#39574=CARTESIAN_POINT('Ctrl Pts',(29.351223493954,-18.7627335234215,29.5458124634024));
#39575=CARTESIAN_POINT('Ctrl Pts',(29.6502234545151,-18.7486685476099,29.5549926880432));
#39576=CARTESIAN_POINT('Ctrl Pts',(30.1759548990665,-18.7357718416967,29.5634265890421));
#39577=CARTESIAN_POINT('Ctrl Pts',(31.2785766862301,-18.7449771625331,29.5574021311857));
#39578=CARTESIAN_POINT('Ctrl Pts',(32.2919610610309,-18.7821959068194,29.5334837411524));
#39579=CARTESIAN_POINT('Ctrl Pts',(33.1744263360525,-18.7823679845324,29.533390407254));
#39580=CARTESIAN_POINT('Ctrl Pts',(33.4973548461808,-18.7823889294252,29.5333792377699));
#39581=CARTESIAN_POINT('Ctrl Pts',(34.1586526208335,-18.7824245927187,29.5333600113094));
#39582=CARTESIAN_POINT('Ctrl Pts',(34.978471543808,-18.7825395490483,29.5332982308031));
#39583=CARTESIAN_POINT('Ctrl Pts',(35.9662945600334,-18.7825865524221,29.5332729456428));
#39584=CARTESIAN_POINT('Ctrl Pts',(37.9401075800399,-18.7826516826344,29.533237934286));
#39585=CARTESIAN_POINT('Ctrl Pts',(39.5833333333333,-18.7829737067337,29.533064777293));
#39586=CARTESIAN_POINT('Ctrl Pts',(40.9,-18.7829737067337,29.533064777293));
#39587=CARTESIAN_POINT('Origin',(6.9,1.83697019872103E-15,30.));
#39588=CARTESIAN_POINT('',(6.9,-21.8303175223207,20.5775906479515));
#39589=CARTESIAN_POINT('Ctrl Pts',(6.9,-8.44145532612415,7.09789564133157));
#39590=CARTESIAN_POINT('Ctrl Pts',(6.9,-11.09468188726,9.87986401752105));
#39591=CARTESIAN_POINT('Ctrl Pts',(6.90000000166257,-13.9485622548227,12.753513475675));
#39592=CARTESIAN_POINT('Ctrl Pts',(6.90000000166257,-18.0885125115534,16.8843019432417));
#39593=CARTESIAN_POINT('Ctrl Pts',(6.9,-19.9691972794379,18.7449692586141));
#39594=CARTESIAN_POINT('Ctrl Pts',(6.9,-21.8303175223207,20.5775906479515));
#39595=CARTESIAN_POINT('Origin',(6.9,0.,0.));
#39596=CARTESIAN_POINT('Origin',(40.9,5.51091059616309E-16,9.));
#39597=CARTESIAN_POINT('Ctrl Pts',(40.9,-1.5,34.4673758792282));
#39598=CARTESIAN_POINT('Ctrl Pts',(40.9,-1.5,33.9668810740701));
#39599=CARTESIAN_POINT('Ctrl Pts',(40.9,-1.5,33.466386268912));
#39600=CARTESIAN_POINT('Ctrl Pts',(40.9,-1.5,32.9658914637539));
#39601=CARTESIAN_POINT('Ctrl Pts',(30.5,1.56108868151375,34.9651684126997));
#39602=CARTESIAN_POINT('Ctrl Pts',(30.5,0.780932928377882,35.));
#39603=CARTESIAN_POINT('Ctrl Pts',(30.5,2.14313189850787E-15,35.));
#39604=CARTESIAN_POINT('Ctrl Pts',(30.5,-35.,35.));
#39605=CARTESIAN_POINT('Ctrl Pts',(30.5,-35.,2.14313189850787E-15));
#39606=CARTESIAN_POINT('Ctrl Pts',(30.5,-35.,-35.));
#39607=CARTESIAN_POINT('Ctrl Pts',(30.5,-2.14313189850787E-15,-35.));
#39608=CARTESIAN_POINT('Ctrl Pts',(30.5,35.,-35.));
#39609=CARTESIAN_POINT('Ctrl Pts',(30.5,35.,-2.14313189850787E-15));
#39610=CARTESIAN_POINT('Ctrl Pts',(30.5,35.,33.472222479613));
#39611=CARTESIAN_POINT('Ctrl Pts',(30.5,1.56108868151375,34.9651684126997));
#39612=CARTESIAN_POINT('Ctrl Pts',(30.3311478274255,1.55772383604587,34.8898028105656));
#39613=CARTESIAN_POINT('Ctrl Pts',(30.3311478274255,0.779249668063536,34.924559320191));
#39614=CARTESIAN_POINT('Ctrl Pts',(30.3311478274255,2.13851248915519E-15,
34.924559320191));
#39615=CARTESIAN_POINT('Ctrl Pts',(30.3311478274255,-34.924559320191,34.924559320191));
#39616=CARTESIAN_POINT('Ctrl Pts',(30.3311478274255,-34.924559320191,2.13851248915519E-15));
#39617=CARTESIAN_POINT('Ctrl Pts',(30.3311478274255,-34.924559320191,-34.924559320191));
#39618=CARTESIAN_POINT('Ctrl Pts',(30.3311478274255,-2.13851248915519E-15,
-34.924559320191));
#39619=CARTESIAN_POINT('Ctrl Pts',(30.3311478274255,34.924559320191,-34.924559320191));
#39620=CARTESIAN_POINT('Ctrl Pts',(30.3311478274255,34.924559320191,-2.13851248915519E-15));
#39621=CARTESIAN_POINT('Ctrl Pts',(30.3311478274255,34.924559320191,33.4000748447964));
#39622=CARTESIAN_POINT('Ctrl Pts',(30.3311478274255,1.55772383604587,34.8898028105656));
#39623=CARTESIAN_POINT('Ctrl Pts',(29.9897712690917,1.55090794481747,34.7371408974366));
#39624=CARTESIAN_POINT('Ctrl Pts',(29.9897712690917,0.775840025831459,34.7717453283792));
#39625=CARTESIAN_POINT('Ctrl Pts',(29.9897712690917,2.12915533085832E-15,
34.7717453283792));
#39626=CARTESIAN_POINT('Ctrl Pts',(29.9897712690917,-34.7717453283791,34.7717453283791));
#39627=CARTESIAN_POINT('Ctrl Pts',(29.9897712690917,-34.7717453283792,2.12915533085832E-15));
#39628=CARTESIAN_POINT('Ctrl Pts',(29.9897712690917,-34.7717453283791,-34.7717453283791));
#39629=CARTESIAN_POINT('Ctrl Pts',(29.9897712690917,-2.12915533085832E-15,
-34.7717453283792));
#39630=CARTESIAN_POINT('Ctrl Pts',(29.9897712690917,34.7717453283791,-34.7717453283791));
#39631=CARTESIAN_POINT('Ctrl Pts',(29.9897712690917,34.7717453283792,-2.12915533085832E-15));
#39632=CARTESIAN_POINT('Ctrl Pts',(29.9897712690917,34.7717453283791,33.2539313038843));
#39633=CARTESIAN_POINT('Ctrl Pts',(29.9897712690917,1.55090794481747,34.7371408974366));
#39634=CARTESIAN_POINT('Ctrl Pts',(29.4666899049319,1.54042548027394,34.5023553003819));
#39635=CARTESIAN_POINT('Ctrl Pts',(29.4666899049319,0.770596184255045,34.5367258427036));
#39636=CARTESIAN_POINT('Ctrl Pts',(29.4666899049319,2.11476453781483E-15,
34.5367258427036));
#39637=CARTESIAN_POINT('Ctrl Pts',(29.4666899049319,-34.5367258427036,34.5367258427036));
#39638=CARTESIAN_POINT('Ctrl Pts',(29.4666899049319,-34.5367258427036,2.11476453781483E-15));
#39639=CARTESIAN_POINT('Ctrl Pts',(29.4666899049319,-34.5367258427036,-34.5367258427036));
#39640=CARTESIAN_POINT('Ctrl Pts',(29.4666899049319,-2.11476453781483E-15,
-34.5367258427036));
#39641=CARTESIAN_POINT('Ctrl Pts',(29.4666899049319,34.5367258427036,-34.5367258427036));
#39642=CARTESIAN_POINT('Ctrl Pts',(29.4666899049319,34.5367258427036,-2.11476453781483E-15));
#39643=CARTESIAN_POINT('Ctrl Pts',(29.4666899049319,34.5367258427036,33.0291706035535));
#39644=CARTESIAN_POINT('Ctrl Pts',(29.4666899049319,1.54042548027394,34.5023553003819));
#39645=CARTESIAN_POINT('Ctrl Pts',(28.7471241621752,1.52592972576568,34.1776802811774));
#39646=CARTESIAN_POINT('Ctrl Pts',(28.7471241621752,0.763344698704457,34.21172738887));
#39647=CARTESIAN_POINT('Ctrl Pts',(28.7471241621752,2.09486412200407E-15,
34.21172738887));
#39648=CARTESIAN_POINT('Ctrl Pts',(28.7471241621752,-34.2117273888699,34.2117273888699));
#39649=CARTESIAN_POINT('Ctrl Pts',(28.7471241621752,-34.21172738887,2.09486412200407E-15));
#39650=CARTESIAN_POINT('Ctrl Pts',(28.7471241621752,-34.2117273888699,-34.2117273888699));
#39651=CARTESIAN_POINT('Ctrl Pts',(28.7471241621752,-2.09486412200407E-15,
-34.21172738887));
#39652=CARTESIAN_POINT('Ctrl Pts',(28.7471241621752,34.2117273888699,-34.2117273888699));
#39653=CARTESIAN_POINT('Ctrl Pts',(28.7471241621752,34.21172738887,-2.09486412200407E-15));
#39654=CARTESIAN_POINT('Ctrl Pts',(28.7471241621752,34.2117273888699,32.718358587775));
#39655=CARTESIAN_POINT('Ctrl Pts',(28.7471241621752,1.52592972576568,34.1776802811774));
#39656=CARTESIAN_POINT('Ctrl Pts',(27.8100958442934,1.50698029472894,33.7532520886149));
#39657=CARTESIAN_POINT('Ctrl Pts',(27.8100958442934,0.753865266276396,33.7868763896026));
#39658=CARTESIAN_POINT('Ctrl Pts',(27.8100958442934,2.06884950118571E-15,
33.7868763896026));
#39659=CARTESIAN_POINT('Ctrl Pts',(27.8100958442934,-33.7868763896026,33.7868763896026));
#39660=CARTESIAN_POINT('Ctrl Pts',(27.8100958442934,-33.7868763896026,2.06884950118571E-15));
#39661=CARTESIAN_POINT('Ctrl Pts',(27.8100958442934,-33.7868763896026,-33.7868763896026));
#39662=CARTESIAN_POINT('Ctrl Pts',(27.8100958442934,-2.06884950118571E-15,
-33.7868763896026));
#39663=CARTESIAN_POINT('Ctrl Pts',(27.8100958442934,33.7868763896026,-33.7868763896026));
#39664=CARTESIAN_POINT('Ctrl Pts',(27.8100958442934,33.7868763896026,-2.06884950118571E-15));
#39665=CARTESIAN_POINT('Ctrl Pts',(27.8100958442934,33.7868763896026,32.3120526686846));
#39666=CARTESIAN_POINT('Ctrl Pts',(27.8100958442934,1.50698029472894,33.7532520886149));
#39667=CARTESIAN_POINT('Ctrl Pts',(26.8343111708818,1.48733431337754,33.3132226048841));
#39668=CARTESIAN_POINT('Ctrl Pts',(26.8343111708818,0.744037385305068,33.3464085574791));
#39669=CARTESIAN_POINT('Ctrl Pts',(26.8343111708818,2.04187862514883E-15,
33.3464085574791));
#39670=CARTESIAN_POINT('Ctrl Pts',(26.8343111708818,-33.3464085574791,33.3464085574791));
#39671=CARTESIAN_POINT('Ctrl Pts',(26.8343111708818,-33.3464085574791,2.04187862514883E-15));
#39672=CARTESIAN_POINT('Ctrl Pts',(26.8343111708818,-33.3464085574791,-33.3464085574791));
#39673=CARTESIAN_POINT('Ctrl Pts',(26.8343111708818,-2.04187862514883E-15,
-33.3464085574791));
#39674=CARTESIAN_POINT('Ctrl Pts',(26.8343111708818,33.3464085574791,-33.3464085574791));
#39675=CARTESIAN_POINT('Ctrl Pts',(26.8343111708818,33.3464085574791,-2.04187862514883E-15));
#39676=CARTESIAN_POINT('Ctrl Pts',(26.8343111708818,33.3464085574791,31.8908116037717));
#39677=CARTESIAN_POINT('Ctrl Pts',(26.8343111708818,1.48733431337754,33.3132226048841));
#39678=CARTESIAN_POINT('Ctrl Pts',(25.8181479469611,1.46726916269953,32.8638045923198));
#39679=CARTESIAN_POINT('Ctrl Pts',(25.8181479469611,0.733999815330425,32.8965428438611));
#39680=CARTESIAN_POINT('Ctrl Pts',(25.8181479469611,2.01433229483741E-15,
32.8965428438611));
#39681=CARTESIAN_POINT('Ctrl Pts',(25.8181479469611,-32.896542843861,32.896542843861));
#39682=CARTESIAN_POINT('Ctrl Pts',(25.8181479469611,-32.8965428438611,2.01433229483741E-15));
#39683=CARTESIAN_POINT('Ctrl Pts',(25.8181479469611,-32.896542843861,-32.896542843861));
#39684=CARTESIAN_POINT('Ctrl Pts',(25.8181479469611,-2.01433229483741E-15,
-32.8965428438611));
#39685=CARTESIAN_POINT('Ctrl Pts',(25.8181479469611,32.896542843861,-32.896542843861));
#39686=CARTESIAN_POINT('Ctrl Pts',(25.8181479469611,32.8965428438611,-2.01433229483741E-15));
#39687=CARTESIAN_POINT('Ctrl Pts',(25.8181479469611,32.896542843861,31.4605828822811));
#39688=CARTESIAN_POINT('Ctrl Pts',(25.8181479469611,1.46726916269953,32.8638045923198));
#39689=CARTESIAN_POINT('Ctrl Pts',(24.7595197917227,1.44728584082668,32.4162193763075));
#39690=CARTESIAN_POINT('Ctrl Pts',(24.7595197917227,0.724003180127257,32.4485117525897));
#39691=CARTESIAN_POINT('Ctrl Pts',(24.7595197917227,1.98689830274521E-15,
32.4485117525897));
#39692=CARTESIAN_POINT('Ctrl Pts',(24.7595197917227,-32.4485117525897,32.4485117525897));
#39693=CARTESIAN_POINT('Ctrl Pts',(24.7595197917227,-32.4485117525897,1.98689830274521E-15));
#39694=CARTESIAN_POINT('Ctrl Pts',(24.7595197917227,-32.4485117525897,-32.4485117525897));
#39695=CARTESIAN_POINT('Ctrl Pts',(24.7595197917227,-1.98689830274521E-15,
-32.4485117525897));
#39696=CARTESIAN_POINT('Ctrl Pts',(24.7595197917227,32.4485117525897,-32.4485117525897));
#39697=CARTESIAN_POINT('Ctrl Pts',(24.7595197917227,32.4485117525897,-1.98689830274521E-15));
#39698=CARTESIAN_POINT('Ctrl Pts',(24.7595197917227,32.4485117525897,31.0321087004291));
#39699=CARTESIAN_POINT('Ctrl Pts',(24.7595197917227,1.44728584082668,32.4162193763075));
#39700=CARTESIAN_POINT('Ctrl Pts',(23.6563574780851,1.42804494464108,31.9852629652417));
#39701=CARTESIAN_POINT('Ctrl Pts',(23.6563574780851,0.714377942573,32.017126031541));
#39702=CARTESIAN_POINT('Ctrl Pts',(23.6563574780851,1.9604835456212E-15,
32.017126031541));
#39703=CARTESIAN_POINT('Ctrl Pts',(23.6563574780851,-32.017126031541,32.017126031541));
#39704=CARTESIAN_POINT('Ctrl Pts',(23.6563574780851,-32.017126031541,1.9604835456212E-15));
#39705=CARTESIAN_POINT('Ctrl Pts',(23.6563574780851,-32.017126031541,-32.017126031541));
#39706=CARTESIAN_POINT('Ctrl Pts',(23.6563574780851,-1.9604835456212E-15,
-32.017126031541));
#39707=CARTESIAN_POINT('Ctrl Pts',(23.6563574780851,32.017126031541,-32.017126031541));
#39708=CARTESIAN_POINT('Ctrl Pts',(23.6563574780851,32.017126031541,-1.9604835456212E-15));
#39709=CARTESIAN_POINT('Ctrl Pts',(23.6563574780851,32.017126031541,30.6195533053014));
#39710=CARTESIAN_POINT('Ctrl Pts',(23.6563574780851,1.42804494464108,31.9852629652417));
#39711=CARTESIAN_POINT('Ctrl Pts',(22.5073180101405,1.41024006077928,31.5864702700101));
#39712=CARTESIAN_POINT('Ctrl Pts',(22.5073180101405,0.70547106863414,31.6179360671638));
#39713=CARTESIAN_POINT('Ctrl Pts',(22.5073180101405,1.93604021001489E-15,
31.6179360671638));
#39714=CARTESIAN_POINT('Ctrl Pts',(22.5073180101405,-31.6179360671638,31.6179360671638));
#39715=CARTESIAN_POINT('Ctrl Pts',(22.5073180101405,-31.6179360671638,1.93604021001489E-15));
#39716=CARTESIAN_POINT('Ctrl Pts',(22.5073180101405,-31.6179360671638,-31.6179360671638));
#39717=CARTESIAN_POINT('Ctrl Pts',(22.5073180101405,-1.93604021001489E-15,
-31.6179360671638));
#39718=CARTESIAN_POINT('Ctrl Pts',(22.5073180101405,31.6179360671638,-31.6179360671638));
#39719=CARTESIAN_POINT('Ctrl Pts',(22.5073180101405,31.6179360671638,-1.93604021001489E-15));
#39720=CARTESIAN_POINT('Ctrl Pts',(22.5073180101405,31.6179360671638,30.237788296751));
#39721=CARTESIAN_POINT('Ctrl Pts',(22.5073180101405,1.41024006077928,31.5864702700101));
#39722=CARTESIAN_POINT('Ctrl Pts',(21.3125219557939,1.394486513532,31.2336232862855));
#39723=CARTESIAN_POINT('Ctrl Pts',(21.3125219557939,0.697590373623123,31.264737584474));
#39724=CARTESIAN_POINT('Ctrl Pts',(21.3125219557939,1.9144130404504E-15,
31.264737584474));
#39725=CARTESIAN_POINT('Ctrl Pts',(21.3125219557939,-31.264737584474,31.264737584474));
#39726=CARTESIAN_POINT('Ctrl Pts',(21.3125219557939,-31.264737584474,1.9144130404504E-15));
#39727=CARTESIAN_POINT('Ctrl Pts',(21.3125219557939,-31.264737584474,-31.264737584474));
#39728=CARTESIAN_POINT('Ctrl Pts',(21.3125219557939,-1.9144130404504E-15,
-31.264737584474));
#39729=CARTESIAN_POINT('Ctrl Pts',(21.3125219557939,31.264737584474,-31.264737584474));
#39730=CARTESIAN_POINT('Ctrl Pts',(21.3125219557939,31.264737584474,-1.9144130404504E-15));
#39731=CARTESIAN_POINT('Ctrl Pts',(21.3125219557939,31.264737584474,29.9000072055494));
#39732=CARTESIAN_POINT('Ctrl Pts',(21.3125219557939,1.394486513532,31.2336232862855));
#39733=CARTESIAN_POINT('Ctrl Pts',(20.0742472323676,1.3812125919422,30.9363148057487));
#39734=CARTESIAN_POINT('Ctrl Pts',(20.0742472323676,0.690950108671535,30.9671329312955));
#39735=CARTESIAN_POINT('Ctrl Pts',(20.0742472323676,1.89619001115408E-15,
30.9671329312955));
#39736=CARTESIAN_POINT('Ctrl Pts',(20.0742472323676,-30.9671329312955,30.9671329312955));
#39737=CARTESIAN_POINT('Ctrl Pts',(20.0742472323676,-30.9671329312955,1.89619001115408E-15));
#39738=CARTESIAN_POINT('Ctrl Pts',(20.0742472323676,-30.9671329312955,-30.9671329312955));
#39739=CARTESIAN_POINT('Ctrl Pts',(20.0742472323676,-1.89619001115408E-15,
-30.9671329312955));
#39740=CARTESIAN_POINT('Ctrl Pts',(20.0742472323676,30.9671329312955,-30.9671329312955));
#39741=CARTESIAN_POINT('Ctrl Pts',(20.0742472323676,30.9671329312955,-1.89619001115408E-15));
#39742=CARTESIAN_POINT('Ctrl Pts',(20.0742472323676,30.9671329312955,29.6153932294878));
#39743=CARTESIAN_POINT('Ctrl Pts',(20.0742472323676,1.3812125919422,30.9363148057487));
#39744=CARTESIAN_POINT('Ctrl Pts',(18.7979917002302,1.3705167280896,30.6967495040754));
#39745=CARTESIAN_POINT('Ctrl Pts',(18.7979917002302,0.685599514321029,30.727328979557));
#39746=CARTESIAN_POINT('Ctrl Pts',(18.7979917002302,1.88150625405811E-15,
30.727328979557));
#39747=CARTESIAN_POINT('Ctrl Pts',(18.7979917002302,-30.727328979557,30.727328979557));
#39748=CARTESIAN_POINT('Ctrl Pts',(18.7979917002302,-30.727328979557,1.88150625405811E-15));
#39749=CARTESIAN_POINT('Ctrl Pts',(18.7979917002302,-30.727328979557,-30.727328979557));
#39750=CARTESIAN_POINT('Ctrl Pts',(18.7979917002302,-1.88150625405811E-15,
-30.727328979557));
#39751=CARTESIAN_POINT('Ctrl Pts',(18.7979917002302,30.727328979557,-30.727328979557));
#39752=CARTESIAN_POINT('Ctrl Pts',(18.7979917002302,30.727328979557,-1.88150625405811E-15));
#39753=CARTESIAN_POINT('Ctrl Pts',(18.7979917002302,30.727328979557,29.3860569087997));
#39754=CARTESIAN_POINT('Ctrl Pts',(18.7979917002302,1.3705167280896,30.6967495040754));
#39755=CARTESIAN_POINT('Ctrl Pts',(17.4917404060759,1.36221698336641,30.5108523315028));
#39756=CARTESIAN_POINT('Ctrl Pts',(17.4917404060759,0.681447575979397,30.5412466200144));
#39757=CARTESIAN_POINT('Ctrl Pts',(17.4917404060759,1.87011199575853E-15,
30.5412466200144));
#39758=CARTESIAN_POINT('Ctrl Pts',(17.4917404060759,-30.5412466200144,30.5412466200144));
#39759=CARTESIAN_POINT('Ctrl Pts',(17.4917404060759,-30.5412466200144,1.87011199575853E-15));
#39760=CARTESIAN_POINT('Ctrl Pts',(17.4917404060759,-30.5412466200144,-30.5412466200144));
#39761=CARTESIAN_POINT('Ctrl Pts',(17.4917404060759,-1.87011199575853E-15,
-30.5412466200144));
#39762=CARTESIAN_POINT('Ctrl Pts',(17.4917404060759,30.5412466200144,-30.5412466200144));
#39763=CARTESIAN_POINT('Ctrl Pts',(17.4917404060759,30.5412466200144,-1.87011199575853E-15));
#39764=CARTESIAN_POINT('Ctrl Pts',(17.4917404060759,30.5412466200144,29.2080971905671));
#39765=CARTESIAN_POINT('Ctrl Pts',(17.4917404060759,1.36221698336641,30.5108523315028));
#39766=CARTESIAN_POINT('Ctrl Pts',(16.1647270995715,1.35595673938413,30.3706357712668));
#39767=CARTESIAN_POINT('Ctrl Pts',(16.1647270995715,0.678315895682604,30.4008903789023));
#39768=CARTESIAN_POINT('Ctrl Pts',(16.1647270995715,1.86151765468761E-15,
30.4008903789023));
#39769=CARTESIAN_POINT('Ctrl Pts',(16.1647270995715,-30.4008903789023,30.4008903789023));
#39770=CARTESIAN_POINT('Ctrl Pts',(16.1647270995715,-30.4008903789023,1.86151765468761E-15));
#39771=CARTESIAN_POINT('Ctrl Pts',(16.1647270995715,-30.4008903789023,-30.4008903789023));
#39772=CARTESIAN_POINT('Ctrl Pts',(16.1647270995715,-1.86151765468761E-15,
-30.4008903789023));
#39773=CARTESIAN_POINT('Ctrl Pts',(16.1647270995715,30.4008903789023,-30.4008903789023));
#39774=CARTESIAN_POINT('Ctrl Pts',(16.1647270995715,30.4008903789023,-1.86151765468761E-15));
#39775=CARTESIAN_POINT('Ctrl Pts',(16.1647270995715,30.4008903789023,29.0738676097412));
#39776=CARTESIAN_POINT('Ctrl Pts',(16.1647270995715,1.35595673938413,30.3706357712668));
#39777=CARTESIAN_POINT('Ctrl Pts',(14.8263876417415,1.3512881251525,30.2660684364343));
#39778=CARTESIAN_POINT('Ctrl Pts',(14.8263876417415,0.675980426451066,30.2962188762246));
#39779=CARTESIAN_POINT('Ctrl Pts',(14.8263876417415,1.8551083736518E-15,
30.2962188762246));
#39780=CARTESIAN_POINT('Ctrl Pts',(14.8263876417415,-30.2962188762245,30.2962188762245));
#39781=CARTESIAN_POINT('Ctrl Pts',(14.8263876417415,-30.2962188762246,1.8551083736518E-15));
#39782=CARTESIAN_POINT('Ctrl Pts',(14.8263876417415,-30.2962188762245,-30.2962188762245));
#39783=CARTESIAN_POINT('Ctrl Pts',(14.8263876417415,-1.8551083736518E-15,
-30.2962188762246));
#39784=CARTESIAN_POINT('Ctrl Pts',(14.8263876417415,30.2962188762245,-30.2962188762245));
#39785=CARTESIAN_POINT('Ctrl Pts',(14.8263876417415,30.2962188762246,-1.8551083736518E-15));
#39786=CARTESIAN_POINT('Ctrl Pts',(14.8263876417415,30.2962188762245,28.9737651004582));
#39787=CARTESIAN_POINT('Ctrl Pts',(14.8263876417415,1.3512881251525,30.2660684364343));
#39788=CARTESIAN_POINT('Ctrl Pts',(13.4853470903953,1.34775518513426,30.186937862885));
#39789=CARTESIAN_POINT('Ctrl Pts',(13.4853470903953,0.674213077019291,30.2170094744125));
#39790=CARTESIAN_POINT('Ctrl Pts',(13.4853470903953,1.85025819663223E-15,
30.2170094744125));
#39791=CARTESIAN_POINT('Ctrl Pts',(13.4853470903953,-30.2170094744125,30.2170094744125));
#39792=CARTESIAN_POINT('Ctrl Pts',(13.4853470903953,-30.2170094744125,1.85025819663223E-15));
#39793=CARTESIAN_POINT('Ctrl Pts',(13.4853470903953,-30.2170094744125,-30.2170094744125));
#39794=CARTESIAN_POINT('Ctrl Pts',(13.4853470903953,-1.85025819663223E-15,
-30.2170094744125));
#39795=CARTESIAN_POINT('Ctrl Pts',(13.4853470903953,30.2170094744125,-30.2170094744125));
#39796=CARTESIAN_POINT('Ctrl Pts',(13.4853470903953,30.2170094744125,-1.85025819663223E-15));
#39797=CARTESIAN_POINT('Ctrl Pts',(13.4853470903953,30.2170094744125,28.8980132513174));
#39798=CARTESIAN_POINT('Ctrl Pts',(13.4853470903953,1.34775518513426,30.186937862885));
#39799=CARTESIAN_POINT('Ctrl Pts',(12.1482076787549,1.34498727870742,30.1249424647305));
#39800=CARTESIAN_POINT('Ctrl Pts',(12.1482076787549,0.672828434816076,30.1549523177074));
#39801=CARTESIAN_POINT('Ctrl Pts',(12.1482076787549,1.84645829171607E-15,
30.1549523177074));
#39802=CARTESIAN_POINT('Ctrl Pts',(12.1482076787549,-30.1549523177074,30.1549523177074));
#39803=CARTESIAN_POINT('Ctrl Pts',(12.1482076787549,-30.1549523177074,1.84645829171607E-15));
#39804=CARTESIAN_POINT('Ctrl Pts',(12.1482076787549,-30.1549523177074,-30.1549523177074));
#39805=CARTESIAN_POINT('Ctrl Pts',(12.1482076787549,-1.84645829171607E-15,
-30.1549523177074));
#39806=CARTESIAN_POINT('Ctrl Pts',(12.1482076787549,30.1549523177074,-30.1549523177074));
#39807=CARTESIAN_POINT('Ctrl Pts',(12.1482076787549,30.1549523177074,-1.84645829171607E-15));
#39808=CARTESIAN_POINT('Ctrl Pts',(12.1482076787549,30.1549523177074,28.8386649382978));
#39809=CARTESIAN_POINT('Ctrl Pts',(12.1482076787549,1.34498727870742,30.1249424647305));
#39810=CARTESIAN_POINT('Ctrl Pts',(10.8190675759626,1.34274367710657,30.0746904138676));
#39811=CARTESIAN_POINT('Ctrl Pts',(10.8190675759626,0.671706075536288,30.1046502067769));
#39812=CARTESIAN_POINT('Ctrl Pts',(10.8190675759626,1.843378175759E-15,
30.1046502067769));
#39813=CARTESIAN_POINT('Ctrl Pts',(10.8190675759626,-30.1046502067769,30.1046502067769));
#39814=CARTESIAN_POINT('Ctrl Pts',(10.8190675759626,-30.1046502067769,1.843378175759E-15));
#39815=CARTESIAN_POINT('Ctrl Pts',(10.8190675759626,-30.1046502067769,-30.1046502067769));
#39816=CARTESIAN_POINT('Ctrl Pts',(10.8190675759626,-1.843378175759E-15,
-30.1046502067769));
#39817=CARTESIAN_POINT('Ctrl Pts',(10.8190675759626,30.1046502067769,-30.1046502067769));
#39818=CARTESIAN_POINT('Ctrl Pts',(10.8190675759626,30.1046502067769,-1.843378175759E-15));
#39819=CARTESIAN_POINT('Ctrl Pts',(10.8190675759626,30.1046502067769,28.7905585540618));
#39820=CARTESIAN_POINT('Ctrl Pts',(10.8190675759626,1.34274367710657,30.0746904138676));
#39821=CARTESIAN_POINT('Ctrl Pts',(9.50027713254189,1.34087520118769,30.032840404991));
#39822=CARTESIAN_POINT('Ctrl Pts',(9.50027713254189,0.670771372474117,30.0627585077754));
#39823=CARTESIAN_POINT('Ctrl Pts',(9.50027713254189,1.84081304900435E-15,
30.0627585077754));
#39824=CARTESIAN_POINT('Ctrl Pts',(9.50027713254189,-30.0627585077753,30.0627585077753));
#39825=CARTESIAN_POINT('Ctrl Pts',(9.50027713254189,-30.0627585077754,1.84081304900435E-15));
#39826=CARTESIAN_POINT('Ctrl Pts',(9.5002771325419,-30.0627585077753,-30.0627585077753));
#39827=CARTESIAN_POINT('Ctrl Pts',(9.5002771325419,-1.84081304900435E-15,
-30.0627585077754));
#39828=CARTESIAN_POINT('Ctrl Pts',(9.5002771325419,30.0627585077753,-30.0627585077753));
#39829=CARTESIAN_POINT('Ctrl Pts',(9.50027713254189,30.0627585077754,-1.84081304900435E-15));
#39830=CARTESIAN_POINT('Ctrl Pts',(9.50027713254189,30.0627585077753,28.750495460661));
#39831=CARTESIAN_POINT('Ctrl Pts',(9.50027713254189,1.34087520118769,30.032840404991));
#39832=CARTESIAN_POINT('Ctrl Pts',(8.45435372222587,1.33961990745209,30.0047244129961));
#39833=CARTESIAN_POINT('Ctrl Pts',(8.45435372222587,0.670143413137451,30.0346145072029));
#39834=CARTESIAN_POINT('Ctrl Pts',(8.45435372222587,1.83908972599354E-15,
30.0346145072029));
#39835=CARTESIAN_POINT('Ctrl Pts',(8.45435372222587,-30.0346145072029,30.0346145072029));
#39836=CARTESIAN_POINT('Ctrl Pts',(8.45435372222587,-30.0346145072029,1.83908972599354E-15));
#39837=CARTESIAN_POINT('Ctrl Pts',(8.45435372222587,-30.0346145072029,-30.0346145072029));
#39838=CARTESIAN_POINT('Ctrl Pts',(8.45435372222587,-1.83908972599354E-15,
-30.0346145072029));
#39839=CARTESIAN_POINT('Ctrl Pts',(8.45435372222587,30.0346145072029,-30.0346145072029));
#39840=CARTESIAN_POINT('Ctrl Pts',(8.45435372222587,30.0346145072029,-1.83908972599354E-15));
#39841=CARTESIAN_POINT('Ctrl Pts',(8.45435372222587,30.0346145072029,28.7235799678431));
#39842=CARTESIAN_POINT('Ctrl Pts',(8.45435372222587,1.33961990745209,30.0047244129961));
#39843=CARTESIAN_POINT('Ctrl Pts',(7.67514864245731,1.33880061938141,29.9863740491064));
#39844=CARTESIAN_POINT('Ctrl Pts',(7.67514864245731,0.669733565164176,30.0162458630552));
#39845=CARTESIAN_POINT('Ctrl Pts',(7.67514864245731,1.83796497093053E-15,
30.0162458630552));
#39846=CARTESIAN_POINT('Ctrl Pts',(7.67514864245731,-30.0162458630552,30.0162458630552));
#39847=CARTESIAN_POINT('Ctrl Pts',(7.67514864245731,-30.0162458630552,1.83796497093053E-15));
#39848=CARTESIAN_POINT('Ctrl Pts',(7.67514864245731,-30.0162458630552,-30.0162458630552));
#39849=CARTESIAN_POINT('Ctrl Pts',(7.67514864245731,-1.83796497093053E-15,
-30.0162458630552));
#39850=CARTESIAN_POINT('Ctrl Pts',(7.67514864245731,30.0162458630552,-30.0162458630552));
#39851=CARTESIAN_POINT('Ctrl Pts',(7.67514864245731,30.0162458630552,-1.83796497093053E-15));
#39852=CARTESIAN_POINT('Ctrl Pts',(7.67514864245731,30.0162458630552,28.7060131294556));
#39853=CARTESIAN_POINT('Ctrl Pts',(7.67514864245731,1.33880061938141,29.9863740491064));
#39854=CARTESIAN_POINT('Ctrl Pts',(7.15799654185577,1.33830853171149,29.9753522996976));
#39855=CARTESIAN_POINT('Ctrl Pts',(7.15799654185577,0.669487398838304,30.0052131340045));
#39856=CARTESIAN_POINT('Ctrl Pts',(7.15799654185577,1.83728941111464E-15,
30.0052131340045));
#39857=CARTESIAN_POINT('Ctrl Pts',(7.15799654185577,-30.0052131340045,30.0052131340045));
#39858=CARTESIAN_POINT('Ctrl Pts',(7.15799654185577,-30.0052131340045,1.83728941111464E-15));
#39859=CARTESIAN_POINT('Ctrl Pts',(7.15799654185577,-30.0052131340045,-30.0052131340045));
#39860=CARTESIAN_POINT('Ctrl Pts',(7.15799654185577,-1.83728941111464E-15,
-30.0052131340045));
#39861=CARTESIAN_POINT('Ctrl Pts',(7.15799654185577,30.0052131340045,-30.0052131340045));
#39862=CARTESIAN_POINT('Ctrl Pts',(7.15799654185577,30.0052131340045,-1.83728941111464E-15));
#39863=CARTESIAN_POINT('Ctrl Pts',(7.15799654185577,30.0052131340045,28.695461987703));
#39864=CARTESIAN_POINT('Ctrl Pts',(7.15799654185577,1.33830853171149,29.9753522996976));
#39865=CARTESIAN_POINT('Ctrl Pts',(6.9,1.33807601272607,29.9701443537426));
#39866=CARTESIAN_POINT('Ctrl Pts',(6.9,0.669371081466756,30.));
#39867=CARTESIAN_POINT('Ctrl Pts',(6.9,1.83697019872103E-15,30.));
#39868=CARTESIAN_POINT('Ctrl Pts',(6.9,-30.,30.));
#39869=CARTESIAN_POINT('Ctrl Pts',(6.9,-30.,1.83697019872103E-15));
#39870=CARTESIAN_POINT('Ctrl Pts',(6.9,-30.,-30.));
#39871=CARTESIAN_POINT('Ctrl Pts',(6.9,-1.83697019872103E-15,-30.));
#39872=CARTESIAN_POINT('Ctrl Pts',(6.9,30.,-30.));
#39873=CARTESIAN_POINT('Ctrl Pts',(6.9,30.,-1.83697019872103E-15));
#39874=CARTESIAN_POINT('Ctrl Pts',(6.9,30.,28.6904764110968));
#39875=CARTESIAN_POINT('Ctrl Pts',(6.9,1.33807601272607,29.9701443537426));
#39876=CARTESIAN_POINT('Ctrl Pts',(6.9,-21.8303175223207,20.5775906479515));
#39877=CARTESIAN_POINT('Ctrl Pts',(7.85773098116326,-20.4889265372406,22.0288565043892));
#39878=CARTESIAN_POINT('Ctrl Pts',(8.88781981167334,-19.0414114324084,23.3171626725998));
#39879=CARTESIAN_POINT('Ctrl Pts',(10.5914578196776,-16.6247285680552,25.1150390010341));
#39880=CARTESIAN_POINT('Ctrl Pts',(11.2365058953701,-15.703976734769,25.7254166302984));
#39881=CARTESIAN_POINT('Ctrl Pts',(12.0558885382926,-14.5853792872662,26.3926147460599));
#39882=CARTESIAN_POINT('Ctrl Pts',(12.1875764958397,-14.4076425286694,26.4963665374952));
#39883=CARTESIAN_POINT('Ctrl Pts',(13.194901830313,-13.0552778456719,27.2691057169114));
#39884=CARTESIAN_POINT('Ctrl Pts',(14.2258982134098,-11.6381637544796,27.991732600527));
#39885=CARTESIAN_POINT('Ctrl Pts',(18.2616480823244,-6.95587410790868,29.9350198014187));
#39886=CARTESIAN_POINT('Ctrl Pts',(21.0496416709525,-4.29983295736294,30.7693084982877));
#39887=CARTESIAN_POINT('Ctrl Pts',(25.8000196361138,-1.93741001991749,32.8040277065106));
#39888=CARTESIAN_POINT('Ctrl Pts',(26.8976561124457,-1.74039351523169,33.3305524688301));
#39889=CARTESIAN_POINT('Ctrl Pts',(28.0045908801237,-1.58669630450145,33.8378020212277));
#39890=CARTESIAN_POINT('Ctrl Pts',(28.5235971652406,-1.54532623843658,34.0754855762016));
#39891=CARTESIAN_POINT('Ctrl Pts',(29.0834839543824,-1.4982885487127,34.3307100593381));
#39892=CARTESIAN_POINT('Ctrl Pts',(29.1146288039499,-1.49562082188434,34.3449058451715));
#39893=CARTESIAN_POINT('Ctrl Pts',(29.5949306848436,-1.45589225448014,34.5637016811193));
#39894=CARTESIAN_POINT('Ctrl Pts',(30.0492939924726,-1.44682754698748,34.7685410859787));
#39895=CARTESIAN_POINT('Ctrl Pts',(30.5,-1.44976976333441,34.9699609326822));
#39896=CARTESIAN_POINT('Ctrl Pts',(6.45331003273164,-8.65286216739172,6.83943894028999));
#39897=CARTESIAN_POINT('Ctrl Pts',(7.20830533428676,-8.29622318255582,7.28712780725476));
#39898=CARTESIAN_POINT('Ctrl Pts',(7.99995511878976,-7.91871702121326,7.7001428520779));
#39899=CARTESIAN_POINT('Ctrl Pts',(9.52825943498397,-7.18271304249705,8.39510948814989));
#39900=CARTESIAN_POINT('Ctrl Pts',(10.4940807594721,-6.69830435523696,8.7864108718328));
#39901=CARTESIAN_POINT('Ctrl Pts',(11.4876274938915,-6.22320820014201,9.12017193389638));
#39902=CARTESIAN_POINT('Ctrl Pts',(12.4303878001112,-5.78075775962483,9.42058964158202));
#39903=CARTESIAN_POINT('Ctrl Pts',(13.3997261751211,-5.32007492151067,9.68640068655135));
#39904=CARTESIAN_POINT('Ctrl Pts',(14.3872053777042,-4.88962379427552,9.90607181050111));
#39905=CARTESIAN_POINT('Ctrl Pts',(15.556163132278,-4.3942725212231,10.1514774675698));
#39906=CARTESIAN_POINT('Ctrl Pts',(16.5289171701813,-3.99001252407697,10.309499502888));
#39907=CARTESIAN_POINT('Ctrl Pts',(18.441690792892,-3.31066676205255,10.5572419303421));
#39908=CARTESIAN_POINT('Ctrl Pts',(19.4166449194874,-2.9827440568927,10.6478584846087));
#39909=CARTESIAN_POINT('Ctrl Pts',(20.8623232387078,-2.58759893430878,10.7551557591785));
#39910=CARTESIAN_POINT('Ctrl Pts',(21.8144303959787,-2.34043714010253,10.8124914939577));
#39911=CARTESIAN_POINT('Ctrl Pts',(22.7818406100989,-2.13287731493684,10.8543222400653));
#39912=CARTESIAN_POINT('Ctrl Pts',(23.3297671905071,-2.0316389093207,10.8753628160501));
#39913=CARTESIAN_POINT('Ctrl Pts',(23.4470348316276,-2.01025275957826,10.8796570477425));
#39914=CARTESIAN_POINT('Ctrl Pts',(23.6811400295324,-1.96865550184816,10.8877908591686));
#39915=CARTESIAN_POINT('Ctrl Pts',(24.094239596771,-1.89823453468209,10.9009196003301));
#39916=CARTESIAN_POINT('Ctrl Pts',(24.6901429177709,-1.80574893003815,10.9167796594793));
#39917=CARTESIAN_POINT('Ctrl Pts',(25.2916165705408,-1.72612415763836,10.9295334868831));
#39918=CARTESIAN_POINT('Ctrl Pts',(25.7739565747927,-1.67150491651973,10.9383070002314));
#39919=CARTESIAN_POINT('Ctrl Pts',(26.0152863105174,-1.64740058814794,10.9422949598257));
#39920=CARTESIAN_POINT('Ctrl Pts',(26.3672928498145,-1.61473834547487,10.94787874029));
#39921=CARTESIAN_POINT('Ctrl Pts',(27.2930496194305,-1.54497298618683,10.9593530234768));
#39922=CARTESIAN_POINT('Ctrl Pts',(28.2854511951053,-1.51980459192319,10.9616448439048));
#39923=CARTESIAN_POINT('Ctrl Pts',(29.2045434923158,-1.49505480423355,10.965198770667));
#39924=CARTESIAN_POINT('Ctrl Pts',(29.5206711976023,-1.48867173691355,10.9661639337506));
#39925=CARTESIAN_POINT('Ctrl Pts',(30.1692097404134,-1.48262317876973,10.9670495493201));
#39926=CARTESIAN_POINT('Ctrl Pts',(31.3135190714371,-1.4864528553831,10.96649000528));
#39927=CARTESIAN_POINT('Ctrl Pts',(32.3203822393921,-1.49996522881633,10.9645683677272));
#39928=CARTESIAN_POINT('Ctrl Pts',(33.1675664922,-1.49997704079034,10.9645708546322));
#39929=CARTESIAN_POINT('Ctrl Pts',(33.4947686467078,-1.49997747170577,10.9645712531308));
#39930=CARTESIAN_POINT('Ctrl Pts',(34.1540868645893,-1.49997908112576,10.9645717353852));
#39931=CARTESIAN_POINT('Ctrl Pts',(34.8114534640785,-1.49998335379094,10.9645734486355));
#39932=CARTESIAN_POINT('Ctrl Pts',(35.7991052695187,-1.49998422299017,10.9645737550385));
#39933=CARTESIAN_POINT('Ctrl Pts',(37.7734889032248,-1.49998916111724,10.9645756745653));
#39934=CARTESIAN_POINT('Ctrl Pts',(39.5833333333333,-1.5,10.9645797934319));
#39935=CARTESIAN_POINT('Ctrl Pts',(40.9,-1.5,10.9645797934319));
#39936=CARTESIAN_POINT('Ctrl Pts',(6.6933875035574,-11.7835517019943,10.176216978544));
#39937=CARTESIAN_POINT('Ctrl Pts',(7.45057679732275,-11.2512208468221,10.7852657388529));
#39938=CARTESIAN_POINT('Ctrl Pts',(8.2413121575229,-10.6930046754631,11.3436596611095));
#39939=CARTESIAN_POINT('Ctrl Pts',(9.76826989623895,-9.61265036078123,12.2763196346049));
#39940=CARTESIAN_POINT('Ctrl Pts',(10.7329606123233,-8.90528802461967,12.797808932554));
#39941=CARTESIAN_POINT('Ctrl Pts',(11.7232269898393,-8.21708628846332,13.2363397818143));
#39942=CARTESIAN_POINT('Ctrl Pts',(12.6618589495312,-7.57719783124145,13.6303705734608));
#39943=CARTESIAN_POINT('Ctrl Pts',(13.62938101007,-6.91168434311037,13.9766495525684));
#39944=CARTESIAN_POINT('Ctrl Pts',(14.6088313783793,-6.29602822290691,14.2570519664642));
#39945=CARTESIAN_POINT('Ctrl Pts',(15.7681704150403,-5.5877427072411,14.570157055854));
#39946=CARTESIAN_POINT('Ctrl Pts',(16.7369555416689,-5.00954692132628,14.767994500732));
#39947=CARTESIAN_POINT('Ctrl Pts',(18.6242750358685,-4.04747101384392,15.072833876247));
#39948=CARTESIAN_POINT('Ctrl Pts',(19.5932251737343,-3.58155807753862,15.1807788814753));
#39949=CARTESIAN_POINT('Ctrl Pts',(21.0118923342793,-3.02625583363473,15.3069309857053));
#39950=CARTESIAN_POINT('Ctrl Pts',(21.9540630652681,-2.67707795507692,15.3728356386159));
#39951=CARTESIAN_POINT('Ctrl Pts',(22.9024384113963,-2.38630901256787,15.4189810434881));
#39952=CARTESIAN_POINT('Ctrl Pts',(23.4384834214784,-2.24465775851538,15.4424563702175));
#39953=CARTESIAN_POINT('Ctrl Pts',(23.5542447038724,-2.2145633523891,15.4472367652768));
#39954=CARTESIAN_POINT('Ctrl Pts',(23.78465432169,-2.15615095063381,15.4562082859198));
#39955=CARTESIAN_POINT('Ctrl Pts',(24.1912813672913,-2.0572689135757,15.4705057473596));
#39956=CARTESIAN_POINT('Ctrl Pts',(24.7767883762699,-1.92760629035867,15.487334852315));
#39957=CARTESIAN_POINT('Ctrl Pts',(25.36654130234,-1.81617759528126,15.5005605148525));
#39958=CARTESIAN_POINT('Ctrl Pts',(25.8384861976413,-1.73988825246362,15.5096611552857));
#39959=CARTESIAN_POINT('Ctrl Pts',(26.0742971451332,-1.70625267454512,15.5138439934012));
#39960=CARTESIAN_POINT('Ctrl Pts',(26.4178590548908,-1.66071842408642,15.5197632302621));
#39961=CARTESIAN_POINT('Ctrl Pts',(27.3173215852521,-1.563674416307,15.5317592244184));
#39962=CARTESIAN_POINT('Ctrl Pts',(28.3008974271582,-1.52789332168387,15.5336084019203));
#39963=CARTESIAN_POINT('Ctrl Pts',(29.2205106969984,-1.49282313901989,15.5372361675902));
#39964=CARTESIAN_POINT('Ctrl Pts',(29.5297893441341,-1.48392111804966,15.5382211183205));
#39965=CARTESIAN_POINT('Ctrl Pts',(30.1710603648191,-1.47539843727042,15.5391260510599));
#39966=CARTESIAN_POINT('Ctrl Pts',(31.3058674630461,-1.48078221272374,15.5385594105444));
#39967=CARTESIAN_POINT('Ctrl Pts',(32.3149674119483,-1.49994719631519,15.5366091538308));
#39968=CARTESIAN_POINT('Ctrl Pts',(33.1687991060451,-1.49996649944875,15.5366148440523));
#39969=CARTESIAN_POINT('Ctrl Pts',(33.4951825987405,-1.49996690229146,15.5366157560837));
#39970=CARTESIAN_POINT('Ctrl Pts',(34.1549121057911,-1.49996939198939,15.5366168596277));
#39971=CARTESIAN_POINT('Ctrl Pts',(34.8118777623806,-1.49997557765831,15.5366207802977));
#39972=CARTESIAN_POINT('Ctrl Pts',(35.7995932556016,-1.49997687727485,15.5366214814653));
#39973=CARTESIAN_POINT('Ctrl Pts',(37.7737223043124,-1.49998408565139,15.536625874162));
#39974=CARTESIAN_POINT('Ctrl Pts',(39.5833333333333,-1.5,15.5366352998475));
#39975=CARTESIAN_POINT('Ctrl Pts',(40.9,-1.5,15.5366352998475));
#39976=CARTESIAN_POINT('Ctrl Pts',(6.84856199327287,-17.3015601300326,15.9756656267856));
#39977=CARTESIAN_POINT('Ctrl Pts',(7.6163426075982,-16.4542577625343,16.880477206766));
#39978=CARTESIAN_POINT('Ctrl Pts',(8.41867777462062,-15.5717695685564,17.7014911506025));
#39979=CARTESIAN_POINT('Ctrl Pts',(9.96113195955868,-13.8764580517237,19.0620073137526));
#39980=CARTESIAN_POINT('Ctrl Pts',(10.9332800166621,-12.7736673235567,19.815224791801));
#39981=CARTESIAN_POINT('Ctrl Pts',(11.9367963602557,-11.6987467748375,20.4447687021717));
#39982=CARTESIAN_POINT('Ctrl Pts',(12.8867814792929,-10.7022950266451,21.0075672609871));
#39983=CARTESIAN_POINT('Ctrl Pts',(13.8590496672151,-9.67539612019949,21.4943962460795));
#39984=CARTESIAN_POINT('Ctrl Pts',(14.8485921349356,-8.72431608662546,21.884054887486));
#39985=CARTESIAN_POINT('Ctrl Pts',(16.0163007294256,-7.63455433184466,22.3166578360873));
#39986=CARTESIAN_POINT('Ctrl Pts',(16.9884569437496,-6.75057879345238,22.5821364755291));
#39987=CARTESIAN_POINT('Ctrl Pts',(18.8739644427958,-5.29110974776816,22.9841384147108));
#39988=CARTESIAN_POINT('Ctrl Pts',(19.8410528812574,-4.58570965781586,23.1201648771934));
#39989=CARTESIAN_POINT('Ctrl Pts',(21.2381152642979,-3.75822630090649,23.2766545601846));
#39990=CARTESIAN_POINT('Ctrl Pts',(22.1709482299956,-3.23413242036785,23.3562489404792));
#39991=CARTESIAN_POINT('Ctrl Pts',(23.0969226589074,-2.80482604568844,23.4088332599271));
#39992=CARTESIAN_POINT('Ctrl Pts',(23.6167257768698,-2.59669919378737,23.436097008432));
#39993=CARTESIAN_POINT('Ctrl Pts',(23.7304440861555,-2.55187487879195,23.4416610185368));
#39994=CARTESIAN_POINT('Ctrl Pts',(23.9557382879883,-2.46529344501871,23.4519564031388));
#39995=CARTESIAN_POINT('Ctrl Pts',(24.3531769354774,-2.3187667506293,23.4680750466195));
#39996=CARTESIAN_POINT('Ctrl Pts',(24.9232265691605,-2.12735895816067,23.4863293251813));
#39997=CARTESIAN_POINT('Ctrl Pts',(25.4945991725924,-1.96359000545671,23.5001927499934));
#39998=CARTESIAN_POINT('Ctrl Pts',(25.9497700202409,-1.8518994638432,23.5097714589304));
#39999=CARTESIAN_POINT('Ctrl Pts',(26.176473840736,-1.80278336268422,23.5142578389004));
#40000=CARTESIAN_POINT('Ctrl Pts',(26.5059907605108,-1.73643358900275,23.5207181203645));
#40001=CARTESIAN_POINT('Ctrl Pts',(27.3606430706766,-1.59579143734496,23.5335529917322));
#40002=CARTESIAN_POINT('Ctrl Pts',(28.328238250736,-1.54133580528123,23.5346127004849));
#40003=CARTESIAN_POINT('Ctrl Pts',(29.2487071190625,-1.48828577636564,23.5383515936462));
#40004=CARTESIAN_POINT('Ctrl Pts',(29.5460132431354,-1.47529943899978,23.5393690406291));
#40005=CARTESIAN_POINT('Ctrl Pts',(30.1745409675272,-1.46257298770338,23.5403036706459));
#40006=CARTESIAN_POINT('Ctrl Pts',(31.2926891957807,-1.47061513008709,23.5397184432942));
#40007=CARTESIAN_POINT('Ctrl Pts',(32.3056292653037,-1.49977993503654,23.5377052457532));
#40008=CARTESIAN_POINT('Ctrl Pts',(33.171063928526,-1.49984576464778,23.53771116989));
#40009=CARTESIAN_POINT('Ctrl Pts',(33.4960099678507,-1.49985013662889,23.5377121171257));
#40010=CARTESIAN_POINT('Ctrl Pts',(34.1564534126615,-1.49986002424299,23.5377132649686));
#40011=CARTESIAN_POINT('Ctrl Pts',(34.8126967694548,-1.4998890457023,23.5377173407623));
#40012=CARTESIAN_POINT('Ctrl Pts',(35.8005200217607,-1.49989467989925,23.5377180698364));
#40013=CARTESIAN_POINT('Ctrl Pts',(37.7741804086525,-1.4999278336931,23.5377226365692));
#40014=CARTESIAN_POINT('Ctrl Pts',(39.5833333333333,-1.5,23.5377324360749));
#40015=CARTESIAN_POINT('Ctrl Pts',(40.9,-1.5,23.5377324360749));
#40016=CARTESIAN_POINT('Ctrl Pts',(6.91525560456497,-22.9100322970705,21.6832437463415));
#40017=CARTESIAN_POINT('Ctrl Pts',(7.68680828807946,-21.7506407559596,22.8901115475878));
#40018=CARTESIAN_POINT('Ctrl Pts',(8.49254333196796,-20.5454520608109,23.9817021083909));
#40019=CARTESIAN_POINT('Ctrl Pts',(10.0410868869421,-18.2355476030532,25.783436835301));
#40020=CARTESIAN_POINT('Ctrl Pts',(11.0156330688494,-16.7381286127845,26.7761285175838));
#40021=CARTESIAN_POINT('Ctrl Pts',(12.0267774787436,-15.2694195930957,27.6065335630864));
#40022=CARTESIAN_POINT('Ctrl Pts',(12.9837665933316,-13.9090077888112,28.3472037410707));
#40023=CARTESIAN_POINT('Ctrl Pts',(13.9582748251365,-12.5185550738456,28.9806054990946));
#40024=CARTESIAN_POINT('Ctrl Pts',(14.9579439087574,-11.2181255435619,29.4879275336708));
#40025=CARTESIAN_POINT('Ctrl Pts',(16.1360231813382,-9.73182073292782,30.0486109782393));
#40026=CARTESIAN_POINT('Ctrl Pts',(17.1125926236779,-8.53469955955227,30.3858860137637));
#40027=CARTESIAN_POINT('Ctrl Pts',(19.0161910165423,-6.54807207599635,30.893375381823));
#40028=CARTESIAN_POINT('Ctrl Pts',(19.9877676407317,-5.59579046139741,31.0588212358041));
#40029=CARTESIAN_POINT('Ctrl Pts',(21.3909461476618,-4.48020211813739,31.2474019180858));
#40030=CARTESIAN_POINT('Ctrl Pts',(22.3248563284891,-3.77659408112775,31.3408522311969));
#40031=CARTESIAN_POINT('Ctrl Pts',(23.2468923217639,-3.20514337922215,31.3997620359148));
#40032=CARTESIAN_POINT('Ctrl Pts',(23.7601739654543,-2.93082137010623,31.430627683656));
#40033=CARTESIAN_POINT('Ctrl Pts',(23.8730573072336,-2.87131241748073,31.4369365823338));
#40034=CARTESIAN_POINT('Ctrl Pts',(24.0961287002213,-2.75675829411561,31.4484760107116));
#40035=CARTESIAN_POINT('Ctrl Pts',(24.4892033184452,-2.56315742515059,31.4662740955766));
#40036=CARTESIAN_POINT('Ctrl Pts',(25.0507326849357,-2.31155892021077,31.4857535994475));
#40037=CARTESIAN_POINT('Ctrl Pts',(25.6099642666879,-2.09799811072266,31.5000858680305));
#40038=CARTESIAN_POINT('Ctrl Pts',(26.0526717556216,-1.95341986226856,31.5100364612848));
#40039=CARTESIAN_POINT('Ctrl Pts',(26.2721174193034,-1.89019302484359,31.5147848140591));
#40040=CARTESIAN_POINT('Ctrl Pts',(26.5900938789433,-1.80510164023555,31.5217327388238));
#40041=CARTESIAN_POINT('Ctrl Pts',(27.4046313185694,-1.62683363158072,31.5353204657088));
#40042=CARTESIAN_POINT('Ctrl Pts',(28.3551551181953,-1.55385623211788,31.5356158769573));
#40043=CARTESIAN_POINT('Ctrl Pts',(29.2766284588593,-1.48285998465491,31.5394629693118));
#40044=CARTESIAN_POINT('Ctrl Pts',(29.5620749777487,-1.46634178597095,31.5405133739895));
#40045=CARTESIAN_POINT('Ctrl Pts',(30.1778667116529,-1.44961397315314,31.5414782418285));
#40046=CARTESIAN_POINT('Ctrl Pts',(31.2793924730891,-1.46018163281271,31.5408746533112));
#40047=CARTESIAN_POINT('Ctrl Pts',(32.2962077526077,-1.49947992165247,31.5387996004541));
#40048=CARTESIAN_POINT('Ctrl Pts',(33.1732631913448,-1.49962796113082,31.5388061398229));
#40049=CARTESIAN_POINT('Ctrl Pts',(33.4967747473349,-1.49963968162193,31.538807182264));
#40050=CARTESIAN_POINT('Ctrl Pts',(34.1579356372808,-1.49966279717681,31.5388084478368));
#40051=CARTESIAN_POINT('Ctrl Pts',(34.813469269944,-1.49973305460827,31.5388129385369));
#40052=CARTESIAN_POINT('Ctrl Pts',(35.8014025220136,-1.49974648220053,31.5388137420569));
#40053=CARTESIAN_POINT('Ctrl Pts',(37.7746083248076,-1.49982643859215,31.5388187740001));
#40054=CARTESIAN_POINT('Ctrl Pts',(39.5833333333333,-1.5,31.5388295723023));
#40055=CARTESIAN_POINT('Ctrl Pts',(40.9,-1.5,31.5388295723023));
#40056=CARTESIAN_POINT('Ctrl Pts',(6.93528330520032,-25.3195110382618,24.1234099037007));
#40057=CARTESIAN_POINT('Ctrl Pts',(7.70864561497005,-24.0266258397084,25.4600205488393));
#40058=CARTESIAN_POINT('Ctrl Pts',(8.51562113079159,-22.683454927525,26.6679288641754));
#40059=CARTESIAN_POINT('Ctrl Pts',(10.0666374697795,-20.1106380333435,28.6593492285767));
#40060=CARTESIAN_POINT('Ctrl Pts',(11.042032006318,-18.4443560472,29.7550958483524));
#40061=CARTESIAN_POINT('Ctrl Pts',(12.0563101934605,-16.8071578945887,30.6719165802071));
#40062=CARTESIAN_POINT('Ctrl Pts',(13.0160460695303,-15.29096142786,31.4891825490877));
#40063=CARTESIAN_POINT('Ctrl Pts',(13.9913179180522,-13.7448072814026,32.1858307461017));
#40064=CARTESIAN_POINT('Ctrl Pts',(14.9948977569346,-12.2946331064003,32.7439647444974));
#40065=CARTESIAN_POINT('Ctrl Pts',(16.1769113040285,-10.6381684618929,33.3600488616169));
#40066=CARTESIAN_POINT('Ctrl Pts',(17.1550702558646,-9.30667068355118,33.7285091938727));
#40067=CARTESIAN_POINT('Ctrl Pts',(19.0659094948408,-7.09221287605646,34.2820742196266));
#40068=CARTESIAN_POINT('Ctrl Pts',(20.0392998042888,-6.03343331328744,34.4604355518963));
#40069=CARTESIAN_POINT('Ctrl Pts',(21.4463900864313,-4.79170617358831,34.6632094821159));
#40070=CARTESIAN_POINT('Ctrl Pts',(22.3814014849328,-4.01016373038329,34.7627470812904));
#40071=CARTESIAN_POINT('Ctrl Pts',(23.3035439511912,-3.37628406315923,34.8244714644531));
#40072=CARTESIAN_POINT('Ctrl Pts',(23.8153199893244,-3.07301749249811,34.8569024326816));
#40073=CARTESIAN_POINT('Ctrl Pts',(23.9280059115487,-3.00714498962961,34.8635321227254));
#40074=CARTESIAN_POINT('Ctrl Pts',(24.1505233346922,-2.88044612076907,34.8756078808959));
#40075=CARTESIAN_POINT('Ctrl Pts',(24.5424299687223,-2.66644368612956,34.8941271156085));
#40076=CARTESIAN_POINT('Ctrl Pts',(25.1014254054398,-2.38883635621612,34.914125424837));
#40077=CARTESIAN_POINT('Ctrl Pts',(25.6566063651091,-2.1539516173883,34.9286453169304));
#40078=CARTESIAN_POINT('Ctrl Pts',(26.0948392448068,-1.99544031319315,34.938744218721));
#40079=CARTESIAN_POINT('Ctrl Pts',(26.3115689572165,-1.92629671309846,34.9435997527764));
#40080=CARTESIAN_POINT('Ctrl Pts',(26.6251471538059,-1.83339663912719,34.9507497717891));
#40081=CARTESIAN_POINT('Ctrl Pts',(27.4236115182935,-1.63986518992209,34.9646466630656));
#40082=CARTESIAN_POINT('Ctrl Pts',(28.3665836197148,-1.55906444107099,34.9646176398389));
#40083=CARTESIAN_POINT('Ctrl Pts',(29.2885219356023,-1.48037458462995,34.9685105141258));
#40084=CARTESIAN_POINT('Ctrl Pts',(29.5689154366503,-1.46244305203796,34.9695750902676));
#40085=CARTESIAN_POINT('Ctrl Pts',(30.1792507153713,-1.44403741340358,34.9705529766509));
#40086=CARTESIAN_POINT('Ctrl Pts',(31.2736623104601,-1.45566276263915,34.9699414890844));
#40087=CARTESIAN_POINT('Ctrl Pts',(32.2921477181609,-1.49932800272566,34.9678399885732));
#40088=CARTESIAN_POINT('Ctrl Pts',(33.1741882479305,-1.499517595871,34.9678468028527));
#40089=CARTESIAN_POINT('Ctrl Pts',(33.4970858163865,-1.49953305131999,34.967847887745));
#40090=CARTESIAN_POINT('Ctrl Pts',(34.1585551188942,-1.49956286264318,34.9678492058823));
#40091=CARTESIAN_POINT('Ctrl Pts',(34.813787937747,-1.49965401758262,34.9678538817401));
#40092=CARTESIAN_POINT('Ctrl Pts',(35.8017689303045,-1.49967139266818,34.9678547184894));
#40093=CARTESIAN_POINT('Ctrl Pts',(37.7747836658544,-1.49977506469251,34.9678599580489));
#40094=CARTESIAN_POINT('Ctrl Pts',(39.5833333333333,-1.5,34.967871202114));
#40095=CARTESIAN_POINT('Ctrl Pts',(40.9,-1.5,34.967871202114));
#40096=CARTESIAN_POINT('Origin',(6.9,15.,25.9807621135332));
#40097=CARTESIAN_POINT('',(6.9,-8.61681422303453,28.7358750109634));
#40098=CARTESIAN_POINT('Ctrl Pts',(6.9,-3.76156693666918,10.3676856018661));
#40099=CARTESIAN_POINT('Ctrl Pts',(6.9,-4.66834435251376,14.103554168739));
#40100=CARTESIAN_POINT('Ctrl Pts',(6.90000000166257,-5.7030525211077,18.0191477848531));
#40101=CARTESIAN_POINT('Ctrl Pts',(6.90000000166257,-7.22296038005706,23.666490663791));
#40102=CARTESIAN_POINT('Ctrl Pts',(6.9,-7.92134750786926,26.2182182108371));
#40103=CARTESIAN_POINT('Ctrl Pts',(6.9,-8.61681422303453,28.7358750109634));
#40104=CARTESIAN_POINT('Origin',(6.9,0.,0.));
#40105=CARTESIAN_POINT('Origin',(40.9,4.5,7.79422863405995));
#40106=CARTESIAN_POINT('Ctrl Pts',(40.9,15.9346498339374,30.5996231131986));
#40107=CARTESIAN_POINT('Ctrl Pts',(40.9,15.6844024313584,30.1661818974695));
#40108=CARTESIAN_POINT('Ctrl Pts',(40.9,15.4341550287793,29.7327406817405));
#40109=CARTESIAN_POINT('Ctrl Pts',(40.9,15.1839076262003,29.2992994660114));
#40110=CARTESIAN_POINT('Ctrl Pts',(30.5,18.8345266621011,29.5001797522422));
#40111=CARTESIAN_POINT('Ctrl Pts',(30.5,18.176307754627,29.9204226682664));
#40112=CARTESIAN_POINT('Ctrl Pts',(30.5,17.5,30.3108891324554));
#40113=CARTESIAN_POINT('Ctrl Pts',(30.5,-12.8108891324553,47.8108891324553));
#40114=CARTESIAN_POINT('Ctrl Pts',(30.5,-30.3108891324554,17.5));
#40115=CARTESIAN_POINT('Ctrl Pts',(30.5,-47.8108891324553,-12.8108891324553));
#40116=CARTESIAN_POINT('Ctrl Pts',(30.5,-17.5,-30.3108891324554));
#40117=CARTESIAN_POINT('Ctrl Pts',(30.5,12.8108891324553,-47.8108891324553));
#40118=CARTESIAN_POINT('Ctrl Pts',(30.5,30.3108891324554,-17.5));
#40119=CARTESIAN_POINT('Ctrl Pts',(30.5,47.0470003722618,11.4877949884694));
#40120=CARTESIAN_POINT('Ctrl Pts',(30.5,18.8345266621011,29.5001797522422));
#40121=CARTESIAN_POINT('Ctrl Pts',(30.3311478274255,18.7939298193791,29.4365936489566));
#40122=CARTESIAN_POINT('Ctrl Pts',(30.3311478274255,18.1371296685291,29.8559307532302));
#40123=CARTESIAN_POINT('Ctrl Pts',(30.3311478274255,17.4622796600955,30.245555587262));
#40124=CARTESIAN_POINT('Ctrl Pts',(30.3311478274255,-12.7832759271665,47.7078352473574));
#40125=CARTESIAN_POINT('Ctrl Pts',(30.3311478274255,-30.245555587262,17.4622796600955));
#40126=CARTESIAN_POINT('Ctrl Pts',(30.3311478274255,-47.7078352473574,-12.7832759271665));
#40127=CARTESIAN_POINT('Ctrl Pts',(30.3311478274255,-17.4622796600955,-30.245555587262));
#40128=CARTESIAN_POINT('Ctrl Pts',(30.3311478274255,12.7832759271665,-47.7078352473574));
#40129=CARTESIAN_POINT('Ctrl Pts',(30.3311478274255,30.245555587262,-17.4622796600955));
#40130=CARTESIAN_POINT('Ctrl Pts',(30.3311478274255,46.9455930096601,11.4630336437998));
#40131=CARTESIAN_POINT('Ctrl Pts',(30.3311478274255,18.7939298193791,29.4365936489566));
#40132=CARTESIAN_POINT('Ctrl Pts',(29.9897712690917,18.7116961278613,29.3077924996107));
#40133=CARTESIAN_POINT('Ctrl Pts',(29.9897712690917,18.0577698358324,29.7252947753835));
#40134=CARTESIAN_POINT('Ctrl Pts',(29.9897712690917,17.3858726641896,30.1132147882992));
#40135=CARTESIAN_POINT('Ctrl Pts',(29.9897712690917,-12.7273421241096,47.4990874524888));
#40136=CARTESIAN_POINT('Ctrl Pts',(29.9897712690917,-30.1132147882992,17.3858726641896));
#40137=CARTESIAN_POINT('Ctrl Pts',(29.9897712690917,-47.4990874524888,-12.7273421241096));
#40138=CARTESIAN_POINT('Ctrl Pts',(29.9897712690917,-17.3858726641896,-30.1132147882992));
#40139=CARTESIAN_POINT('Ctrl Pts',(29.9897712690917,12.7273421241096,-47.4990874524888));
#40140=CARTESIAN_POINT('Ctrl Pts',(29.9897712690917,30.1132147882992,-17.3858726641896));
#40141=CARTESIAN_POINT('Ctrl Pts',(29.9897712690917,46.7401804402414,11.4128766206768));
#40142=CARTESIAN_POINT('Ctrl Pts',(29.9897712690917,18.7116961278613,29.3077924996107));
#40143=CARTESIAN_POINT('Ctrl Pts',(29.4666899049319,18.5852252487451,29.1097034403905));
#40144=CARTESIAN_POINT('Ctrl Pts',(29.4666899049319,17.935718792976,29.5243838511923));
#40145=CARTESIAN_POINT('Ctrl Pts',(29.4666899049319,17.2683629213518,29.9096819433198));
#40146=CARTESIAN_POINT('Ctrl Pts',(29.4666899049319,-12.641319021968,47.1780448646716));
#40147=CARTESIAN_POINT('Ctrl Pts',(29.4666899049319,-29.9096819433198,17.2683629213518));
#40148=CARTESIAN_POINT('Ctrl Pts',(29.4666899049319,-47.1780448646716,-12.641319021968));
#40149=CARTESIAN_POINT('Ctrl Pts',(29.4666899049319,-17.2683629213518,-29.9096819433198));
#40150=CARTESIAN_POINT('Ctrl Pts',(29.4666899049319,12.641319021968,-47.1780448646716));
#40151=CARTESIAN_POINT('Ctrl Pts',(29.4666899049319,29.9096819433198,-17.2683629213518));
#40152=CARTESIAN_POINT('Ctrl Pts',(29.4666899049319,46.4242672450966,11.3357378872558));
#40153=CARTESIAN_POINT('Ctrl Pts',(29.4666899049319,18.5852252487451,29.1097034403905));
#40154=CARTESIAN_POINT('Ctrl Pts',(28.7471241621752,18.4103340474916,28.8357745030392));
#40155=CARTESIAN_POINT('Ctrl Pts',(28.7471241621752,17.7669395953572,29.246552676757));
#40156=CARTESIAN_POINT('Ctrl Pts',(28.7471241621752,17.105863694435,29.6282250261092));
#40157=CARTESIAN_POINT('Ctrl Pts',(28.7471241621752,-12.5223613316743,46.7340887205442));
#40158=CARTESIAN_POINT('Ctrl Pts',(28.7471241621752,-29.6282250261092,17.105863694435));
#40159=CARTESIAN_POINT('Ctrl Pts',(28.7471241621752,-46.7340887205442,-12.5223613316743));
#40160=CARTESIAN_POINT('Ctrl Pts',(28.7471241621752,-17.105863694435,-29.6282250261092));
#40161=CARTESIAN_POINT('Ctrl Pts',(28.7471241621752,12.5223613316743,-46.7340887205442));
#40162=CARTESIAN_POINT('Ctrl Pts',(28.7471241621752,29.6282250261092,-17.105863694435));
#40163=CARTESIAN_POINT('Ctrl Pts',(28.7471241621752,45.9874043199967,11.2290660127069));
#40164=CARTESIAN_POINT('Ctrl Pts',(28.7471241621752,18.4103340474916,28.8357745030392));
#40165=CARTESIAN_POINT('Ctrl Pts',(27.8100958442934,18.1817092625453,28.4776836217162));
#40166=CARTESIAN_POINT('Ctrl Pts',(27.8100958442934,17.5463046664274,28.8833606347823));
#40167=CARTESIAN_POINT('Ctrl Pts',(27.8100958442934,16.8934381948013,29.2602932679205));
#40168=CARTESIAN_POINT('Ctrl Pts',(27.8100958442934,-12.3668550731192,46.1537314627218));
#40169=CARTESIAN_POINT('Ctrl Pts',(27.8100958442934,-29.2602932679205,16.8934381948013));
#40170=CARTESIAN_POINT('Ctrl Pts',(27.8100958442934,-46.1537314627218,-12.3668550731192));
#40171=CARTESIAN_POINT('Ctrl Pts',(27.8100958442934,-16.8934381948013,-29.2602932679205));
#40172=CARTESIAN_POINT('Ctrl Pts',(27.8100958442934,12.3668550731192,-46.1537314627218));
#40173=CARTESIAN_POINT('Ctrl Pts',(27.8100958442934,29.2602932679205,-16.8934381948013));
#40174=CARTESIAN_POINT('Ctrl Pts',(27.8100958442934,45.4163196022628,11.0896202647003));
#40175=CARTESIAN_POINT('Ctrl Pts',(27.8100958442934,18.1817092625453,28.4776836217162));
#40176=CARTESIAN_POINT('Ctrl Pts',(26.8343111708818,17.9446806017473,28.1064299010669));
#40177=CARTESIAN_POINT('Ctrl Pts',(26.8343111708818,17.3175595557791,28.5068182430991));
#40178=CARTESIAN_POINT('Ctrl Pts',(26.8343111708818,16.6732042787395,28.8788369357517));
#40179=CARTESIAN_POINT('Ctrl Pts',(26.8343111708818,-12.2056326570121,45.5520412144912));
#40180=CARTESIAN_POINT('Ctrl Pts',(26.8343111708818,-28.8788369357517,16.6732042787395));
#40181=CARTESIAN_POINT('Ctrl Pts',(26.8343111708818,-45.5520412144912,-12.2056326570121));
#40182=CARTESIAN_POINT('Ctrl Pts',(26.8343111708818,-16.6732042787395,-28.8788369357517));
#40183=CARTESIAN_POINT('Ctrl Pts',(26.8343111708818,12.2056326570121,-45.5520412144912));
#40184=CARTESIAN_POINT('Ctrl Pts',(26.8343111708818,28.8788369357517,-16.6732042787395));
#40185=CARTESIAN_POINT('Ctrl Pts',(26.8343111708818,44.8242427376375,10.9450487174303));
#40186=CARTESIAN_POINT('Ctrl Pts',(26.8343111708818,17.9446806017473,28.1064299010669));
#40187=CARTESIAN_POINT('Ctrl Pts',(25.8181479469611,17.7025946652472,27.7272550606068));
#40188=CARTESIAN_POINT('Ctrl Pts',(25.8181479469611,17.0839339083798,28.1222418918016));
#40189=CARTESIAN_POINT('Ctrl Pts',(25.8181479469611,16.4482714219305,28.4892417994669));
#40190=CARTESIAN_POINT('Ctrl Pts',(25.8181479469611,-12.0409703775363,44.9375132213974));
#40191=CARTESIAN_POINT('Ctrl Pts',(25.8181479469611,-28.4892417994669,16.4482714219305));
#40192=CARTESIAN_POINT('Ctrl Pts',(25.8181479469611,-44.9375132213974,-12.0409703775363));
#40193=CARTESIAN_POINT('Ctrl Pts',(25.8181479469611,-16.4482714219305,-28.4892417994669));
#40194=CARTESIAN_POINT('Ctrl Pts',(25.8181479469611,12.0409703775363,-44.9375132213974));
#40195=CARTESIAN_POINT('Ctrl Pts',(25.8181479469611,28.4892417994669,-16.4482714219305));
#40196=CARTESIAN_POINT('Ctrl Pts',(25.8181479469611,44.2195332406074,10.7973925719907));
#40197=CARTESIAN_POINT('Ctrl Pts',(25.8181479469611,17.7025946652472,27.7272550606068));
#40198=CARTESIAN_POINT('Ctrl Pts',(24.7595197917227,17.4614959928472,27.3496265541183));
#40199=CARTESIAN_POINT('Ctrl Pts',(24.7595197917227,16.8512610227058,27.739233902677));
#40200=CARTESIAN_POINT('Ctrl Pts',(24.7595197917227,16.2242558762949,28.1012354927406));
#40201=CARTESIAN_POINT('Ctrl Pts',(24.7595197917227,-11.8769796164457,44.3254913690355));
#40202=CARTESIAN_POINT('Ctrl Pts',(24.7595197917227,-28.1012354927406,16.2242558762949));
#40203=CARTESIAN_POINT('Ctrl Pts',(24.7595197917227,-44.3254913690355,-11.8769796164457));
#40204=CARTESIAN_POINT('Ctrl Pts',(24.7595197917227,-16.2242558762949,-28.1012354927406));
#40205=CARTESIAN_POINT('Ctrl Pts',(24.7595197917227,11.8769796164457,-44.3254913690355));
#40206=CARTESIAN_POINT('Ctrl Pts',(24.7595197917227,28.1012354927406,-16.2242558762949));
#40207=CARTESIAN_POINT('Ctrl Pts',(24.7595197917227,43.6172898429552,10.6503385912769));
#40208=CARTESIAN_POINT('Ctrl Pts',(24.7595197917227,17.4614959928472,27.3496265541183));
#40209=CARTESIAN_POINT('Ctrl Pts',(23.6563574780851,17.229354682426,26.9860278023044));
#40210=CARTESIAN_POINT('Ctrl Pts',(23.6563574780851,16.627232461942,27.370455528196));
#40211=CARTESIAN_POINT('Ctrl Pts',(23.6563574780851,16.0085630157705,27.7276444994825));
#40212=CARTESIAN_POINT('Ctrl Pts',(23.6563574780851,-11.719081483712,43.736207515253));
#40213=CARTESIAN_POINT('Ctrl Pts',(23.6563574780851,-27.7276444994825,16.0085630157705));
#40214=CARTESIAN_POINT('Ctrl Pts',(23.6563574780851,-43.736207515253,-11.719081483712));
#40215=CARTESIAN_POINT('Ctrl Pts',(23.6563574780851,-16.0085630157705,-27.7276444994825));
#40216=CARTESIAN_POINT('Ctrl Pts',(23.6563574780851,11.719081483712,-43.736207515253));
#40217=CARTESIAN_POINT('Ctrl Pts',(23.6563574780851,27.7276444994825,-16.0085630157705));
#40218=CARTESIAN_POINT('Ctrl Pts',(23.6563574780851,43.0374211521332,10.5087479991523));
#40219=CARTESIAN_POINT('Ctrl Pts',(23.6563574780851,17.229354682426,26.9860278023044));
#40220=CARTESIAN_POINT('Ctrl Pts',(22.5073180101405,17.0145388530744,26.649565639321));
#40221=CARTESIAN_POINT('Ctrl Pts',(22.5073180101405,16.419923900654,27.0292003150791));
#40222=CARTESIAN_POINT('Ctrl Pts',(22.5073180101405,15.8089680335819,27.3819358493961));
#40223=CARTESIAN_POINT('Ctrl Pts',(22.5073180101405,-11.5729678158142,43.190903882978));
#40224=CARTESIAN_POINT('Ctrl Pts',(22.5073180101405,-27.3819358493961,15.8089680335819));
#40225=CARTESIAN_POINT('Ctrl Pts',(22.5073180101405,-43.190903882978,-11.5729678158142));
#40226=CARTESIAN_POINT('Ctrl Pts',(22.5073180101405,-15.8089680335819,-27.3819358493961));
#40227=CARTESIAN_POINT('Ctrl Pts',(22.5073180101405,11.5729678158142,-43.190903882978));
#40228=CARTESIAN_POINT('Ctrl Pts',(22.5073180101405,27.3819358493961,-15.8089680335819));
#40229=CARTESIAN_POINT('Ctrl Pts',(22.5073180101405,42.5008299977716,10.3777247856603));
#40230=CARTESIAN_POINT('Ctrl Pts',(22.5073180101405,17.0145388530744,26.649565639321));
#40231=CARTESIAN_POINT('Ctrl Pts',(21.3125219557939,16.8244723890963,26.3518679613905));
#40232=CARTESIAN_POINT('Ctrl Pts',(21.3125219557939,16.2364997772301,26.727261803997));
#40233=CARTESIAN_POINT('Ctrl Pts',(21.3125219557939,15.632368792237,27.0760569908086));
#40234=CARTESIAN_POINT('Ctrl Pts',(21.3125219557939,-11.4436881985716,42.7084257830456));
#40235=CARTESIAN_POINT('Ctrl Pts',(21.3125219557939,-27.0760569908086,15.632368792237));
#40236=CARTESIAN_POINT('Ctrl Pts',(21.3125219557939,-42.7084257830456,-11.4436881985716));
#40237=CARTESIAN_POINT('Ctrl Pts',(21.3125219557939,-15.632368792237,-27.0760569908086));
#40238=CARTESIAN_POINT('Ctrl Pts',(21.3125219557939,11.4436881985716,-42.7084257830456));
#40239=CARTESIAN_POINT('Ctrl Pts',(21.3125219557939,27.0760569908086,-15.632368792237));
#40240=CARTESIAN_POINT('Ctrl Pts',(21.3125219557939,42.0260605935833,10.2617970211066));
#40241=CARTESIAN_POINT('Ctrl Pts',(21.3125219557939,16.8244723890963,26.3518679613905));
#40242=CARTESIAN_POINT('Ctrl Pts',(20.0742472323676,16.6643225955232,26.1010282252799));
#40243=CARTESIAN_POINT('Ctrl Pts',(20.0742472323676,16.0819468125049,26.4728487465358));
#40244=CARTESIAN_POINT('Ctrl Pts',(20.0742472323676,15.4835664656477,26.8183238008716));
#40245=CARTESIAN_POINT('Ctrl Pts',(20.0742472323676,-11.3347573352238,42.3018902665193));
#40246=CARTESIAN_POINT('Ctrl Pts',(20.0742472323676,-26.8183238008716,15.4835664656477));
#40247=CARTESIAN_POINT('Ctrl Pts',(20.0742472323676,-42.3018902665193,-11.3347573352238));
#40248=CARTESIAN_POINT('Ctrl Pts',(20.0742472323676,-15.4835664656477,-26.8183238008716));
#40249=CARTESIAN_POINT('Ctrl Pts',(20.0742472323676,11.3347573352238,-42.3018902665193));
#40250=CARTESIAN_POINT('Ctrl Pts',(20.0742472323676,26.8183238008716,-15.4835664656477));
#40251=CARTESIAN_POINT('Ctrl Pts',(20.0742472323676,41.6260204156154,10.1641164141543));
#40252=CARTESIAN_POINT('Ctrl Pts',(20.0742472323676,16.6643225955232,26.1010282252799));
#40253=CARTESIAN_POINT('Ctrl Pts',(18.7979917002302,16.5352770548748,25.8989065200918));
#40254=CARTESIAN_POINT('Ctrl Pts',(18.7979917002302,15.9574110860028,26.2678477295776));
#40255=CARTESIAN_POINT('Ctrl Pts',(18.7979917002302,15.3636644897785,26.6106474867381));
#40256=CARTESIAN_POINT('Ctrl Pts',(18.7979917002302,-11.2469829969596,41.9743119765166));
#40257=CARTESIAN_POINT('Ctrl Pts',(18.7979917002302,-26.6106474867381,15.3636644897785));
#40258=CARTESIAN_POINT('Ctrl Pts',(18.7979917002302,-41.9743119765166,-11.2469829969596));
#40259=CARTESIAN_POINT('Ctrl Pts',(18.7979917002302,-15.3636644897785,-26.6106474867381));
#40260=CARTESIAN_POINT('Ctrl Pts',(18.7979917002302,11.2469829969596,-41.9743119765166));
#40261=CARTESIAN_POINT('Ctrl Pts',(18.7979917002302,26.6106474867381,-15.3636644897785));
#40262=CARTESIAN_POINT('Ctrl Pts',(18.7979917002302,41.303675941138,10.0854073102973));
#40263=CARTESIAN_POINT('Ctrl Pts',(18.7979917002302,16.5352770548748,25.8989065200918));
#40264=CARTESIAN_POINT('Ctrl Pts',(17.4917404060759,16.4351406788133,25.7420647185138));
#40265=CARTESIAN_POINT('Ctrl Pts',(17.4917404060759,15.8607742221527,26.1087716481884));
#40266=CARTESIAN_POINT('Ctrl Pts',(17.4917404060759,15.2706233100072,26.4494954361781));
#40267=CARTESIAN_POINT('Ctrl Pts',(17.4917404060759,-11.1788721261709,41.7201187461852));
#40268=CARTESIAN_POINT('Ctrl Pts',(17.4917404060759,-26.4494954361781,15.2706233100072));
#40269=CARTESIAN_POINT('Ctrl Pts',(17.4917404060759,-41.7201187461852,-11.1788721261709));
#40270=CARTESIAN_POINT('Ctrl Pts',(17.4917404060759,-15.2706233100072,-26.4494954361781));
#40271=CARTESIAN_POINT('Ctrl Pts',(17.4917404060759,11.1788721261709,-41.7201187461852));
#40272=CARTESIAN_POINT('Ctrl Pts',(17.4917404060759,26.4494954361781,-15.2706233100072));
#40273=CARTESIAN_POINT('Ctrl Pts',(17.4917404060759,41.0535440314616,10.0243308532288));
#40274=CARTESIAN_POINT('Ctrl Pts',(17.4917404060759,16.4351406788133,25.7420647185138));
#40275=CARTESIAN_POINT('Ctrl Pts',(16.1647270995715,16.3596108683728,25.6237637373094));
#40276=CARTESIAN_POINT('Ctrl Pts',(16.1647270995715,15.7878839869031,25.988785417954));
#40277=CARTESIAN_POINT('Ctrl Pts',(16.1647270995715,15.2004451894511,26.3279433657953));
#40278=CARTESIAN_POINT('Ctrl Pts',(16.1647270995715,-11.1274981763442,41.5283885552464));
#40279=CARTESIAN_POINT('Ctrl Pts',(16.1647270995715,-26.3279433657953,15.2004451894511));
#40280=CARTESIAN_POINT('Ctrl Pts',(16.1647270995715,-41.5283885552464,-11.1274981763442));
#40281=CARTESIAN_POINT('Ctrl Pts',(16.1647270995715,-15.2004451894511,-26.3279433657953));
#40282=CARTESIAN_POINT('Ctrl Pts',(16.1647270995715,11.1274981763442,-41.5283885552464));
#40283=CARTESIAN_POINT('Ctrl Pts',(16.1647270995715,26.3279433657953,-15.2004451894511));
#40284=CARTESIAN_POINT('Ctrl Pts',(16.1647270995715,40.8648771706659,9.9782627468503));
#40285=CARTESIAN_POINT('Ctrl Pts',(16.1647270995715,16.3596108683728,25.6237637373094));
#40286=CARTESIAN_POINT('Ctrl Pts',(14.8263876417415,16.3032840624315,25.5355400760543));
#40287=CARTESIAN_POINT('Ctrl Pts',(14.8263876417415,15.7335256598799,25.8993049721986));
#40288=CARTESIAN_POINT('Ctrl Pts',(14.8263876417415,15.1481094381123,26.2372951854241));
#40289=CARTESIAN_POINT('Ctrl Pts',(14.8263876417415,-11.0891857473118,41.3854046235364));
#40290=CARTESIAN_POINT('Ctrl Pts',(14.8263876417415,-26.2372951854241,15.1481094381123));
#40291=CARTESIAN_POINT('Ctrl Pts',(14.8263876417415,-41.3854046235364,-11.0891857473118));
#40292=CARTESIAN_POINT('Ctrl Pts',(14.8263876417415,-15.1481094381123,-26.2372951854241));
#40293=CARTESIAN_POINT('Ctrl Pts',(14.8263876417415,11.0891857473118,-41.3854046235364));
#40294=CARTESIAN_POINT('Ctrl Pts',(14.8263876417415,26.2372951854241,-15.1481094381123));
#40295=CARTESIAN_POINT('Ctrl Pts',(14.8263876417415,40.7241777356532,9.94390718216753));
#40296=CARTESIAN_POINT('Ctrl Pts',(14.8263876417415,16.3032840624315,25.5355400760543));
#40297=CARTESIAN_POINT('Ctrl Pts',(13.4853470903953,16.260659159851,25.4687774591536));
#40298=CARTESIAN_POINT('Ctrl Pts',(13.4853470903953,15.6923903894686,25.8315912927267));
#40299=CARTESIAN_POINT('Ctrl Pts',(13.4853470903953,15.1085047372063,26.1686978312363));
#40300=CARTESIAN_POINT('Ctrl Pts',(13.4853470903953,-11.06019309403,41.2772025684426));
#40301=CARTESIAN_POINT('Ctrl Pts',(13.4853470903953,-26.1686978312363,15.1085047372063));
#40302=CARTESIAN_POINT('Ctrl Pts',(13.4853470903953,-41.2772025684426,-11.06019309403));
#40303=CARTESIAN_POINT('Ctrl Pts',(13.4853470903953,-15.1085047372063,-26.1686978312363));
#40304=CARTESIAN_POINT('Ctrl Pts',(13.4853470903953,11.06019309403,-41.2772025684426));
#40305=CARTESIAN_POINT('Ctrl Pts',(13.4853470903953,26.1686978312363,-15.1085047372063));
#40306=CARTESIAN_POINT('Ctrl Pts',(13.4853470903953,40.617704456895,9.91790885733394));
#40307=CARTESIAN_POINT('Ctrl Pts',(13.4853470903953,16.260659159851,25.4687774591536));
#40308=CARTESIAN_POINT('Ctrl Pts',(12.1482076787549,16.2272643834928,25.4164718226475));
#40309=CARTESIAN_POINT('Ctrl Pts',(12.1482076787549,15.660162675793,25.778540539635));
#40310=CARTESIAN_POINT('Ctrl Pts',(12.1482076787549,15.0774761588537,26.1149547570431));
#40311=CARTESIAN_POINT('Ctrl Pts',(12.1482076787549,-11.0374785981893,41.1924309158968));
#40312=CARTESIAN_POINT('Ctrl Pts',(12.1482076787549,-26.1149547570431,15.0774761588537));
#40313=CARTESIAN_POINT('Ctrl Pts',(12.1482076787549,-41.1924309158968,-11.0374785981893));
#40314=CARTESIAN_POINT('Ctrl Pts',(12.1482076787549,-15.0774761588537,-26.1149547570431));
#40315=CARTESIAN_POINT('Ctrl Pts',(12.1482076787549,11.0374785981893,-41.1924309158968));
#40316=CARTESIAN_POINT('Ctrl Pts',(12.1482076787549,26.1149547570431,-15.0774761588537));
#40317=CARTESIAN_POINT('Ctrl Pts',(12.1482076787549,40.5342872261919,9.89754028893978));
#40318=CARTESIAN_POINT('Ctrl Pts',(12.1482076787549,16.2272643834928,25.4164718226475));
#40319=CARTESIAN_POINT('Ctrl Pts',(10.8190675759626,16.200195342079,25.3740740708084));
#40320=CARTESIAN_POINT('Ctrl Pts',(10.8190675759626,15.6340396286792,25.7355388133451));
#40321=CARTESIAN_POINT('Ctrl Pts',(10.8190675759626,15.0523251033884,26.0713918511132));
#40322=CARTESIAN_POINT('Ctrl Pts',(10.8190675759626,-11.0190667477248,41.1237169545017));
#40323=CARTESIAN_POINT('Ctrl Pts',(10.8190675759626,-26.0713918511132,15.0523251033884));
#40324=CARTESIAN_POINT('Ctrl Pts',(10.8190675759626,-41.1237169545017,-11.0190667477248));
#40325=CARTESIAN_POINT('Ctrl Pts',(10.8190675759626,-15.0523251033884,-26.0713918511132));
#40326=CARTESIAN_POINT('Ctrl Pts',(10.8190675759626,11.0190667477248,-41.1237169545017));
#40327=CARTESIAN_POINT('Ctrl Pts',(10.8190675759626,26.0713918511132,-15.0523251033884));
#40328=CARTESIAN_POINT('Ctrl Pts',(10.8190675759626,40.4666711281441,9.88102999357243));
#40329=CARTESIAN_POINT('Ctrl Pts',(10.8190675759626,16.200195342079,25.3740740708084));
#40330=CARTESIAN_POINT('Ctrl Pts',(9.50027713254189,16.1776521900286,25.3387651379321));
#40331=CARTESIAN_POINT('Ctrl Pts',(9.50027713254189,15.6122843025816,25.6997268893332));
#40332=CARTESIAN_POINT('Ctrl Pts',(9.50027713254189,15.0313792538877,26.0351125755702));
#40333=CARTESIAN_POINT('Ctrl Pts',(9.50027713254189,-11.0037333216825,41.0664918294579));
#40334=CARTESIAN_POINT('Ctrl Pts',(9.50027713254189,-26.0351125755702,15.0313792538877));
#40335=CARTESIAN_POINT('Ctrl Pts',(9.5002771325419,-41.0664918294579,-11.0037333216825));
#40336=CARTESIAN_POINT('Ctrl Pts',(9.5002771325419,-15.0313792538877,-26.0351125755702));
#40337=CARTESIAN_POINT('Ctrl Pts',(9.5002771325419,11.0037333216825,-41.0664918294579));
#40338=CARTESIAN_POINT('Ctrl Pts',(9.50027713254189,26.0351125755702,-15.0313792538877));
#40339=CARTESIAN_POINT('Ctrl Pts',(9.50027713254189,40.4103603059007,9.86728018643391));
#40340=CARTESIAN_POINT('Ctrl Pts',(9.50027713254189,16.1776521900286,25.3387651379321));
#40341=CARTESIAN_POINT('Ctrl Pts',(8.45435372222587,16.1625070777669,25.3150436214797));
#40342=CARTESIAN_POINT('Ctrl Pts',(8.45435372222587,15.5976684735573,25.6756674495416));
#40343=CARTESIAN_POINT('Ctrl Pts',(8.45435372222587,15.0173072536015,26.0107391561104));
#40344=CARTESIAN_POINT('Ctrl Pts',(8.45435372222587,-10.9934319025089,41.0280464097118));
#40345=CARTESIAN_POINT('Ctrl Pts',(8.45435372222587,-26.0107391561104,15.0173072536015));
#40346=CARTESIAN_POINT('Ctrl Pts',(8.45435372222587,-41.0280464097118,-10.9934319025089));
#40347=CARTESIAN_POINT('Ctrl Pts',(8.45435372222587,-15.0173072536015,-26.0107391561104));
#40348=CARTESIAN_POINT('Ctrl Pts',(8.45435372222587,10.9934319025089,-41.0280464097118));
#40349=CARTESIAN_POINT('Ctrl Pts',(8.45435372222587,26.0107391561104,-15.0173072536015));
#40350=CARTESIAN_POINT('Ctrl Pts',(8.45435372222587,40.3725291400319,9.85804268618444));
#40351=CARTESIAN_POINT('Ctrl Pts',(8.45435372222587,16.1625070777669,25.3150436214797));
#40352=CARTESIAN_POINT('Ctrl Pts',(7.67514864245731,16.1526223715398,25.2995613842179));
#40353=CARTESIAN_POINT('Ctrl Pts',(7.67514864245731,15.5881292127269,25.6599646610633));
#40354=CARTESIAN_POINT('Ctrl Pts',(7.67514864245731,15.0081229315276,25.9948314436454));
#40355=CARTESIAN_POINT('Ctrl Pts',(7.67514864245731,-10.9867085121178,41.0029543751729));
#40356=CARTESIAN_POINT('Ctrl Pts',(7.67514864245731,-25.9948314436454,15.0081229315276));
#40357=CARTESIAN_POINT('Ctrl Pts',(7.67514864245731,-41.0029543751729,-10.9867085121178));
#40358=CARTESIAN_POINT('Ctrl Pts',(7.67514864245731,-15.0081229315276,-25.9948314436454));
#40359=CARTESIAN_POINT('Ctrl Pts',(7.67514864245731,10.9867085121178,-41.0029543751729));
#40360=CARTESIAN_POINT('Ctrl Pts',(7.67514864245731,25.9948314436454,-15.0081229315276));
#40361=CARTESIAN_POINT('Ctrl Pts',(7.67514864245731,40.3478380083732,9.85201367995058));
#40362=CARTESIAN_POINT('Ctrl Pts',(7.67514864245731,16.1526223715398,25.2995613842179));
#40363=CARTESIAN_POINT('Ctrl Pts',(7.15799654185577,16.1466853364124,25.2902623130707));
#40364=CARTESIAN_POINT('Ctrl Pts',(7.15799654185577,15.5823996619098,25.6505331205953));
#40365=CARTESIAN_POINT('Ctrl Pts',(7.15799654185577,15.0026065670023,25.9852768200144));
#40366=CARTESIAN_POINT('Ctrl Pts',(7.15799654185577,-10.9826702530121,40.9878833870167));
#40367=CARTESIAN_POINT('Ctrl Pts',(7.15799654185577,-25.9852768200144,15.0026065670023));
#40368=CARTESIAN_POINT('Ctrl Pts',(7.15799654185577,-40.9878833870167,-10.9826702530121));
#40369=CARTESIAN_POINT('Ctrl Pts',(7.15799654185577,-15.0026065670023,-25.9852768200144));
#40370=CARTESIAN_POINT('Ctrl Pts',(7.15799654185577,10.9826702530121,-40.9878833870167));
#40371=CARTESIAN_POINT('Ctrl Pts',(7.15799654185577,25.9852768200144,-15.0026065670023));
#40372=CARTESIAN_POINT('Ctrl Pts',(7.15799654185577,40.3330078138659,9.84839248767923));
#40373=CARTESIAN_POINT('Ctrl Pts',(7.15799654185577,16.1466853364124,25.2902623130707));
#40374=CARTESIAN_POINT('Ctrl Pts',(6.9,16.1438799960866,25.2858683590648));
#40375=CARTESIAN_POINT('Ctrl Pts',(6.9,15.5796923611089,25.6460765727998));
#40376=CARTESIAN_POINT('Ctrl Pts',(6.9,15.,25.9807621135332));
#40377=CARTESIAN_POINT('Ctrl Pts',(6.9,-10.9807621135332,40.9807621135332));
#40378=CARTESIAN_POINT('Ctrl Pts',(6.9,-25.9807621135332,15.));
#40379=CARTESIAN_POINT('Ctrl Pts',(6.9,-40.9807621135332,-10.9807621135332));
#40380=CARTESIAN_POINT('Ctrl Pts',(6.9,-15.,-25.9807621135332));
#40381=CARTESIAN_POINT('Ctrl Pts',(6.9,10.9807621135332,-40.9807621135332));
#40382=CARTESIAN_POINT('Ctrl Pts',(6.9,25.9807621135332,-15.));
#40383=CARTESIAN_POINT('Ctrl Pts',(6.9,40.3260003190816,9.84668141868804));
#40384=CARTESIAN_POINT('Ctrl Pts',(6.9,16.1438799960866,25.2858683590648));
#40385=CARTESIAN_POINT('Ctrl Pts',(6.9,-8.61681422303453,28.7358750109634));
#40386=CARTESIAN_POINT('Ctrl Pts',(7.85773098116326,-6.72950262532883,29.3220126177434));
#40387=CARTESIAN_POINT('Ctrl Pts',(8.88781981167334,-4.83176468807716,29.7139609348499));
#40388=CARTESIAN_POINT('Ctrl Pts',(10.5914578196776,-1.83991777043967,30.0626260759601));
#40389=CARTESIAN_POINT('Ctrl Pts',(11.2365058953701,-0.737334477600529,
30.1308526921615));
#40390=CARTESIAN_POINT('Ctrl Pts',(12.0558885382926,0.564998386426061,30.1493644860168));
#40391=CARTESIAN_POINT('Ctrl Pts',(12.1875764958397,0.77079883027483,30.1503477937894));
#40392=CARTESIAN_POINT('Ctrl Pts',(13.194901830313,2.32835059063959,30.1433772121647));
#40393=CARTESIAN_POINT('Ctrl Pts',(14.2258982134098,3.91692083548088,30.0606334052373));
#40394=CARTESIAN_POINT('Ctrl Pts',(18.2616480823244,8.94354621773403,29.4024246647732));
#40395=CARTESIAN_POINT('Ctrl Pts',(21.0496416709525,11.660889676038,28.796919295079));
#40396=CARTESIAN_POINT('Ctrl Pts',(25.8000196361138,14.7241675584603,29.3778263502455));
#40397=CARTESIAN_POINT('Ctrl Pts',(26.8976561124457,15.1580512376427,29.7353019177929));
#40398=CARTESIAN_POINT('Ctrl Pts',(28.0045908801237,15.5447817028247,30.0977443108623));
#40399=CARTESIAN_POINT('Ctrl Pts',(28.5235971652406,15.6994510084801,30.2828992744991));
#40400=CARTESIAN_POINT('Ctrl Pts',(29.0834839543824,15.8677990842846,30.4804113157012));
#40401=CARTESIAN_POINT('Ctrl Pts',(29.1146288039499,15.877207296405,30.4913713634453));
#40402=CARTESIAN_POINT('Ctrl Pts',(29.5949306848436,16.0210111630069,30.6609898319163));
#40403=CARTESIAN_POINT('Ctrl Pts',(30.0492939924726,16.1312811324031,30.8338536064743));
#40404=CARTESIAN_POINT('Ctrl Pts',(30.5,16.229443021655,31.0097594187194));
#40405=CARTESIAN_POINT('Ctrl Pts',(6.45331003273164,-4.07387898226151,10.2495589536195));
#40406=CARTESIAN_POINT('Ctrl Pts',(7.20830533428676,-3.54117612793135,10.4589493929845));
#40407=CARTESIAN_POINT('Ctrl Pts',(7.99943720515023,-3.00808536723907,10.6278530262205));
#40408=CARTESIAN_POINT('Ctrl Pts',(9.76195392812149,-1.87226624217412,10.8974188156737));
#40409=CARTESIAN_POINT('Ctrl Pts',(10.7319699357145,-1.2567580486118,10.978614804603));
#40410=CARTESIAN_POINT('Ctrl Pts',(12.6618070777417,-0.165209663835399,
11.0581512103982));
#40411=CARTESIAN_POINT('Ctrl Pts',(13.6366888866736,0.364704064273056,11.0460663569154));
#40412=CARTESIAN_POINT('Ctrl Pts',(15.5563694249501,1.27025231764748,10.9884970038505));
#40413=CARTESIAN_POINT('Ctrl Pts',(16.5294822240035,1.69980161462952,10.9232664847119));
#40414=CARTESIAN_POINT('Ctrl Pts',(18.4405353898675,2.41132585012623,10.79829507883));
#40415=CARTESIAN_POINT('Ctrl Pts',(19.4148048972757,2.74047342809725,10.7128845485964));
#40416=CARTESIAN_POINT('Ctrl Pts',(20.6320159197514,3.07372863623311,10.6248232626626));
#40417=CARTESIAN_POINT('Ctrl Pts',(21.1045081958651,3.19855905527616,10.5890632628362));
#40418=CARTESIAN_POINT('Ctrl Pts',(22.0534615877,3.42883778652053,10.517515820459));
#40419=CARTESIAN_POINT('Ctrl Pts',(22.7823820470183,3.58029681662344,10.4664588970829));
#40420=CARTESIAN_POINT('Ctrl Pts',(23.3297776630268,3.67835397010647,10.4341170945839));
#40421=CARTESIAN_POINT('Ctrl Pts',(23.447059931746,3.69902619132828,10.4271412460568));
#40422=CARTESIAN_POINT('Ctrl Pts',(23.6811266122301,3.73910834650872,10.4133903945396));
#40423=CARTESIAN_POINT('Ctrl Pts',(24.094173095085,3.80664723977494,10.3895545652129));
#40424=CARTESIAN_POINT('Ctrl Pts',(24.6899146335616,3.8946407511,10.3570603924452));
#40425=CARTESIAN_POINT('Ctrl Pts',(25.2912361170961,3.96994444386569,10.3283061836388));
#40426=CARTESIAN_POINT('Ctrl Pts',(25.7735285180352,4.02162740546583,10.3085973054881));
#40427=CARTESIAN_POINT('Ctrl Pts',(26.0148283477101,4.04448759176681,10.3000025859218));
#40428=CARTESIAN_POINT('Ctrl Pts',(26.5981242438445,4.09600397233593,10.2809495486037));
#40429=CARTESIAN_POINT('Ctrl Pts',(27.5413774795631,4.14752077886532,10.2607319091994));
#40430=CARTESIAN_POINT('Ctrl Pts',(28.5384263877915,4.17105255246829,10.2503835882544));
#40431=CARTESIAN_POINT('Ctrl Pts',(29.123550305837,4.18584784382927,10.2444533826691));
#40432=CARTESIAN_POINT('Ctrl Pts',(29.2812719873802,4.18934848102512,10.2430815653884));
#40433=CARTESIAN_POINT('Ctrl Pts',(29.60335738317,4.19465178436656,10.2409825864506));
#40434=CARTESIAN_POINT('Ctrl Pts',(30.1682075695061,4.19956029863434,10.2390432854401));
#40435=CARTESIAN_POINT('Ctrl Pts',(31.3151152846709,4.19601580459666,10.2404426493562));
#40436=CARTESIAN_POINT('Ctrl Pts',(32.3203773995798,4.18330340731804,10.2455622764132));
#40437=CARTESIAN_POINT('Ctrl Pts',(33.1677006908683,4.18329188254759,10.245571342205));
#40438=CARTESIAN_POINT('Ctrl Pts',(33.4949132850991,4.18329063364476,10.2455724350351));
#40439=CARTESIAN_POINT('Ctrl Pts',(34.1541785734608,4.18328832445807,10.2455743198855));
#40440=CARTESIAN_POINT('Ctrl Pts',(34.976129104799,4.18328098024987,10.2455804319184));
#40441=CARTESIAN_POINT('Ctrl Pts',(35.9637295000904,4.18327789132127,10.2455829874647));
#40442=CARTESIAN_POINT('Ctrl Pts',(37.938359040684,4.1832737025367,10.2455864680815));
#40443=CARTESIAN_POINT('Ctrl Pts',(39.5833333333333,4.18325179103929,10.2456046429336));
#40444=CARTESIAN_POINT('Ctrl Pts',(40.9,4.18325179103929,10.2456046429336));
#40445=CARTESIAN_POINT('Ctrl Pts',(6.63336813585096,-4.85602971916217,13.590868440034));
#40446=CARTESIAN_POINT('Ctrl Pts',(7.389696336477,-4.14888858981181,13.8391951107513));
#40447=CARTESIAN_POINT('Ctrl Pts',(8.18053946683774,-3.44401143686368,14.0346488726453));
#40448=CARTESIAN_POINT('Ctrl Pts',(9.94201947683641,-1.94757748540838,14.3333081335907));
#40449=CARTESIAN_POINT('Ctrl Pts',(10.9113717350149,-1.13915583855168,14.4104989873604));
#40450=CARTESIAN_POINT('Ctrl Pts',(12.8347397322171,0.286629408466322,14.4628660834127));
#40451=CARTESIAN_POINT('Ctrl Pts',(13.808142871698,0.978270473832916,14.4226409916871));
#40452=CARTESIAN_POINT('Ctrl Pts',(15.7151185916567,2.15221389622412,14.3061107665235));
#40453=CARTESIAN_POINT('Ctrl Pts',(16.6852254797785,2.70962741922244,14.2015789338064));
#40454=CARTESIAN_POINT('Ctrl Pts',(18.5768226767695,3.62608620812782,14.0076819635675));
#40455=CARTESIAN_POINT('Ctrl Pts',(19.5464729449597,4.0512053341543,13.8818273075212));
#40456=CARTESIAN_POINT('Ctrl Pts',(20.7463406818482,4.47793026920173,13.7535017581769));
#40457=CARTESIAN_POINT('Ctrl Pts',(21.2156214332097,4.63869318435446,13.7015810566902));
#40458=CARTESIAN_POINT('Ctrl Pts',(22.1537708528639,4.93390876526191,13.5988388255709));
#40459=CARTESIAN_POINT('Ctrl Pts',(22.8728508922898,5.127670732978,13.5262523639447));
#40460=CARTESIAN_POINT('Ctrl Pts',(23.4112391022538,5.25280074041755,13.48036797944));
#40461=CARTESIAN_POINT('Ctrl Pts',(23.5274006995055,5.27931561824267,13.4704404449522));
#40462=CARTESIAN_POINT('Ctrl Pts',(23.7586975975701,5.3306297071107,13.4509289072634));
#40463=CARTESIAN_POINT('Ctrl Pts',(24.1668938536999,5.41708560365398,13.417181092299));
#40464=CARTESIAN_POINT('Ctrl Pts',(24.7548128660958,5.52956305821884,13.3713845002052));
#40465=CARTESIAN_POINT('Ctrl Pts',(25.3473131502197,5.62567073595883,13.3310219589392));
#40466=CARTESIAN_POINT('Ctrl Pts',(25.8218041556281,5.69154378511353,13.3034028562425));
#40467=CARTESIAN_POINT('Ctrl Pts',(26.0589587666352,5.72065900880548,13.2913640661324));
#40468=CARTESIAN_POINT('Ctrl Pts',(26.6316948383761,5.78623492045643,13.2646759506016));
#40469=CARTESIAN_POINT('Ctrl Pts',(27.5576851463966,5.85186367837989,13.236440987388));
#40470=CARTESIAN_POINT('Ctrl Pts',(28.5507795710394,5.88219883517421,13.2219159498841));
#40471=CARTESIAN_POINT('Ctrl Pts',(29.1361849357887,5.90128718803103,13.2135466774645));
#40472=CARTESIAN_POINT('Ctrl Pts',(29.2912521292177,5.90574282943922,13.211632738116));
#40473=CARTESIAN_POINT('Ctrl Pts',(29.6100275770339,5.91253309751288,13.2086893874642));
#40474=CARTESIAN_POINT('Ctrl Pts',(30.1692894984413,5.91881362945886,13.2059721234291));
#40475=CARTESIAN_POINT('Ctrl Pts',(31.3098805820073,5.91428725204102,13.2079309635128));
#40476=CARTESIAN_POINT('Ctrl Pts',(32.3163182251692,5.89785677449483,13.215170536538));
#40477=CARTESIAN_POINT('Ctrl Pts',(33.1686695899412,5.89783797451692,13.215185743277));
#40478=CARTESIAN_POINT('Ctrl Pts',(33.4952713010558,5.89783593918779,13.2151875891279));
#40479=CARTESIAN_POINT('Ctrl Pts',(34.1548283685118,5.8978321735044,13.2151907586342));
#40480=CARTESIAN_POINT('Ctrl Pts',(34.9764778638342,5.89782019909884,13.2152010495212));
#40481=CARTESIAN_POINT('Ctrl Pts',(35.9641101124161,5.89781516246843,13.2152053506642));
#40482=CARTESIAN_POINT('Ctrl Pts',(37.9386244259607,5.89780833274506,13.2152112104218));
#40483=CARTESIAN_POINT('Ctrl Pts',(39.5833333333333,5.89777260594516,13.2152418049849));
#40484=CARTESIAN_POINT('Ctrl Pts',(40.9,5.89777260594516,13.2152418049849));
#40485=CARTESIAN_POINT('Ctrl Pts',(6.84649785567288,-6.71741536412573,21.377211306072));
#40486=CARTESIAN_POINT('Ctrl Pts',(7.61279643984166,-5.59224351411651,21.7222003209083));
#40487=CARTESIAN_POINT('Ctrl Pts',(8.41290239278216,-4.4778139915129,21.9819683115275));
#40488=CARTESIAN_POINT('Ctrl Pts',(10.1883118359637,-2.12504829883048,22.351694214315));
#40489=CARTESIAN_POINT('Ctrl Pts',(11.1645908932198,-0.860235293933499,
22.4195115822635));
#40490=CARTESIAN_POINT('Ctrl Pts',(13.104616539894,1.36442582505286,22.4060524143024));
#40491=CARTESIAN_POINT('Ctrl Pts',(14.0814329274866,2.43568052201622,22.2982732069865));
#40492=CARTESIAN_POINT('Ctrl Pts',(15.9946796213894,4.24582169215595,22.0394507048973));
#40493=CARTESIAN_POINT('Ctrl Pts',(16.9653275559585,5.10151618176833,21.8412782041901));
#40494=CARTESIAN_POINT('Ctrl Pts',(18.8448710605557,6.49486940232068,21.4842569534398));
#40495=CARTESIAN_POINT('Ctrl Pts',(19.810123630216,7.14150804350578,21.2634255374822));
#40496=CARTESIAN_POINT('Ctrl Pts',(20.9856903475788,7.78021164720303,21.0426589820636));
#40497=CARTESIAN_POINT('Ctrl Pts',(21.450037782948,8.0234729107848,20.9532273635236));
#40498=CARTESIAN_POINT('Ctrl Pts',(22.3710393802638,8.46623345546782,20.7788884454097));
#40499=CARTESIAN_POINT('Ctrl Pts',(23.0719693188992,8.75491470148122,20.6575298272077));
#40500=CARTESIAN_POINT('Ctrl Pts',(23.5926347936587,8.94023465873174,20.5813719818061));
#40501=CARTESIAN_POINT('Ctrl Pts',(23.7065892332644,8.98001571960572,20.5647099449239));
#40502=CARTESIAN_POINT('Ctrl Pts',(23.9323706520528,9.05664995495951,20.5321468576875));
#40503=CARTESIAN_POINT('Ctrl Pts',(24.3307466212144,9.18574049076631,20.4759485784751));
#40504=CARTESIAN_POINT('Ctrl Pts',(24.9023508233185,9.35309964749801,20.4001844372317));
#40505=CARTESIAN_POINT('Ctrl Pts',(25.4757972573111,9.49555868076778,20.3338472412532));
#40506=CARTESIAN_POINT('Ctrl Pts',(25.9330914993694,9.5928869770777,20.28864648982));
#40507=CARTESIAN_POINT('Ctrl Pts',(26.1609781823312,9.63581705245677,20.2689918009898));
#40508=CARTESIAN_POINT('Ctrl Pts',(26.709932241435,9.73235004955936,20.2254900271808));
#40509=CARTESIAN_POINT('Ctrl Pts',(27.5959509089719,9.82915847887794,20.1795241403997));
#40510=CARTESIAN_POINT('Ctrl Pts',(28.579749560637,9.87532060641944,20.155272253243));
#40511=CARTESIAN_POINT('Ctrl Pts',(29.1657855350677,9.90441669946594,20.1412111689925));
#40512=CARTESIAN_POINT('Ctrl Pts',(29.3146731630637,9.9109781197532,20.1381027603739));
#40513=CARTESIAN_POINT('Ctrl Pts',(29.6257300067643,9.92113271524803,20.1332492263269));
#40514=CARTESIAN_POINT('Ctrl Pts',(30.1719452394076,9.93050366138696,20.1287785103479));
#40515=CARTESIAN_POINT('Ctrl Pts',(31.2977811219682,9.923768747263,20.1319916124711));
#40516=CARTESIAN_POINT('Ctrl Pts',(32.3069259117671,9.8985708956696,20.1442225454147));
#40517=CARTESIAN_POINT('Ctrl Pts',(33.1709940314752,9.89851679451553,20.1442592438603));
#40518=CARTESIAN_POINT('Ctrl Pts',(33.4961680489761,9.89851046735387,20.1442637388652));
#40519=CARTESIAN_POINT('Ctrl Pts',(34.1564024558335,9.89849933968833,20.1442714128625));
#40520=CARTESIAN_POINT('Ctrl Pts',(34.9773378017947,9.8984634550922,20.1442963704308));
#40521=CARTESIAN_POINT('Ctrl Pts',(35.9650395265661,9.89844842592581,20.1443067963913));
#40522=CARTESIAN_POINT('Ctrl Pts',(37.9392783163648,9.8984279817608,20.1443210056784));
#40523=CARTESIAN_POINT('Ctrl Pts',(39.5833333333333,9.89832117405885,20.1443951831047));
#40524=CARTESIAN_POINT('Ctrl Pts',(40.9,9.89832117405885,20.1443951831047));
#40525=CARTESIAN_POINT('Ctrl Pts',(6.90857970435318,-8.71018585725741,29.1272609852091));
#40526=CARTESIAN_POINT('Ctrl Pts',(7.67983757144493,-7.1626049441802,29.5775536996439));
#40527=CARTESIAN_POINT('Ctrl Pts',(8.48457055999567,-5.63283520142949,29.9097225030882));
#40528=CARTESIAN_POINT('Ctrl Pts',(10.2689932185249,-2.41146069737718,30.3644487697131));
#40529=CARTESIAN_POINT('Ctrl Pts',(11.2491988139072,-0.683672158318406,
30.4296414097155));
#40530=CARTESIAN_POINT('Ctrl Pts',(13.2074449203971,2.36894751212038,30.3576235761245));
#40531=CARTESIAN_POINT('Ctrl Pts',(14.1878085217557,3.82665309566742,30.184965998838));
#40532=CARTESIAN_POINT('Ctrl Pts',(16.1228140255812,6.30658851121944,29.7814752498472));
#40533=CARTESIAN_POINT('Ctrl Pts',(17.0983171044692,7.46839135174002,29.4886591763939));
#40534=CARTESIAN_POINT('Ctrl Pts',(18.9977376700381,9.36704911481261,28.960082872958));
#40535=CARTESIAN_POINT('Ctrl Pts',(19.9674462816337,10.2409515663328,28.6415548808294));
#40536=CARTESIAN_POINT('Ctrl Pts',(21.147106003231,11.1004135437216,28.3239820751166));
#40537=CARTESIAN_POINT('Ctrl Pts',(21.6116736136675,11.4272945418467,28.1962714220824));
#40538=CARTESIAN_POINT('Ctrl Pts',(22.5321107331755,12.0202838349911,27.948540960796));
#40539=CARTESIAN_POINT('Ctrl Pts',(23.2282372947769,12.4035528917693,27.7781185470828));
#40540=CARTESIAN_POINT('Ctrl Pts',(23.7411423015336,12.6473785079706,27.6723004799184));
#40541=CARTESIAN_POINT('Ctrl Pts',(23.8541050059083,12.7001926206312,27.6489722597557));
#40542=CARTESIAN_POINT('Ctrl Pts',(24.0772792343329,12.8015323632731,27.6035767537811));
#40543=CARTESIAN_POINT('Ctrl Pts',(24.4706231308706,12.9720321690745,27.5254067801747));
#40544=CARTESIAN_POINT('Ctrl Pts',(25.0326506601034,13.1919318242548,27.4207276483819));
#40545=CARTESIAN_POINT('Ctrl Pts',(25.5929166162092,13.3777331675808,27.3299203180183));
#40546=CARTESIAN_POINT('Ctrl Pts',(26.036986986334,13.5038445845534,27.2685418388));
#40547=CARTESIAN_POINT('Ctrl Pts',(26.257289284528,13.5592118403736,27.2420133361897));
#40548=CARTESIAN_POINT('Ctrl Pts',(26.7861809172635,13.6833062419416,27.1835476308027));
#40549=CARTESIAN_POINT('Ctrl Pts',(27.6340630276978,13.8074117592232,27.1220525704358));
#40550=CARTESIAN_POINT('Ctrl Pts',(28.6084466264574,13.8693290201703,27.0881176443602));
#40551=CARTESIAN_POINT('Ctrl Pts',(29.1951297895239,13.908430904103,27.0683644245336));
#40552=CARTESIAN_POINT('Ctrl Pts',(29.3379067795074,13.9168171018367,27.0642236253566));
#40553=CARTESIAN_POINT('Ctrl Pts',(29.6412852452592,13.9300946799831,27.0575993546201));
#40554=CARTESIAN_POINT('Ctrl Pts',(30.1744790744103,13.9423073235084,27.0515191755617));
#40555=CARTESIAN_POINT('Ctrl Pts',(31.285567721335,13.933569334585,27.0558675796336));
#40556=CARTESIAN_POINT('Ctrl Pts',(32.2974599236722,13.8994232817537,27.0731946134563));
#40557=CARTESIAN_POINT('Ctrl Pts',(33.1732579076352,13.8993047075201,27.0732696672437));
#40558=CARTESIAN_POINT('Ctrl Pts',(33.4970065888605,13.8992904506871,27.0732789151668));
#40559=CARTESIAN_POINT('Ctrl Pts',(34.1579215418456,13.8992658208367,27.0732946436726));
#40560=CARTESIAN_POINT('Ctrl Pts',(34.9781539333149,13.8991859907804,27.0733458523267));
#40561=CARTESIAN_POINT('Ctrl Pts',(35.9659297143336,13.8991526077107,27.0733672375489));
#40562=CARTESIAN_POINT('Ctrl Pts',(37.9398993196362,13.8991071452309,27.0733963900547));
#40563=CARTESIAN_POINT('Ctrl Pts',(39.5833333333333,13.8988697421725,27.0735485612246));
#40564=CARTESIAN_POINT('Ctrl Pts',(40.9,13.8988697421725,27.0735485612246));
#40565=CARTESIAN_POINT('Ctrl Pts',(6.93528330520032,-9.8656348186849,33.5512413216408));
#40566=CARTESIAN_POINT('Ctrl Pts',(7.70864561497005,-8.0776580699914,34.0623374960229));
#40567=CARTESIAN_POINT('Ctrl Pts',(8.5154187135237,-6.31093086144102,34.4367698578614));
#40568=CARTESIAN_POINT('Ctrl Pts',(10.3035747340622,-2.59403255178489,34.941954951338));
#40569=CARTESIAN_POINT('Ctrl Pts',(11.2855474597114,-0.60186360733143,35.0067705115655));
#40570=CARTESIAN_POINT('Ctrl Pts',(13.2510271399958,2.92382891559037,34.9032893217431));
#40571=CARTESIAN_POINT('Ctrl Pts',(14.2329608248363,4.60257161238984,34.6945593989859));
#40572=CARTESIAN_POINT('Ctrl Pts',(16.1768697182175,7.46747574760142,34.2095752766377));
#40573=CARTESIAN_POINT('Ctrl Pts',(17.1545233971705,8.80499374792143,33.8632511750181));
#40574=CARTESIAN_POINT('Ctrl Pts',(19.0635787323925,10.9976618314205,33.2359528227277));
#40575=CARTESIAN_POINT('Ctrl Pts',(20.0357940514507,12.0029926013879,32.8613840028835));
#40576=CARTESIAN_POINT('Ctrl Pts',(21.2200273744511,12.9932317593816,32.4867165469277));
#40577=CARTESIAN_POINT('Ctrl Pts',(21.6852779128345,13.3687144259959,32.3368305207218));
#40578=CARTESIAN_POINT('Ctrl Pts',(22.6074094382988,14.0501505350056,32.0460468583652));
#40579=CARTESIAN_POINT('Ctrl Pts',(23.303404556016,14.4891819334101,31.8467199720656));
#40580=CARTESIAN_POINT('Ctrl Pts',(23.8143672767891,14.7674149360666,31.7234333079367));
#40581=CARTESIAN_POINT('Ctrl Pts',(23.9270724954075,14.8277950271988,31.6962311639846));
#40582=CARTESIAN_POINT('Ctrl Pts',(24.1495225469485,14.9435144746797,31.6433583861176));
#40583=CARTESIAN_POINT('Ctrl Pts',(24.5413305977737,15.1380475804188,31.5524212197088));
#40584=CARTESIAN_POINT('Ctrl Pts',(25.09998893572,15.3882930140603,31.4310156375918));
#40585=CARTESIAN_POINT('Ctrl Pts',(25.6548568854792,15.5988027583032,31.3262265443364));
#40586=CARTESIAN_POINT('Ctrl Pts',(26.0929602492094,15.741087693316,31.2557376661541));
#40587=CARTESIAN_POINT('Ctrl Pts',(26.3096479269533,15.8033473177939,31.2253935968531));
#40588=CARTESIAN_POINT('Ctrl Pts',(26.8287121638341,15.9425694431084,31.1587088311854));
#40589=CARTESIAN_POINT('Ctrl Pts',(27.6557884297532,16.0810926132799,31.0890012981156));
#40590=CARTESIAN_POINT('Ctrl Pts',(28.624709126668,16.1519656805034,31.0495586097517));
#40591=CARTESIAN_POINT('Ctrl Pts',(29.2117706203409,16.1967753671696,31.0265558099781));
#40592=CARTESIAN_POINT('Ctrl Pts',(29.351092195488,16.206115111319,31.021876437373));
#40593=CARTESIAN_POINT('Ctrl Pts',(29.6501043905815,16.2210980111665,31.014285796168));
#40594=CARTESIAN_POINT('Ctrl Pts',(30.175870201979,16.2348498398373,31.0073340046886));
#40595=CARTESIAN_POINT('Ctrl Pts',(31.278535210342,16.2250286703999,31.0122942956317));
#40596=CARTESIAN_POINT('Ctrl Pts',(32.2920164760146,16.1856975481828,31.0325718136053));
#40597=CARTESIAN_POINT('Ctrl Pts',(33.1745232741631,16.1855272745483,31.0326760798738));
#40598=CARTESIAN_POINT('Ctrl Pts',(33.4974585875216,16.1855064782319,31.0326890056743));
#40599=CARTESIAN_POINT('Ctrl Pts',(34.1587639155491,16.1854709093049,31.0327109045834));
#40600=CARTESIAN_POINT('Ctrl Pts',(34.9785998474407,16.1853552918985,31.0327822824583));
#40601=CARTESIAN_POINT('Ctrl Pts',(35.9664200829455,16.1853069853609,31.0328120805002));
#40602=CARTESIAN_POINT('Ctrl Pts',(37.9402388284556,16.185241157271,31.0328527115372));
#40603=CARTESIAN_POINT('Ctrl Pts',(39.5833333333333,16.1848974953804,31.033064777293));
#40604=CARTESIAN_POINT('Ctrl Pts',(40.9,16.1848974953804,31.033064777293));
#40605=CARTESIAN_POINT('Origin',(6.9,25.9807621135332,15.));
#40606=CARTESIAN_POINT('',(6.9,6.90555748864272,29.194404870986));
#40607=CARTESIAN_POINT('Ctrl Pts',(6.9,1.9262302757419,10.8594625780008));
#40608=CARTESIAN_POINT('Ctrl Pts',(6.9,3.00887228147899,14.5482083700348));
#40609=CARTESIAN_POINT('Ctrl Pts',(6.90000000166257,4.07058553003038,18.4565659967827));
#40610=CARTESIAN_POINT('Ctrl Pts',(6.90000000166257,5.57797815223758,24.1072623232988));
#40611=CARTESIAN_POINT('Ctrl Pts',(6.9,6.24902093139924,26.6663167664834));
#40612=CARTESIAN_POINT('Ctrl Pts',(6.9,6.90555748864272,29.194404870986));
#40613=CARTESIAN_POINT('Origin',(6.9,0.,0.));
#40614=CARTESIAN_POINT('Origin',(40.9,7.79422863405995,4.5));
#40615=CARTESIAN_POINT('Ctrl Pts',(40.9,29.0996231131986,18.5327260452907));
#40616=CARTESIAN_POINT('Ctrl Pts',(40.9,28.6661818974695,18.2824786427117));
#40617=CARTESIAN_POINT('Ctrl Pts',(40.9,28.2327406817405,18.0322312401326));
#40618=CARTESIAN_POINT('Ctrl Pts',(40.9,27.7992994660114,17.7819838375536));
#40619=CARTESIAN_POINT('Ctrl Pts',(30.5,31.061268433756,16.1306417505986));
#40620=CARTESIAN_POINT('Ctrl Pts',(30.5,30.7013555966443,16.823692245373));
#40621=CARTESIAN_POINT('Ctrl Pts',(30.5,30.3108891324554,17.5));
#40622=CARTESIAN_POINT('Ctrl Pts',(30.5,12.8108891324554,47.8108891324553));
#40623=CARTESIAN_POINT('Ctrl Pts',(30.5,-17.5,30.3108891324554));
#40624=CARTESIAN_POINT('Ctrl Pts',(30.5,-47.8108891324553,12.8108891324554));
#40625=CARTESIAN_POINT('Ctrl Pts',(30.5,-30.3108891324554,-17.5));
#40626=CARTESIAN_POINT('Ctrl Pts',(30.5,-12.8108891324554,-47.8108891324553));
#40627=CARTESIAN_POINT('Ctrl Pts',(30.5,17.5,-30.3108891324554));
#40628=CARTESIAN_POINT('Ctrl Pts',(30.5,46.4877949884694,-13.5747778926489));
#40629=CARTESIAN_POINT('Ctrl Pts',(30.5,31.061268433756,16.1306417505986));
#40630=CARTESIAN_POINT('Ctrl Pts',(30.3311478274255,30.9943174850025,16.0958729911865));
#40631=CARTESIAN_POINT('Ctrl Pts',(30.3311478274255,30.6351804212937,16.7874296516619));
#40632=CARTESIAN_POINT('Ctrl Pts',(30.3311478274255,30.245555587262,17.4622796600955));
#40633=CARTESIAN_POINT('Ctrl Pts',(30.3311478274255,12.7832759271665,47.7078352473574));
#40634=CARTESIAN_POINT('Ctrl Pts',(30.3311478274255,-17.4622796600955,30.245555587262));
#40635=CARTESIAN_POINT('Ctrl Pts',(30.3311478274255,-47.7078352473574,12.7832759271665));
#40636=CARTESIAN_POINT('Ctrl Pts',(30.3311478274255,-30.245555587262,-17.4622796600955));
#40637=CARTESIAN_POINT('Ctrl Pts',(30.3311478274255,-12.7832759271665,-47.7078352473574));
#40638=CARTESIAN_POINT('Ctrl Pts',(30.3311478274255,17.4622796600955,-30.245555587262));
#40639=CARTESIAN_POINT('Ctrl Pts',(30.3311478274255,46.3875929639907,-13.5455181648638));
#40640=CARTESIAN_POINT('Ctrl Pts',(30.3311478274255,30.9943174850025,16.0958729911865));
#40641=CARTESIAN_POINT('Ctrl Pts',(29.9897712690917,30.8587004444282,16.0254447695752));
#40642=CARTESIAN_POINT('Ctrl Pts',(29.9897712690917,30.501134801215,16.7139754925468));
#40643=CARTESIAN_POINT('Ctrl Pts',(29.9897712690917,30.1132147882992,17.3858726641896));
#40644=CARTESIAN_POINT('Ctrl Pts',(29.9897712690917,12.7273421241097,47.4990874524888));
#40645=CARTESIAN_POINT('Ctrl Pts',(29.9897712690917,-17.3858726641896,30.1132147882992));
#40646=CARTESIAN_POINT('Ctrl Pts',(29.9897712690917,-47.4990874524888,12.7273421241097));
#40647=CARTESIAN_POINT('Ctrl Pts',(29.9897712690917,-30.1132147882992,-17.3858726641896));
#40648=CARTESIAN_POINT('Ctrl Pts',(29.9897712690917,-12.7273421241097,-47.4990874524888));
#40649=CARTESIAN_POINT('Ctrl Pts',(29.9897712690917,17.3858726641896,-30.1132147882992));
#40650=CARTESIAN_POINT('Ctrl Pts',(29.9897712690917,46.1846219490559,-13.4862491363571));
#40651=CARTESIAN_POINT('Ctrl Pts',(29.9897712690917,30.8587004444282,16.0254447695752));
#40652=CARTESIAN_POINT('Ctrl Pts',(29.4666899049319,30.6501289206644,15.9171300516369));
#40653=CARTESIAN_POINT('Ctrl Pts',(29.4666899049319,30.2949800354474,16.6010070497276));
#40654=CARTESIAN_POINT('Ctrl Pts',(29.4666899049319,29.9096819433198,17.2683629213518));
#40655=CARTESIAN_POINT('Ctrl Pts',(29.4666899049319,12.641319021968,47.1780448646716));
#40656=CARTESIAN_POINT('Ctrl Pts',(29.4666899049319,-17.2683629213518,29.9096819433198));
#40657=CARTESIAN_POINT('Ctrl Pts',(29.4666899049319,-47.1780448646716,12.641319021968));
#40658=CARTESIAN_POINT('Ctrl Pts',(29.4666899049319,-29.9096819433198,-17.2683629213518));
#40659=CARTESIAN_POINT('Ctrl Pts',(29.4666899049319,-12.641319021968,-47.1780448646716));
#40660=CARTESIAN_POINT('Ctrl Pts',(29.4666899049319,17.2683629213518,-29.9096819433198));
#40661=CARTESIAN_POINT('Ctrl Pts',(29.4666899049319,45.8724637299593,-13.3950966415431));
#40662=CARTESIAN_POINT('Ctrl Pts',(29.4666899049319,30.6501289206644,15.9171300516369));
#40663=CARTESIAN_POINT('Ctrl Pts',(28.7471241621752,30.3617042288049,15.7673462336858));
#40664=CARTESIAN_POINT('Ctrl Pts',(28.7471241621752,30.0098973754615,16.4447877935127));
#40665=CARTESIAN_POINT('Ctrl Pts',(28.7471241621752,29.6282250261092,17.105863694435));
#40666=CARTESIAN_POINT('Ctrl Pts',(28.7471241621752,12.5223613316743,46.7340887205442));
#40667=CARTESIAN_POINT('Ctrl Pts',(28.7471241621752,-17.105863694435,29.6282250261092));
#40668=CARTESIAN_POINT('Ctrl Pts',(28.7471241621752,-46.7340887205442,12.5223613316743));
#40669=CARTESIAN_POINT('Ctrl Pts',(28.7471241621752,-29.6282250261092,-17.105863694435));
#40670=CARTESIAN_POINT('Ctrl Pts',(28.7471241621752,-12.5223613316743,-46.7340887205442));
#40671=CARTESIAN_POINT('Ctrl Pts',(28.7471241621752,17.105863694435,-29.6282250261092));
#40672=CARTESIAN_POINT('Ctrl Pts',(28.7471241621752,45.4407934015768,-13.2690457322218));
#40673=CARTESIAN_POINT('Ctrl Pts',(28.7471241621752,30.3617042288049,15.7673462336858));
#40674=CARTESIAN_POINT('Ctrl Pts',(27.8100958442934,29.9846639164451,15.5715428260696));
#40675=CARTESIAN_POINT('Ctrl Pts',(27.8100958442934,29.6372259010587,16.2405717231752));
#40676=CARTESIAN_POINT('Ctrl Pts',(27.8100958442934,29.2602932679205,16.8934381948013));
#40677=CARTESIAN_POINT('Ctrl Pts',(27.8100958442934,12.3668550731192,46.1537314627218));
#40678=CARTESIAN_POINT('Ctrl Pts',(27.8100958442934,-16.8934381948013,29.2602932679205));
#40679=CARTESIAN_POINT('Ctrl Pts',(27.8100958442934,-46.1537314627218,12.3668550731192));
#40680=CARTESIAN_POINT('Ctrl Pts',(27.8100958442934,-29.2602932679205,-16.8934381948013));
#40681=CARTESIAN_POINT('Ctrl Pts',(27.8100958442934,-12.3668550731192,-46.1537314627218));
#40682=CARTESIAN_POINT('Ctrl Pts',(27.8100958442934,16.8934381948013,-29.2602932679205));
#40683=CARTESIAN_POINT('Ctrl Pts',(27.8100958442934,44.8764966543029,-13.1042669335782));
#40684=CARTESIAN_POINT('Ctrl Pts',(27.8100958442934,29.9846639164451,15.5715428260696));
#40685=CARTESIAN_POINT('Ctrl Pts',(26.8343111708818,29.5937642144445,15.3685420031368));
#40686=CARTESIAN_POINT('Ctrl Pts',(26.8343111708818,29.2508556284042,16.0288490017));
#40687=CARTESIAN_POINT('Ctrl Pts',(26.8343111708818,28.8788369357517,16.6732042787395));
#40688=CARTESIAN_POINT('Ctrl Pts',(26.8343111708818,12.2056326570121,45.5520412144912));
#40689=CARTESIAN_POINT('Ctrl Pts',(26.8343111708818,-16.6732042787395,28.8788369357517));
#40690=CARTESIAN_POINT('Ctrl Pts',(26.8343111708818,-45.5520412144912,12.2056326570121));
#40691=CARTESIAN_POINT('Ctrl Pts',(26.8343111708818,-28.8788369357517,-16.6732042787395));
#40692=CARTESIAN_POINT('Ctrl Pts',(26.8343111708818,-12.2056326570121,-45.5520412144912));
#40693=CARTESIAN_POINT('Ctrl Pts',(26.8343111708818,16.6732042787395,-28.8788369357517));
#40694=CARTESIAN_POINT('Ctrl Pts',(26.8343111708818,44.2914572749094,-12.9334311338658));
#40695=CARTESIAN_POINT('Ctrl Pts',(26.8343111708818,29.5937642144445,15.3685420031368));
#40696=CARTESIAN_POINT('Ctrl Pts',(25.8181479469611,29.1945242233064,15.1612099270726));
#40697=CARTESIAN_POINT('Ctrl Pts',(25.8181479469611,28.8562417071321,15.8126089354813));
#40698=CARTESIAN_POINT('Ctrl Pts',(25.8181479469611,28.4892417994669,16.4482714219305));
#40699=CARTESIAN_POINT('Ctrl Pts',(25.8181479469611,12.0409703775363,44.9375132213974));
#40700=CARTESIAN_POINT('Ctrl Pts',(25.8181479469611,-16.4482714219305,28.4892417994669));
#40701=CARTESIAN_POINT('Ctrl Pts',(25.8181479469611,-44.9375132213974,12.0409703775363));
#40702=CARTESIAN_POINT('Ctrl Pts',(25.8181479469611,-28.4892417994669,-16.4482714219305));
#40703=CARTESIAN_POINT('Ctrl Pts',(25.8181479469611,-12.0409703775363,-44.9375132213974));
#40704=CARTESIAN_POINT('Ctrl Pts',(25.8181479469611,16.4482714219305,-28.4892417994669));
#40705=CARTESIAN_POINT('Ctrl Pts',(25.8181479469611,43.6939354158518,-12.7589503583263));
#40706=CARTESIAN_POINT('Ctrl Pts',(25.8181479469611,29.1945242233064,15.1612099270726));
#40707=CARTESIAN_POINT('Ctrl Pts',(24.7595197917227,28.796912394945,14.9547233834603));
#40708=CARTESIAN_POINT('Ctrl Pts',(24.7595197917227,28.4632370828042,15.5972507298839));
#40709=CARTESIAN_POINT('Ctrl Pts',(24.7595197917227,28.1012354927406,16.2242558762949));
#40710=CARTESIAN_POINT('Ctrl Pts',(24.7595197917227,11.8769796164458,44.3254913690355));
#40711=CARTESIAN_POINT('Ctrl Pts',(24.7595197917227,-16.2242558762949,28.1012354927406));
#40712=CARTESIAN_POINT('Ctrl Pts',(24.7595197917227,-44.3254913690355,11.8769796164458));
#40713=CARTESIAN_POINT('Ctrl Pts',(24.7595197917227,-28.1012354927406,-16.2242558762949));
#40714=CARTESIAN_POINT('Ctrl Pts',(24.7595197917227,-11.8769796164458,-44.3254913690355));
#40715=CARTESIAN_POINT('Ctrl Pts',(24.7595197917227,16.2242558762949,-28.1012354927406));
#40716=CARTESIAN_POINT('Ctrl Pts',(24.7595197917227,43.0988503438666,-12.5851811425261));
#40717=CARTESIAN_POINT('Ctrl Pts',(24.7595197917227,28.796912394945,14.9547233834603));
#40718=CARTESIAN_POINT('Ctrl Pts',(23.6563574780851,28.4140727469455,14.7559082828157));
#40719=CARTESIAN_POINT('Ctrl Pts',(23.6563574780851,28.084833470769,15.389893569599));
#40720=CARTESIAN_POINT('Ctrl Pts',(23.6563574780851,27.7276444994825,16.0085630157705));
#40721=CARTESIAN_POINT('Ctrl Pts',(23.6563574780851,11.719081483712,43.736207515253));
#40722=CARTESIAN_POINT('Ctrl Pts',(23.6563574780851,-16.0085630157705,27.7276444994825));
#40723=CARTESIAN_POINT('Ctrl Pts',(23.6563574780851,-43.736207515253,11.719081483712));
#40724=CARTESIAN_POINT('Ctrl Pts',(23.6563574780851,-27.7276444994825,-16.0085630157705));
#40725=CARTESIAN_POINT('Ctrl Pts',(23.6563574780851,-11.719081483712,-43.736207515253));
#40726=CARTESIAN_POINT('Ctrl Pts',(23.6563574780851,16.0085630157705,-27.7276444994825));
#40727=CARTESIAN_POINT('Ctrl Pts',(23.6563574780851,42.5258740306932,-12.4178678468319));
#40728=CARTESIAN_POINT('Ctrl Pts',(23.6563574780851,28.4140727469455,14.7559082828157));
#40729=CARTESIAN_POINT('Ctrl Pts',(22.5073180101405,28.0598057001003,14.5719314169357));
#40730=CARTESIAN_POINT('Ctrl Pts',(22.5073180101405,27.7346713837132,15.1980121665098));
#40731=CARTESIAN_POINT('Ctrl Pts',(22.5073180101405,27.3819358493961,15.8089680335819));
#40732=CARTESIAN_POINT('Ctrl Pts',(22.5073180101405,11.5729678158142,43.190903882978));
#40733=CARTESIAN_POINT('Ctrl Pts',(22.5073180101405,-15.8089680335819,27.3819358493961));
#40734=CARTESIAN_POINT('Ctrl Pts',(22.5073180101405,-43.190903882978,11.5729678158142));
#40735=CARTESIAN_POINT('Ctrl Pts',(22.5073180101405,-27.3819358493961,-15.8089680335819));
#40736=CARTESIAN_POINT('Ctrl Pts',(22.5073180101405,-11.5729678158142,-43.190903882978));
#40737=CARTESIAN_POINT('Ctrl Pts',(22.5073180101405,15.8089680335819,-27.3819358493961));
#40738=CARTESIAN_POINT('Ctrl Pts',(22.5073180101405,41.9956608528241,-12.2630417010206));
#40739=CARTESIAN_POINT('Ctrl Pts',(22.5073180101405,28.0598057001003,14.5719314169357));
#40740=CARTESIAN_POINT('Ctrl Pts',(21.3125219557939,27.7463544749225,14.4091508971893));
#40741=CARTESIAN_POINT('Ctrl Pts',(21.3125219557939,27.4248521776202,15.0282378072439));
#40742=CARTESIAN_POINT('Ctrl Pts',(21.3125219557939,27.0760569908086,15.632368792237));
#40743=CARTESIAN_POINT('Ctrl Pts',(21.3125219557939,11.4436881985716,42.7084257830456));
#40744=CARTESIAN_POINT('Ctrl Pts',(21.3125219557939,-15.632368792237,27.0760569908086));
#40745=CARTESIAN_POINT('Ctrl Pts',(21.3125219557939,-42.7084257830456,11.4436881985716));
#40746=CARTESIAN_POINT('Ctrl Pts',(21.3125219557939,-27.0760569908086,-15.632368792237));
#40747=CARTESIAN_POINT('Ctrl Pts',(21.3125219557939,-11.4436881985716,-42.7084257830456));
#40748=CARTESIAN_POINT('Ctrl Pts',(21.3125219557939,15.632368792237,-27.0760569908086));
#40749=CARTESIAN_POINT('Ctrl Pts',(21.3125219557939,41.5265346055806,-12.1260533880339));
#40750=CARTESIAN_POINT('Ctrl Pts',(21.3125219557939,27.7463544749225,14.4091508971893));
#40751=CARTESIAN_POINT('Ctrl Pts',(20.0742472323676,27.4822408172221,14.2719922102254));
#40752=CARTESIAN_POINT('Ctrl Pts',(20.0742472323676,27.1637988552073,14.8851861187906));
#40753=CARTESIAN_POINT('Ctrl Pts',(20.0742472323676,26.8183238008716,15.4835664656477));
#40754=CARTESIAN_POINT('Ctrl Pts',(20.0742472323676,11.3347573352238,42.3018902665193));
#40755=CARTESIAN_POINT('Ctrl Pts',(20.0742472323676,-15.4835664656477,26.8183238008716));
#40756=CARTESIAN_POINT('Ctrl Pts',(20.0742472323676,-42.3018902665193,11.3347573352238));
#40757=CARTESIAN_POINT('Ctrl Pts',(20.0742472323676,-26.8183238008716,-15.4835664656477));
#40758=CARTESIAN_POINT('Ctrl Pts',(20.0742472323676,-11.3347573352238,-42.3018902665193));
#40759=CARTESIAN_POINT('Ctrl Pts',(20.0742472323676,15.4835664656477,-26.8183238008716));
#40760=CARTESIAN_POINT('Ctrl Pts',(20.0742472323676,41.1312493454498,-12.0106271861277));
#40761=CARTESIAN_POINT('Ctrl Pts',(20.0742472323676,27.4822408172221,14.2719922102254));
#40762=CARTESIAN_POINT('Ctrl Pts',(18.7979917002302,27.2694232481814,14.1614724492006));
#40763=CARTESIAN_POINT('Ctrl Pts',(18.7979917002302,26.9534472438987,14.7699178935542));
#40764=CARTESIAN_POINT('Ctrl Pts',(18.7979917002302,26.6106474867381,15.3636644897785));
#40765=CARTESIAN_POINT('Ctrl Pts',(18.7979917002302,11.2469829969596,41.9743119765166));
#40766=CARTESIAN_POINT('Ctrl Pts',(18.7979917002302,-15.3636644897785,26.6106474867381));
#40767=CARTESIAN_POINT('Ctrl Pts',(18.7979917002302,-41.9743119765166,11.2469829969596));
#40768=CARTESIAN_POINT('Ctrl Pts',(18.7979917002302,-26.6106474867381,-15.3636644897785));
#40769=CARTESIAN_POINT('Ctrl Pts',(18.7979917002302,-11.2469829969596,-41.9743119765166));
#40770=CARTESIAN_POINT('Ctrl Pts',(18.7979917002302,15.3636644897785,-26.6106474867381));
#40771=CARTESIAN_POINT('Ctrl Pts',(18.7979917002302,40.8127362898543,-11.9176190323383));
#40772=CARTESIAN_POINT('Ctrl Pts',(18.7979917002302,27.2694232481814,14.1614724492006));
#40773=CARTESIAN_POINT('Ctrl Pts',(17.4917404060759,27.1042817018803,14.0757116526895));
#40774=CARTESIAN_POINT('Ctrl Pts',(17.4917404060759,26.7902192241678,14.6804723978617));
#40775=CARTESIAN_POINT('Ctrl Pts',(17.4917404060759,26.4494954361781,15.2706233100072));
#40776=CARTESIAN_POINT('Ctrl Pts',(17.4917404060759,11.1788721261709,41.7201187461852));
#40777=CARTESIAN_POINT('Ctrl Pts',(17.4917404060759,-15.2706233100072,26.4494954361781));
#40778=CARTESIAN_POINT('Ctrl Pts',(17.4917404060759,-41.7201187461852,11.1788721261709));
#40779=CARTESIAN_POINT('Ctrl Pts',(17.4917404060759,-26.4494954361781,-15.2706233100072));
#40780=CARTESIAN_POINT('Ctrl Pts',(17.4917404060759,-11.1788721261709,-41.7201187461852));
#40781=CARTESIAN_POINT('Ctrl Pts',(17.4917404060759,15.2706233100072,-26.4494954361781));
#40782=CARTESIAN_POINT('Ctrl Pts',(17.4917404060759,40.5655774732432,-11.8454468408945));
#40783=CARTESIAN_POINT('Ctrl Pts',(17.4917404060759,27.1042817018803,14.0757116526895));
#40784=CARTESIAN_POINT('Ctrl Pts',(16.1647270995715,26.9797204766935,14.011024902894));
#40785=CARTESIAN_POINT('Ctrl Pts',(16.1647270995715,26.6671013136366,14.6130063919992));
#40786=CARTESIAN_POINT('Ctrl Pts',(16.1647270995715,26.3279433657953,15.2004451894511));
#40787=CARTESIAN_POINT('Ctrl Pts',(16.1647270995715,11.1274981763442,41.5283885552464));
#40788=CARTESIAN_POINT('Ctrl Pts',(16.1647270995715,-15.2004451894511,26.3279433657953));
#40789=CARTESIAN_POINT('Ctrl Pts',(16.1647270995715,-41.5283885552464,11.1274981763442));
#40790=CARTESIAN_POINT('Ctrl Pts',(16.1647270995715,-26.3279433657953,-15.2004451894511));
#40791=CARTESIAN_POINT('Ctrl Pts',(16.1647270995715,-11.1274981763442,-41.5283885552464));
#40792=CARTESIAN_POINT('Ctrl Pts',(16.1647270995715,15.2004451894511,-26.3279433657953));
#40793=CARTESIAN_POINT('Ctrl Pts',(16.1647270995715,40.3791531257526,-11.7910095609247));
#40794=CARTESIAN_POINT('Ctrl Pts',(16.1647270995715,26.9797204766935,14.011024902894));
#40795=CARTESIAN_POINT('Ctrl Pts',(14.8263876417415,26.8868282012067,13.9627843740029));
#40796=CARTESIAN_POINT('Ctrl Pts',(14.8263876417415,26.5752853986496,14.5626932163446));
#40797=CARTESIAN_POINT('Ctrl Pts',(14.8263876417415,26.2372951854241,15.1481094381123));
#40798=CARTESIAN_POINT('Ctrl Pts',(14.8263876417415,11.0891857473118,41.3854046235364));
#40799=CARTESIAN_POINT('Ctrl Pts',(14.8263876417415,-15.1481094381123,26.2372951854241));
#40800=CARTESIAN_POINT('Ctrl Pts',(14.8263876417415,-41.3854046235364,11.0891857473118));
#40801=CARTESIAN_POINT('Ctrl Pts',(14.8263876417415,-26.2372951854241,-15.1481094381123));
#40802=CARTESIAN_POINT('Ctrl Pts',(14.8263876417415,-11.0891857473118,-41.3854046235364));
#40803=CARTESIAN_POINT('Ctrl Pts',(14.8263876417415,15.1481094381123,-26.2372951854241));
#40804=CARTESIAN_POINT('Ctrl Pts',(14.8263876417415,40.2401260583921,-11.750412635195));
#40805=CARTESIAN_POINT('Ctrl Pts',(14.8263876417415,26.8868282012067,13.9627843740029));
#40806=CARTESIAN_POINT('Ctrl Pts',(13.4853470903953,26.8165326442879,13.926278703034));
#40807=CARTESIAN_POINT('Ctrl Pts',(13.4853470903953,26.505804369746,14.5246190849439));
#40808=CARTESIAN_POINT('Ctrl Pts',(13.4853470903953,26.1686978312363,15.1085047372063));
#40809=CARTESIAN_POINT('Ctrl Pts',(13.4853470903953,11.0601930940301,41.2772025684426));
#40810=CARTESIAN_POINT('Ctrl Pts',(13.4853470903953,-15.1085047372063,26.1686978312363));
#40811=CARTESIAN_POINT('Ctrl Pts',(13.4853470903953,-41.2772025684426,11.0601930940301));
#40812=CARTESIAN_POINT('Ctrl Pts',(13.4853470903953,-26.1686978312363,-15.1085047372063));
#40813=CARTESIAN_POINT('Ctrl Pts',(13.4853470903953,-11.0601930940301,-41.2772025684426));
#40814=CARTESIAN_POINT('Ctrl Pts',(13.4853470903953,15.1085047372063,-26.1686978312363));
#40815=CARTESIAN_POINT('Ctrl Pts',(13.4853470903953,40.1349183317465,-11.7196912055776));
#40816=CARTESIAN_POINT('Ctrl Pts',(13.4853470903953,26.8165326442879,13.926278703034));
#40817=CARTESIAN_POINT('Ctrl Pts',(12.1482076787549,26.7614591013549,13.8976780812377));
#40818=CARTESIAN_POINT('Ctrl Pts',(12.1482076787549,26.4513689744511,14.4947896419145));
#40819=CARTESIAN_POINT('Ctrl Pts',(12.1482076787549,26.1149547570431,15.0774761588537));
#40820=CARTESIAN_POINT('Ctrl Pts',(12.1482076787549,11.0374785981894,41.1924309158968));
#40821=CARTESIAN_POINT('Ctrl Pts',(12.1482076787549,-15.0774761588537,26.1149547570431));
#40822=CARTESIAN_POINT('Ctrl Pts',(12.1482076787549,-41.1924309158968,11.0374785981894));
#40823=CARTESIAN_POINT('Ctrl Pts',(12.1482076787549,-26.1149547570431,-15.0774761588537));
#40824=CARTESIAN_POINT('Ctrl Pts',(12.1482076787549,-11.0374785981894,-41.1924309158968));
#40825=CARTESIAN_POINT('Ctrl Pts',(12.1482076787549,15.0774761588537,-26.1149547570431));
#40826=CARTESIAN_POINT('Ctrl Pts',(12.1482076787549,40.0524926066472,-11.6956222878942));
#40827=CARTESIAN_POINT('Ctrl Pts',(12.1482076787549,26.7614591013549,13.8976780812377));
#40828=CARTESIAN_POINT('Ctrl Pts',(10.8190675759626,26.716817747915,13.8744950717886));
#40829=CARTESIAN_POINT('Ctrl Pts',(10.8190675759626,26.4072448888814,14.4706105780977));
#40830=CARTESIAN_POINT('Ctrl Pts',(10.8190675759626,26.0713918511132,15.0523251033884));
#40831=CARTESIAN_POINT('Ctrl Pts',(10.8190675759626,11.0190667477248,41.1237169545017));
#40832=CARTESIAN_POINT('Ctrl Pts',(10.8190675759626,-15.0523251033884,26.0713918511132));
#40833=CARTESIAN_POINT('Ctrl Pts',(10.8190675759626,-41.1237169545017,11.0190667477248));
#40834=CARTESIAN_POINT('Ctrl Pts',(10.8190675759626,-26.0713918511132,-15.0523251033884));
#40835=CARTESIAN_POINT('Ctrl Pts',(10.8190675759626,-11.0190667477248,-41.1237169545017));
#40836=CARTESIAN_POINT('Ctrl Pts',(10.8190675759626,15.0523251033884,-26.0713918511132));
#40837=CARTESIAN_POINT('Ctrl Pts',(10.8190675759626,39.9856802003493,-11.6761125740823));
#40838=CARTESIAN_POINT('Ctrl Pts',(10.8190675759626,26.716817747915,13.8744950717886));
#40839=CARTESIAN_POINT('Ctrl Pts',(9.50027713254189,26.6796403391198,13.8551882149624));
#40840=CARTESIAN_POINT('Ctrl Pts',(9.50027713254189,26.3704982618073,14.4504742051937));
#40841=CARTESIAN_POINT('Ctrl Pts',(9.50027713254189,26.0351125755702,15.0313792538877));
#40842=CARTESIAN_POINT('Ctrl Pts',(9.50027713254189,11.0037333216825,41.0664918294579));
#40843=CARTESIAN_POINT('Ctrl Pts',(9.50027713254189,-15.0313792538877,26.0351125755702));
#40844=CARTESIAN_POINT('Ctrl Pts',(9.5002771325419,-41.0664918294579,11.0037333216825));
#40845=CARTESIAN_POINT('Ctrl Pts',(9.5002771325419,-26.0351125755702,-15.0313792538877));
#40846=CARTESIAN_POINT('Ctrl Pts',(9.5002771325419,-11.0037333216825,-41.0664918294579));
#40847=CARTESIAN_POINT('Ctrl Pts',(9.50027713254189,15.0313792538877,-26.0351125755702));
#40848=CARTESIAN_POINT('Ctrl Pts',(9.50027713254189,39.9300386942093,-11.6598648452397));
#40849=CARTESIAN_POINT('Ctrl Pts',(9.50027713254189,26.6796403391198,13.8551882149624));
#40850=CARTESIAN_POINT('Ctrl Pts',(8.45435372222587,26.6546635289318,13.8422173352292));
#40851=CARTESIAN_POINT('Ctrl Pts',(8.45435372222587,26.3458108626791,14.4369460336456));
#40852=CARTESIAN_POINT('Ctrl Pts',(8.45435372222587,26.0107391561104,15.0173072536015));
#40853=CARTESIAN_POINT('Ctrl Pts',(8.45435372222587,10.9934319025089,41.0280464097118));
#40854=CARTESIAN_POINT('Ctrl Pts',(8.45435372222587,-15.0173072536015,26.0107391561104));
#40855=CARTESIAN_POINT('Ctrl Pts',(8.45435372222587,-41.0280464097118,10.9934319025089));
#40856=CARTESIAN_POINT('Ctrl Pts',(8.45435372222587,-26.0107391561104,-15.0173072536015));
#40857=CARTESIAN_POINT('Ctrl Pts',(8.45435372222587,-10.9934319025089,-41.0280464097118));
#40858=CARTESIAN_POINT('Ctrl Pts',(8.45435372222587,15.0173072536015,-26.0107391561104));
#40859=CARTESIAN_POINT('Ctrl Pts',(8.45435372222587,39.8926571933874,-11.6489491721888));
#40860=CARTESIAN_POINT('Ctrl Pts',(8.45435372222587,26.6546635289318,13.8422173352292));
#40861=CARTESIAN_POINT('Ctrl Pts',(7.67514864245731,26.6383620035993,13.8337516775666));
#40862=CARTESIAN_POINT('Ctrl Pts',(7.67514864245731,26.3296982262274,14.4281166503283));
#40863=CARTESIAN_POINT('Ctrl Pts',(7.67514864245731,25.9948314436454,15.0081229315276));
#40864=CARTESIAN_POINT('Ctrl Pts',(7.67514864245731,10.9867085121178,41.0029543751729));
#40865=CARTESIAN_POINT('Ctrl Pts',(7.67514864245731,-15.0081229315276,25.9948314436454));
#40866=CARTESIAN_POINT('Ctrl Pts',(7.67514864245731,-41.0029543751729,10.9867085121178));
#40867=CARTESIAN_POINT('Ctrl Pts',(7.67514864245731,-25.9948314436454,-15.0081229315276));
#40868=CARTESIAN_POINT('Ctrl Pts',(7.67514864245731,-10.9867085121178,-41.0029543751729));
#40869=CARTESIAN_POINT('Ctrl Pts',(7.67514864245731,15.0081229315276,-25.9948314436454));
#40870=CARTESIAN_POINT('Ctrl Pts',(7.67514864245731,39.8682595430058,-11.6418248789176));
#40871=CARTESIAN_POINT('Ctrl Pts',(7.67514864245731,26.6383620035993,13.8337516775666));
#40872=CARTESIAN_POINT('Ctrl Pts',(7.15799654185577,26.6285708447822,13.8286669632852));
#40873=CARTESIAN_POINT('Ctrl Pts',(7.15799654185577,26.3200205194336,14.4228134720947));
#40874=CARTESIAN_POINT('Ctrl Pts',(7.15799654185577,25.9852768200144,15.0026065670023));
#40875=CARTESIAN_POINT('Ctrl Pts',(7.15799654185577,10.9826702530122,40.9878833870167));
#40876=CARTESIAN_POINT('Ctrl Pts',(7.15799654185577,-15.0026065670023,25.9852768200144));
#40877=CARTESIAN_POINT('Ctrl Pts',(7.15799654185577,-40.9878833870167,10.9826702530122));
#40878=CARTESIAN_POINT('Ctrl Pts',(7.15799654185577,-25.9852768200144,-15.0026065670023));
#40879=CARTESIAN_POINT('Ctrl Pts',(7.15799654185577,-10.9826702530122,-40.9878833870167));
#40880=CARTESIAN_POINT('Ctrl Pts',(7.15799654185577,15.0026065670023,-25.9852768200144));
#40881=CARTESIAN_POINT('Ctrl Pts',(7.15799654185577,39.8536056216838,-11.6375458261629));
#40882=CARTESIAN_POINT('Ctrl Pts',(7.15799654185577,26.6285708447822,13.8286669632852));
#40883=CARTESIAN_POINT('Ctrl Pts',(6.9,26.6239443717909,13.8262643576559));
#40884=CARTESIAN_POINT('Ctrl Pts',(6.9,26.3154476542665,14.4203076388911));
#40885=CARTESIAN_POINT('Ctrl Pts',(6.9,25.9807621135332,15.));
#40886=CARTESIAN_POINT('Ctrl Pts',(6.9,10.9807621135332,40.9807621135332));
#40887=CARTESIAN_POINT('Ctrl Pts',(6.9,-15.,25.9807621135332));
#40888=CARTESIAN_POINT('Ctrl Pts',(6.9,-40.9807621135332,10.9807621135332));
#40889=CARTESIAN_POINT('Ctrl Pts',(6.9,-25.9807621135332,-15.));
#40890=CARTESIAN_POINT('Ctrl Pts',(6.9,-10.9807621135332,-40.9807621135332));
#40891=CARTESIAN_POINT('Ctrl Pts',(6.9,15.,-25.9807621135332));
#40892=CARTESIAN_POINT('Ctrl Pts',(6.9,39.846681418688,-11.6355239079847));
#40893=CARTESIAN_POINT('Ctrl Pts',(6.9,26.6239443717909,13.8262643576559));
#40894=CARTESIAN_POINT('Ctrl Pts',(6.9,6.90555748864272,29.194404870986));
#40895=CARTESIAN_POINT('Ctrl Pts',(7.85773098116326,8.83308608050287,28.7583591297181));
#40896=CARTESIAN_POINT('Ctrl Pts',(8.88781981167334,10.6725495024415,28.148927360677));
#40897=CARTESIAN_POINT('Ctrl Pts',(10.5914578196776,13.4378975079049,26.9549567714738));
#40898=CARTESIAN_POINT('Ctrl Pts',(11.2365058953701,14.4268759573926,26.4627511078989));
#40899=CARTESIAN_POINT('Ctrl Pts',(12.0558885382926,15.5639851987506,25.8276163596339));
#40900=CARTESIAN_POINT('Ctrl Pts',(12.1875764958397,15.7427052651201,25.7255677072203));
#40901=CARTESIAN_POINT('Ctrl Pts',(13.194901830313,17.0880993664927,24.9407551262718));
#40902=CARTESIAN_POINT('Ctrl Pts',(14.2258982134098,18.4224696507577,24.0748117650462));
#40903=CARTESIAN_POINT('Ctrl Pts',(18.2616480823244,22.4465505568645,20.9914735836847));
#40904=CARTESIAN_POINT('Ctrl Pts',(21.0496416709525,24.4970863377161,19.1084188222497));
#40905=CARTESIAN_POINT('Ctrl Pts',(25.8000196361138,27.440416330328,18.0798601480504));
#40906=CARTESIAN_POINT('Ctrl Pts',(26.8976561124457,27.9949084025612,18.1725012311874));
#40907=CARTESIAN_POINT('Ctrl Pts',(28.0045908801237,28.5110480063609,18.293020318403));
#40908=CARTESIAN_POINT('Ctrl Pts',(28.5235971652406,28.7375730360626,18.3760345677216));
#40909=CARTESIAN_POINT('Ctrl Pts',(29.0834839543824,28.9821227669884,18.4629109750536));
#40910=CARTESIAN_POINT('Ctrl Pts',(29.1146288039499,28.995750541561,18.4676985487665));
#40911=CARTESIAN_POINT('Ctrl Pts',(29.5949306848436,29.2050975774362,18.5426905181125));
#40912=CARTESIAN_POINT('Ctrl Pts',(30.0492939924726,29.3870260594868,18.6372599535756));
#40913=CARTESIAN_POINT('Ctrl Pts',(30.5,29.559989655385,18.7405179110273));
#40914=CARTESIAN_POINT('Ctrl Pts',(6.45331003273164,1.59669678622779,10.9133179225515));
#40915=CARTESIAN_POINT('Ctrl Pts',(7.20830533428676,2.1627262104287,10.8283039351861));
#40916=CARTESIAN_POINT('Ctrl Pts',(7.9992896214032,2.70879554626307,10.7080816105349));
#40917=CARTESIAN_POINT('Ctrl Pts',(9.76164489174098,3.82718122480732,10.3736775708918));
#40918=CARTESIAN_POINT('Ctrl Pts',(10.7316587814816,4.40082635509404,10.1362456656108));
#40919=CARTESIAN_POINT('Ctrl Pts',(12.6606926111663,5.38563263712134,9.65961205419967));
#40920=CARTESIAN_POINT('Ctrl Pts',(13.6374431259541,5.83915384029437,9.38360450626091));
#40921=CARTESIAN_POINT('Ctrl Pts',(14.8679539417017,6.32358226998234,9.06165302613707));
#40922=CARTESIAN_POINT('Ctrl Pts',(15.8146186835335,6.68453209751777,8.8086769516328));
#40923=CARTESIAN_POINT('Ctrl Pts',(16.7768279789012,7.0051694125711,8.55011854625631));
#40924=CARTESIAN_POINT('Ctrl Pts',(18.4426549461009,7.48808598435166,8.14533972931254));
#40925=CARTESIAN_POINT('Ctrl Pts',(19.4151948753427,7.72973898022671,7.90738588441824));
#40926=CARTESIAN_POINT('Ctrl Pts',(20.6328868119184,7.97443640583059,7.66437297695771));
#40927=CARTESIAN_POINT('Ctrl Pts',(21.1054260060187,8.06465516157005,7.57098863237663));
#40928=CARTESIAN_POINT('Ctrl Pts',(22.0544239964407,8.2283193842107,7.3938759247957));
#40929=CARTESIAN_POINT('Ctrl Pts',(22.7836594350112,8.33397294082319,7.27389266543021));
#40930=CARTESIAN_POINT('Ctrl Pts',(23.5025637456204,8.42426711082601,7.17270583388455));
#40931=CARTESIAN_POINT('Ctrl Pts',(23.9756232708729,8.4795264691222,7.10861034193437));
#40932=CARTESIAN_POINT('Ctrl Pts',(24.5702383273712,8.53935462310087,7.03666681503306));
#40933=CARTESIAN_POINT('Ctrl Pts',(25.0506812637281,8.58189400875846,6.98463603831062));
#40934=CARTESIAN_POINT('Ctrl Pts',(25.4117237717367,8.61093616318062,6.94891133994702));
#40935=CARTESIAN_POINT('Ctrl Pts',(25.713233130151,8.63276690479095,6.92207219011214));
#40936=CARTESIAN_POINT('Ctrl Pts',(25.924350018954,8.64675417662542,6.90499555217216));
#40937=CARTESIAN_POINT('Ctrl Pts',(26.0449825351307,8.65437719289231,6.89574165973189));
#40938=CARTESIAN_POINT('Ctrl Pts',(26.1053107047432,8.65806460962808,6.89128602190966));
#40939=CARTESIAN_POINT('Ctrl Pts',(26.5982868813559,8.68771831234638,6.85557010312596));
#40940=CARTESIAN_POINT('Ctrl Pts',(27.5414448539116,8.7222238682218,6.81230249083085));
#40941=CARTESIAN_POINT('Ctrl Pts',(28.5384718269746,8.73742874004845,6.79157348079204));
#40942=CARTESIAN_POINT('Ctrl Pts',(29.123571801101,8.74727658763319,6.77903979219489));
#40943=CARTESIAN_POINT('Ctrl Pts',(29.2812925824008,8.74962231400052,6.77610142826287));
#40944=CARTESIAN_POINT('Ctrl Pts',(29.6033746665997,8.75316560056402,6.77163194910164));
#40945=CARTESIAN_POINT('Ctrl Pts',(30.1682156581426,8.75644680260445,6.76749797708623));
#40946=CARTESIAN_POINT('Ctrl Pts',(31.31511200853,8.75407681716339,6.7704817474239));
#40947=CARTESIAN_POINT('Ctrl Pts',(32.3203490755539,8.74562733267077,6.78127046660755));
#40948=CARTESIAN_POINT('Ctrl Pts',(33.1676615322707,8.74562186943987,6.78128357449778));
#40949=CARTESIAN_POINT('Ctrl Pts',(33.4948723279894,8.74562133595168,6.78128505761794));
#40950=CARTESIAN_POINT('Ctrl Pts',(34.1541357431676,8.74562028433967,6.7812877053352));
#40951=CARTESIAN_POINT('Ctrl Pts',(34.9760826079903,8.74561702798978,6.78129612595839));
#40952=CARTESIAN_POINT('Ctrl Pts',(35.9636845487691,8.74561567977429,6.78129958330352));
#40953=CARTESIAN_POINT('Ctrl Pts',(37.9383132355672,8.74561382885199,6.78130435924949));
#40954=CARTESIAN_POINT('Ctrl Pts',(39.5833333333333,8.74560464293355,6.7813280023926));
#40955=CARTESIAN_POINT('Ctrl Pts',(40.9,8.74560464293355,6.7813280023926));
#40956=CARTESIAN_POINT('Ctrl Pts',(6.63336813585096,2.58998912169033,14.1980521881427));
#40957=CARTESIAN_POINT('Ctrl Pts',(7.389696336477,3.32655463912721,14.0595388287459));
#40958=CARTESIAN_POINT('Ctrl Pts',(8.18035160561763,4.03465273479121,13.8764440634215));
#40959=CARTESIAN_POINT('Ctrl Pts',(9.9416314386187,5.47986851886093,13.3869575789582));
#40960=CARTESIAN_POINT('Ctrl Pts',(10.9109664605568,6.21859686207518,13.0495988183286));
#40961=CARTESIAN_POINT('Ctrl Pts',(12.8334013836927,7.47915893423736,12.3824387994051));
#40962=CARTESIAN_POINT('Ctrl Pts',(13.8089179831182,8.05904353786121,12.0008911509523));
#40963=CARTESIAN_POINT('Ctrl Pts',(15.0306778911272,8.67329495695321,11.5604290689694));
#40964=CARTESIAN_POINT('Ctrl Pts',(15.9745670647921,9.13243737556314,11.2141745075895));
#40965=CARTESIAN_POINT('Ctrl Pts',(16.9295440841729,9.53704617981304,10.8635736365946));
#40966=CARTESIAN_POINT('Ctrl Pts',(18.5792362231986,10.1451076803253,10.3171018918725));
#40967=CARTESIAN_POINT('Ctrl Pts',(19.5469773926756,10.4493242965117,9.99640408637918));
#40968=CARTESIAN_POINT('Ctrl Pts',(20.7474295734276,10.754900018616,9.67172058444861));
#40969=CARTESIAN_POINT('Ctrl Pts',(21.2167794172893,10.8681544802446,9.54637190554475));
#40970=CARTESIAN_POINT('Ctrl Pts',(22.1549843938463,11.0724642143302,9.30976886072816));
#40971=CARTESIAN_POINT('Ctrl Pts',(22.8744776078266,11.2039970972494,9.14996578827686));
#40972=CARTESIAN_POINT('Ctrl Pts',(23.5816077902761,11.3162019466948,9.01558422395416));
#40973=CARTESIAN_POINT('Ctrl Pts',(24.0500749276264,11.3851612528794,8.93008359351429));
#40974=CARTESIAN_POINT('Ctrl Pts',(24.6365533946125,11.4594652258083,8.83449183240023));
#40975=CARTESIAN_POINT('Ctrl Pts',(25.1102835291687,11.512269915973,8.76539275960626));
#40976=CARTESIAN_POINT('Ctrl Pts',(25.4658322439329,11.5482688417072,8.71801358900137));
#40977=CARTESIAN_POINT('Ctrl Pts',(25.7624874136684,11.5753180370233,8.68244638509936));
#40978=CARTESIAN_POINT('Ctrl Pts',(25.9700349923411,11.5926401638759,8.65983585467431));
#40979=CARTESIAN_POINT('Ctrl Pts',(26.0885791323128,11.6020803597252,8.64758737376051));
#40980=CARTESIAN_POINT('Ctrl Pts',(26.1478525996403,11.606646750038,8.64169115913857));
#40981=CARTESIAN_POINT('Ctrl Pts',(26.6319130667262,11.6433645250355,8.59444428954213));
#40982=CARTESIAN_POINT('Ctrl Pts',(27.5577774489366,11.6860824768892,8.53717709311578));
#40983=CARTESIAN_POINT('Ctrl Pts',(28.5508423746856,11.7050908260001,8.5094282805872));
#40984=CARTESIAN_POINT('Ctrl Pts',(29.1362159539421,11.7174369518245,8.49263545125888));
#40985=CARTESIAN_POINT('Ctrl Pts',(29.291281950884,11.7203386713975,8.48875007883411));
#40986=CARTESIAN_POINT('Ctrl Pts',(29.6100529981868,11.724747509447,8.48280581727725));
#40987=CARTESIAN_POINT('Ctrl Pts',(30.1693026775045,11.7288279027909,8.4773119045209));
#40988=CARTESIAN_POINT('Ctrl Pts',(31.3098786008462,11.725887289448,8.48127083805327));
#40989=CARTESIAN_POINT('Ctrl Pts',(32.3162827048882,11.7152777874898,8.49575357359986));
#40990=CARTESIAN_POINT('Ctrl Pts',(33.1686195735696,11.7152690782769,8.495775239756));
#40991=CARTESIAN_POINT('Ctrl Pts',(33.4952188807557,11.7152682401723,8.49577770055111));
#40992=CARTESIAN_POINT('Ctrl Pts',(34.1547734244041,11.7152665713231,8.49578208271195));
#40993=CARTESIAN_POINT('Ctrl Pts',(34.9764178792931,11.7152614171757,8.49579602915744));
#40994=CARTESIAN_POINT('Ctrl Pts',(35.9640520550921,11.7152592814565,8.49580175406155));
#40995=CARTESIAN_POINT('Ctrl Pts',(37.9385651163987,11.7152563511876,8.49580966365999));
#40996=CARTESIAN_POINT('Ctrl Pts',(39.5833333333333,11.7152418049849,8.49584881729847));
#40997=CARTESIAN_POINT('Ctrl Pts',(40.9,11.7152418049849,8.49584881729847));
#40998=CARTESIAN_POINT('Ctrl Pts',(6.84648239176542,4.8711720049463,21.8719108775553));
#40999=CARTESIAN_POINT('Ctrl Pts',(7.61278097593421,6.01809391809558,21.6080942034255));
#41000=CARTESIAN_POINT('Ctrl Pts',(8.41274152921386,7.11297694015339,21.2759544371052));
#41001=CARTESIAN_POINT('Ctrl Pts',(10.1879716557546,9.3352659896486,20.4198986989574));
#41002=CARTESIAN_POINT('Ctrl Pts',(11.1642573475929,10.4645258845954,19.8462357742843));
#41003=CARTESIAN_POINT('Ctrl Pts',(13.1034321172788,12.3837514736036,18.7228640453274));
#41004=CARTESIAN_POINT('Ctrl Pts',(14.0822646095709,13.259092905625,18.0925354910949));
#41005=CARTESIAN_POINT('Ctrl Pts',(15.3084001581866,14.1807147676624,17.369341405527));
#41006=CARTESIAN_POINT('Ctrl Pts',(16.2531227144981,14.8695159890908,16.8032299545452));
#41007=CARTESIAN_POINT('Ctrl Pts',(17.2084375604977,15.4708786153412,16.2348330754283));
#41008=CARTESIAN_POINT('Ctrl Pts',(18.8473961588578,16.3684102669437,15.3570672461537));
#41009=CARTESIAN_POINT('Ctrl Pts',(19.8110405035781,16.8164458459157,14.8437940564496));
#41010=CARTESIAN_POINT('Ctrl Pts',(20.9872655006159,17.2594998647323,14.3329359049566));
#41011=CARTESIAN_POINT('Ctrl Pts',(21.4517346237734,17.4254488483261,14.1338378277511));
#41012=CARTESIAN_POINT('Ctrl Pts',(22.3727984841463,17.7217491293399,13.7614448137587));
#41013=CARTESIAN_POINT('Ctrl Pts',(23.0743543377559,17.9111527143534,13.5118529399621));
#41014=CARTESIAN_POINT('Ctrl Pts',(23.7582742987063,18.0719640430561,13.3034745440379));
#41015=CARTESIAN_POINT('Ctrl Pts',(24.2174386855893,18.1719103336476,13.1693266480666));
#41016=CARTESIAN_POINT('Ctrl Pts',(24.7870213943586,18.2785218143407,13.020703786838));
#41017=CARTESIAN_POINT('Ctrl Pts',(25.2463470121633,18.3542161979471,12.9133861579982));
#41018=CARTESIAN_POINT('Ctrl Pts',(25.5899787396418,18.4056632423986,12.8400372670538));
#41019=CARTESIAN_POINT('Ctrl Pts',(25.8759048428223,18.4442660174719,12.7850917865304));
#41020=CARTESIAN_POINT('Ctrl Pts',(26.0755068065028,18.468956785964,12.7502361709813));
#41021=CARTESIAN_POINT('Ctrl Pts',(26.1893780149128,18.4824083304411,12.7313725692327));
#41022=CARTESIAN_POINT('Ctrl Pts',(26.2462863876019,18.4889145361418,12.7222969574594));
#41023=CARTESIAN_POINT('Ctrl Pts',(26.7102722067271,18.5411896593428,12.6496548741737));
#41024=CARTESIAN_POINT('Ctrl Pts',(27.5960905386885,18.602045864812,12.5614420302555));
#41025=CARTESIAN_POINT('Ctrl Pts',(28.5798438027284,18.6298999603239,12.5173520665107));
#41026=CARTESIAN_POINT('Ctrl Pts',(29.1658297917575,18.6480680632813,12.4906249890438));
#41027=CARTESIAN_POINT('Ctrl Pts',(29.3147155528136,18.652196249303,12.4846522276655));
#41028=CARTESIAN_POINT('Ctrl Pts',(29.6257654938389,18.6585637397072,12.4753713397181));
#41029=CARTESIAN_POINT('Ctrl Pts',(30.1719616098275,18.6644443298452,12.4668129248998));
#41030=CARTESIAN_POINT('Ctrl Pts',(31.2977738410332,18.6602190141085,12.4729611884879));
#41031=CARTESIAN_POINT('Ctrl Pts',(32.3068669150107,18.6445149503825,12.4961463862896));
#41032=CARTESIAN_POINT('Ctrl Pts',(33.1709127040732,18.6444874715365,12.4962026881972));
#41033=CARTESIAN_POINT('Ctrl Pts',(33.4960830255433,18.644484418038,12.4962093123004));
#41034=CARTESIAN_POINT('Ctrl Pts',(34.1563135822161,18.6444789016083,12.4962208405723));
#41035=CARTESIAN_POINT('Ctrl Pts',(34.9772414248898,18.6444614154563,12.4962577684094));
#41036=CARTESIAN_POINT('Ctrl Pts',(35.9649463721129,18.6444542286038,12.496272896639));
#41037=CARTESIAN_POINT('Ctrl Pts',(37.9391834323222,18.6444443083029,12.4962938290756));
#41038=CARTESIAN_POINT('Ctrl Pts',(39.5833333333333,18.6443951831047,12.4963973854122));
#41039=CARTESIAN_POINT('Ctrl Pts',(40.9,18.6443951831047,12.4963973854122));
#41040=CARTESIAN_POINT('Ctrl Pts',(6.90857970435318,7.02038826853569,29.5800408844791));
#41041=CARTESIAN_POINT('Ctrl Pts',(7.67983757144493,8.58577901088988,29.1962153577801));
#41042=CARTESIAN_POINT('Ctrl Pts',(8.48446296596919,10.0765485557757,28.7191114013952));
#41043=CARTESIAN_POINT('Ctrl Pts',(10.2687526859613,13.0935628879537,27.5023711977385));
#41044=CARTESIAN_POINT('Ctrl Pts',(11.2489627292759,14.6224501564806,26.6949552438923));
#41045=CARTESIAN_POINT('Ctrl Pts',(13.2065810728343,17.2294066625499,25.1069038454383));
#41046=CARTESIAN_POINT('Ctrl Pts',(14.1884325798659,18.406995285395,24.2271697832518));
#41047=CARTESIAN_POINT('Ctrl Pts',(15.4296983589675,19.6550892131211,23.2080338536349));
#41048=CARTESIAN_POINT('Ctrl Pts',(16.3788042670986,20.5796860932724,22.4189011948389));
#41049=CARTESIAN_POINT('Ctrl Pts',(17.3450159165718,21.3903231452906,21.6217224592711));
#41050=CARTESIAN_POINT('Ctrl Pts',(18.9999962645462,22.5937460627634,20.3951481814249));
#41051=CARTESIAN_POINT('Ctrl Pts',(19.9686658165164,23.1898054127388,19.6835411202358));
#41052=CARTESIAN_POINT('Ctrl Pts',(21.148943716884,23.7756910485748,18.9783964629486));
#41053=CARTESIAN_POINT('Ctrl Pts',(21.6136662410167,23.9949385633152,18.7043064424585));
#41054=CARTESIAN_POINT('Ctrl Pts',(22.5341605437881,24.3846521737582,18.1932305660766));
#41055=CARTESIAN_POINT('Ctrl Pts',(23.2310352415762,24.6315178872709,17.8537326154787));
#41056=CARTESIAN_POINT('Ctrl Pts',(23.9047680627609,24.8394315921367,17.5731511638351));
#41057=CARTESIAN_POINT('Ctrl Pts',(24.3593217251592,24.96958718913,17.391254980069));
#41058=CARTESIAN_POINT('Ctrl Pts',(24.9191284505008,25.1069751863358,17.1917285847407));
#41059=CARTESIAN_POINT('Ctrl Pts',(25.3687829483026,25.2041659752934,17.0482631873592));
#41060=CARTESIAN_POINT('Ctrl Pts',(25.7038809466239,25.269917189492,16.9507036504243));
#41061=CARTESIAN_POINT('Ctrl Pts',(25.9815275275379,25.3190677310922,16.8779731233104));
#41062=CARTESIAN_POINT('Ctrl Pts',(26.1747255747307,25.3504124116977,16.832023377701));
#41063=CARTESIAN_POINT('Ctrl Pts',(26.284743001994,25.3674660195526,16.8072090098453));
#41064=CARTESIAN_POINT('Ctrl Pts',(26.3396756125252,25.3757090167853,16.7952849898384));
#41065=CARTESIAN_POINT('Ctrl Pts',(26.7867185605548,25.4418392909473,16.7000344271697));
#41066=CARTESIAN_POINT('Ctrl Pts',(27.6343089133549,25.5185659559041,16.5847364280862));
#41067=CARTESIAN_POINT('Ctrl Pts',(28.608620419133,25.5552242576153,16.5243820587323));
#41068=CARTESIAN_POINT('Ctrl Pts',(29.1952293795947,25.5792110357045,16.4877244301024));
#41069=CARTESIAN_POINT('Ctrl Pts',(29.3380035933317,25.5844033272728,16.4799452423708));
#41070=CARTESIAN_POINT('Ctrl Pts',(29.6413717635319,25.5925899885789,16.4675695714432));
#41071=CARTESIAN_POINT('Ctrl Pts',(30.1745368065168,25.6001268754993,16.4561967872261));
#41072=CARTESIAN_POINT('Ctrl Pts',(31.2855894033321,25.5947346655062,16.464330041984));
#41073=CARTESIAN_POINT('Ctrl Pts',(32.2974015084454,25.57383077045,16.4964013295029));
#41074=CARTESIAN_POINT('Ctrl Pts',(33.1731651112182,25.5737672879573,16.4965224425527));
#41075=CARTESIAN_POINT('Ctrl Pts',(33.4969081472871,25.57375987162,16.4965369996128));
#41076=CARTESIAN_POINT('Ctrl Pts',(34.1578169391039,25.5737469053194,16.4965619872358));
#41077=CARTESIAN_POINT('Ctrl Pts',(34.9780359591179,25.5737054251286,16.496642344611));
#41078=CARTESIAN_POINT('Ctrl Pts',(35.9658147840134,25.5736884251095,16.4966752246752));
#41079=CARTESIAN_POINT('Ctrl Pts',(37.9397802282711,25.5736649097448,16.4967207607426));
#41080=CARTESIAN_POINT('Ctrl Pts',(39.5833333333333,25.5735485612246,16.4969459535258));
#41081=CARTESIAN_POINT('Ctrl Pts',(40.9,25.5735485612246,16.4969459535258));
#41082=CARTESIAN_POINT('Ctrl Pts',(6.93528330520032,8.231730283379,33.9890447223856));
#41083=CARTESIAN_POINT('Ctrl Pts',(7.70864561497005,10.0357116563145,33.5376786188307));
#41084=CARTESIAN_POINT('Ctrl Pts',(8.51532719250786,11.7528338486872,32.9786927413523));
#41085=CARTESIAN_POINT('Ctrl Pts',(10.3033707684643,15.2242195800702,31.5578840442132));
#41086=CARTESIAN_POINT('Ctrl Pts',(11.285359425586,16.9818886494149,30.6179424293771));
#41087=CARTESIAN_POINT('Ctrl Pts',(13.2503075123955,19.9828238609275,28.7660858779662));
#41088=CARTESIAN_POINT('Ctrl Pts',(14.2335802328307,21.333808720003,27.7445903826109));
#41089=CARTESIAN_POINT('Ctrl Pts',(15.4809874764708,22.7701484639683,26.5562215055806));
#41090=CARTESIAN_POINT('Ctrl Pts',(16.4318967140332,23.8303538982284,25.6398645222147));
#41091=CARTESIAN_POINT('Ctrl Pts',(17.4027860882061,24.7620955812504,24.7114068344531));
#41092=CARTESIAN_POINT('Ctrl Pts',(19.0657008739463,26.1438767914272,23.2827894621994));
#41093=CARTESIAN_POINT('Ctrl Pts',(20.0370987955263,26.8257745442827,22.4568785783624));
#41094=CARTESIAN_POINT('Ctrl Pts',(21.2219373681819,27.4963832022122,21.636875295208));
#41095=CARTESIAN_POINT('Ctrl Pts',(21.6873545199147,27.7466423667126,21.3192655757679));
#41096=CARTESIAN_POINT('Ctrl Pts',(22.6095407883915,28.1914275999317,20.7266792263566));
#41097=CARTESIAN_POINT('Ctrl Pts',(23.306319546872,28.4721721598032,20.3342063552499));
#41098=CARTESIAN_POINT('Ctrl Pts',(23.97749158379,28.7077527668379,20.0111563083465));
#41099=CARTESIAN_POINT('Ctrl Pts',(24.4307021142574,28.8553793495036,19.8016082531841));
#41100=CARTESIAN_POINT('Ctrl Pts',(24.9871188326861,29.0105626137835,19.5726095610118));
#41101=CARTESIAN_POINT('Ctrl Pts',(25.4329141726813,29.1200357132463,19.4084486444522));
#41102=CARTESIAN_POINT('Ctrl Pts',(25.7643950554696,29.1939083663022,19.2971155191106));
#41103=CARTESIAN_POINT('Ctrl Pts',(26.0382972138574,29.2489718106937,19.2143910494173));
#41104=CARTESIAN_POINT('Ctrl Pts',(26.2284820979132,29.2840172105126,19.1622606931669));
#41105=CARTESIAN_POINT('Ctrl Pts',(26.336649445506,29.3030632173393,19.1341507449285));
#41106=CARTESIAN_POINT('Ctrl Pts',(26.3906225284363,29.3122642693063,19.1206543727096));
#41107=CARTESIAN_POINT('Ctrl Pts',(26.829365411603,29.3859982106888,19.012988583459));
#41108=CARTESIAN_POINT('Ctrl Pts',(27.6560988760142,29.4710985842864,18.8833816200192));
#41109=CARTESIAN_POINT('Ctrl Pts',(28.6249317030316,29.5127595133995,18.8137794716614));
#41110=CARTESIAN_POINT('Ctrl Pts',(29.2119052185271,29.5400636810175,18.7714558506413));
#41111=CARTESIAN_POINT('Ctrl Pts',(29.3512234939538,29.5458124634022,18.7627335234214));
#41112=CARTESIAN_POINT('Ctrl Pts',(29.6502234545149,29.5549926880431,18.7486685476098));
#41113=CARTESIAN_POINT('Ctrl Pts',(30.1759548990663,29.5634265890419,18.7357718416965));
#41114=CARTESIAN_POINT('Ctrl Pts',(31.2785766862299,29.5574021311856,18.744977162533));
#41115=CARTESIAN_POINT('Ctrl Pts',(32.2919610610308,29.5334837411523,18.7821959068193));
#41116=CARTESIAN_POINT('Ctrl Pts',(33.1744263360524,29.5333904072539,18.7823679845324));
#41117=CARTESIAN_POINT('Ctrl Pts',(33.4973548461807,29.5333792377698,18.7823889294252));
#41118=CARTESIAN_POINT('Ctrl Pts',(34.1586526208335,29.5333600113093,18.7824245927187));
#41119=CARTESIAN_POINT('Ctrl Pts',(34.9784715438079,29.533298230803,18.7825395490483));
#41120=CARTESIAN_POINT('Ctrl Pts',(35.9662945600334,29.5332729456427,18.782586552422));
#41121=CARTESIAN_POINT('Ctrl Pts',(37.9401075800398,29.5332379342859,18.7826516826343));
#41122=CARTESIAN_POINT('Ctrl Pts',(39.5833333333333,29.533064777293,18.7829737067337));
#41123=CARTESIAN_POINT('Ctrl Pts',(40.9,29.533064777293,18.7829737067337));
#41124=CARTESIAN_POINT('Origin',(6.9,30.,0.));
#41125=CARTESIAN_POINT('',(6.9,20.5775906479515,21.8303175223207));
#41126=CARTESIAN_POINT('Ctrl Pts',(6.9,7.09789564133157,8.44145532612415));
#41127=CARTESIAN_POINT('Ctrl Pts',(6.9,9.87986401752105,11.09468188726));
#41128=CARTESIAN_POINT('Ctrl Pts',(6.90000000166257,12.753513475675,13.9485622548227));
#41129=CARTESIAN_POINT('Ctrl Pts',(6.90000000166257,16.8843019432417,18.0885125115534));
#41130=CARTESIAN_POINT('Ctrl Pts',(6.9,18.7449692586141,19.9691972794379));
#41131=CARTESIAN_POINT('Ctrl Pts',(6.9,20.5775906479515,21.8303175223207));
#41132=CARTESIAN_POINT('Origin',(6.9,0.,0.));
#41133=CARTESIAN_POINT('Origin',(40.9,9.,0.));
#41134=CARTESIAN_POINT('Ctrl Pts',(40.9,34.4673758792282,1.5));
#41135=CARTESIAN_POINT('Ctrl Pts',(40.9,33.9668810740701,1.5));
#41136=CARTESIAN_POINT('Ctrl Pts',(40.9,33.466386268912,1.5));
#41137=CARTESIAN_POINT('Ctrl Pts',(40.9,32.9658914637539,1.5));
#41138=CARTESIAN_POINT('Ctrl Pts',(30.5,34.9651684126997,-1.56108868151375));
#41139=CARTESIAN_POINT('Ctrl Pts',(30.5,35.,-0.78093292837788));
#41140=CARTESIAN_POINT('Ctrl Pts',(30.5,35.,0.));
#41141=CARTESIAN_POINT('Ctrl Pts',(30.5,35.,35.));
#41142=CARTESIAN_POINT('Ctrl Pts',(30.5,0.,35.));
#41143=CARTESIAN_POINT('Ctrl Pts',(30.5,-35.,35.));
#41144=CARTESIAN_POINT('Ctrl Pts',(30.5,-35.,0.));
#41145=CARTESIAN_POINT('Ctrl Pts',(30.5,-35.,-35.));
#41146=CARTESIAN_POINT('Ctrl Pts',(30.5,0.,-35.));
#41147=CARTESIAN_POINT('Ctrl Pts',(30.5,33.472222479613,-35.));
#41148=CARTESIAN_POINT('Ctrl Pts',(30.5,34.9651684126997,-1.56108868151375));
#41149=CARTESIAN_POINT('Ctrl Pts',(30.3311478274255,34.8898028105656,-1.55772383604587));
#41150=CARTESIAN_POINT('Ctrl Pts',(30.3311478274255,34.924559320191,-0.779249668063534));
#41151=CARTESIAN_POINT('Ctrl Pts',(30.3311478274255,34.924559320191,0.));
#41152=CARTESIAN_POINT('Ctrl Pts',(30.3311478274255,34.924559320191,34.924559320191));
#41153=CARTESIAN_POINT('Ctrl Pts',(30.3311478274255,0.,34.924559320191));
#41154=CARTESIAN_POINT('Ctrl Pts',(30.3311478274255,-34.924559320191,34.924559320191));
#41155=CARTESIAN_POINT('Ctrl Pts',(30.3311478274255,-34.924559320191,0.));
#41156=CARTESIAN_POINT('Ctrl Pts',(30.3311478274255,-34.924559320191,-34.924559320191));
#41157=CARTESIAN_POINT('Ctrl Pts',(30.3311478274255,0.,-34.924559320191));
#41158=CARTESIAN_POINT('Ctrl Pts',(30.3311478274255,33.4000748447964,-34.924559320191));
#41159=CARTESIAN_POINT('Ctrl Pts',(30.3311478274255,34.8898028105656,-1.55772383604587));
#41160=CARTESIAN_POINT('Ctrl Pts',(29.9897712690917,34.7371408974366,-1.55090794481746));
#41161=CARTESIAN_POINT('Ctrl Pts',(29.9897712690917,34.7717453283792,-0.775840025831457));
#41162=CARTESIAN_POINT('Ctrl Pts',(29.9897712690917,34.7717453283792,0.));
#41163=CARTESIAN_POINT('Ctrl Pts',(29.9897712690917,34.7717453283791,34.7717453283791));
#41164=CARTESIAN_POINT('Ctrl Pts',(29.9897712690917,0.,34.7717453283792));
#41165=CARTESIAN_POINT('Ctrl Pts',(29.9897712690917,-34.7717453283791,34.7717453283791));
#41166=CARTESIAN_POINT('Ctrl Pts',(29.9897712690917,-34.7717453283792,0.));
#41167=CARTESIAN_POINT('Ctrl Pts',(29.9897712690917,-34.7717453283791,-34.7717453283791));
#41168=CARTESIAN_POINT('Ctrl Pts',(29.9897712690917,0.,-34.7717453283792));
#41169=CARTESIAN_POINT('Ctrl Pts',(29.9897712690917,33.2539313038843,-34.7717453283791));
#41170=CARTESIAN_POINT('Ctrl Pts',(29.9897712690917,34.7371408974366,-1.55090794481746));
#41171=CARTESIAN_POINT('Ctrl Pts',(29.4666899049319,34.5023553003819,-1.54042548027394));
#41172=CARTESIAN_POINT('Ctrl Pts',(29.4666899049319,34.5367258427036,-0.770596184255043));
#41173=CARTESIAN_POINT('Ctrl Pts',(29.4666899049319,34.5367258427036,0.));
#41174=CARTESIAN_POINT('Ctrl Pts',(29.4666899049319,34.5367258427036,34.5367258427036));
#41175=CARTESIAN_POINT('Ctrl Pts',(29.4666899049319,0.,34.5367258427036));
#41176=CARTESIAN_POINT('Ctrl Pts',(29.4666899049319,-34.5367258427036,34.5367258427036));
#41177=CARTESIAN_POINT('Ctrl Pts',(29.4666899049319,-34.5367258427036,0.));
#41178=CARTESIAN_POINT('Ctrl Pts',(29.4666899049319,-34.5367258427036,-34.5367258427036));
#41179=CARTESIAN_POINT('Ctrl Pts',(29.4666899049319,0.,-34.5367258427036));
#41180=CARTESIAN_POINT('Ctrl Pts',(29.4666899049319,33.0291706035535,-34.5367258427036));
#41181=CARTESIAN_POINT('Ctrl Pts',(29.4666899049319,34.5023553003819,-1.54042548027394));
#41182=CARTESIAN_POINT('Ctrl Pts',(28.7471241621752,34.1776802811774,-1.52592972576568));
#41183=CARTESIAN_POINT('Ctrl Pts',(28.7471241621752,34.21172738887,-0.763344698704455));
#41184=CARTESIAN_POINT('Ctrl Pts',(28.7471241621752,34.21172738887,0.));
#41185=CARTESIAN_POINT('Ctrl Pts',(28.7471241621752,34.2117273888699,34.2117273888699));
#41186=CARTESIAN_POINT('Ctrl Pts',(28.7471241621752,0.,34.21172738887));
#41187=CARTESIAN_POINT('Ctrl Pts',(28.7471241621752,-34.2117273888699,34.2117273888699));
#41188=CARTESIAN_POINT('Ctrl Pts',(28.7471241621752,-34.21172738887,0.));
#41189=CARTESIAN_POINT('Ctrl Pts',(28.7471241621752,-34.2117273888699,-34.2117273888699));
#41190=CARTESIAN_POINT('Ctrl Pts',(28.7471241621752,0.,-34.21172738887));
#41191=CARTESIAN_POINT('Ctrl Pts',(28.7471241621752,32.718358587775,-34.2117273888699));
#41192=CARTESIAN_POINT('Ctrl Pts',(28.7471241621752,34.1776802811774,-1.52592972576568));
#41193=CARTESIAN_POINT('Ctrl Pts',(27.8100958442934,33.7532520886149,-1.50698029472893));
#41194=CARTESIAN_POINT('Ctrl Pts',(27.8100958442934,33.7868763896026,-0.753865266276394));
#41195=CARTESIAN_POINT('Ctrl Pts',(27.8100958442934,33.7868763896026,0.));
#41196=CARTESIAN_POINT('Ctrl Pts',(27.8100958442934,33.7868763896026,33.7868763896026));
#41197=CARTESIAN_POINT('Ctrl Pts',(27.8100958442934,0.,33.7868763896026));
#41198=CARTESIAN_POINT('Ctrl Pts',(27.8100958442934,-33.7868763896026,33.7868763896026));
#41199=CARTESIAN_POINT('Ctrl Pts',(27.8100958442934,-33.7868763896026,0.));
#41200=CARTESIAN_POINT('Ctrl Pts',(27.8100958442934,-33.7868763896026,-33.7868763896026));
#41201=CARTESIAN_POINT('Ctrl Pts',(27.8100958442934,0.,-33.7868763896026));
#41202=CARTESIAN_POINT('Ctrl Pts',(27.8100958442934,32.3120526686846,-33.7868763896026));
#41203=CARTESIAN_POINT('Ctrl Pts',(27.8100958442934,33.7532520886149,-1.50698029472893));
#41204=CARTESIAN_POINT('Ctrl Pts',(26.8343111708818,33.3132226048841,-1.48733431337754));
#41205=CARTESIAN_POINT('Ctrl Pts',(26.8343111708818,33.3464085574791,-0.744037385305066));
#41206=CARTESIAN_POINT('Ctrl Pts',(26.8343111708818,33.3464085574791,0.));
#41207=CARTESIAN_POINT('Ctrl Pts',(26.8343111708818,33.3464085574791,33.3464085574791));
#41208=CARTESIAN_POINT('Ctrl Pts',(26.8343111708818,0.,33.3464085574791));
#41209=CARTESIAN_POINT('Ctrl Pts',(26.8343111708818,-33.3464085574791,33.3464085574791));
#41210=CARTESIAN_POINT('Ctrl Pts',(26.8343111708818,-33.3464085574791,0.));
#41211=CARTESIAN_POINT('Ctrl Pts',(26.8343111708818,-33.3464085574791,-33.3464085574791));
#41212=CARTESIAN_POINT('Ctrl Pts',(26.8343111708818,0.,-33.3464085574791));
#41213=CARTESIAN_POINT('Ctrl Pts',(26.8343111708818,31.8908116037717,-33.3464085574791));
#41214=CARTESIAN_POINT('Ctrl Pts',(26.8343111708818,33.3132226048841,-1.48733431337754));
#41215=CARTESIAN_POINT('Ctrl Pts',(25.8181479469611,32.8638045923198,-1.46726916269953));
#41216=CARTESIAN_POINT('Ctrl Pts',(25.8181479469611,32.8965428438611,-0.733999815330423));
#41217=CARTESIAN_POINT('Ctrl Pts',(25.8181479469611,32.8965428438611,0.));
#41218=CARTESIAN_POINT('Ctrl Pts',(25.8181479469611,32.896542843861,32.896542843861));
#41219=CARTESIAN_POINT('Ctrl Pts',(25.8181479469611,0.,32.8965428438611));
#41220=CARTESIAN_POINT('Ctrl Pts',(25.8181479469611,-32.896542843861,32.896542843861));
#41221=CARTESIAN_POINT('Ctrl Pts',(25.8181479469611,-32.8965428438611,0.));
#41222=CARTESIAN_POINT('Ctrl Pts',(25.8181479469611,-32.896542843861,-32.896542843861));
#41223=CARTESIAN_POINT('Ctrl Pts',(25.8181479469611,0.,-32.8965428438611));
#41224=CARTESIAN_POINT('Ctrl Pts',(25.8181479469611,31.4605828822811,-32.896542843861));
#41225=CARTESIAN_POINT('Ctrl Pts',(25.8181479469611,32.8638045923198,-1.46726916269953));
#41226=CARTESIAN_POINT('Ctrl Pts',(24.7595197917227,32.4162193763075,-1.44728584082667));
#41227=CARTESIAN_POINT('Ctrl Pts',(24.7595197917227,32.4485117525897,-0.724003180127255));
#41228=CARTESIAN_POINT('Ctrl Pts',(24.7595197917227,32.4485117525897,0.));
#41229=CARTESIAN_POINT('Ctrl Pts',(24.7595197917227,32.4485117525897,32.4485117525897));
#41230=CARTESIAN_POINT('Ctrl Pts',(24.7595197917227,0.,32.4485117525897));
#41231=CARTESIAN_POINT('Ctrl Pts',(24.7595197917227,-32.4485117525897,32.4485117525897));
#41232=CARTESIAN_POINT('Ctrl Pts',(24.7595197917227,-32.4485117525897,0.));
#41233=CARTESIAN_POINT('Ctrl Pts',(24.7595197917227,-32.4485117525897,-32.4485117525897));
#41234=CARTESIAN_POINT('Ctrl Pts',(24.7595197917227,0.,-32.4485117525897));
#41235=CARTESIAN_POINT('Ctrl Pts',(24.7595197917227,31.0321087004291,-32.4485117525897));
#41236=CARTESIAN_POINT('Ctrl Pts',(24.7595197917227,32.4162193763075,-1.44728584082667));
#41237=CARTESIAN_POINT('Ctrl Pts',(23.6563574780851,31.9852629652417,-1.42804494464108));
#41238=CARTESIAN_POINT('Ctrl Pts',(23.6563574780851,32.017126031541,-0.714377942572998));
#41239=CARTESIAN_POINT('Ctrl Pts',(23.6563574780851,32.017126031541,0.));
#41240=CARTESIAN_POINT('Ctrl Pts',(23.6563574780851,32.017126031541,32.017126031541));
#41241=CARTESIAN_POINT('Ctrl Pts',(23.6563574780851,0.,32.017126031541));
#41242=CARTESIAN_POINT('Ctrl Pts',(23.6563574780851,-32.017126031541,32.017126031541));
#41243=CARTESIAN_POINT('Ctrl Pts',(23.6563574780851,-32.017126031541,0.));
#41244=CARTESIAN_POINT('Ctrl Pts',(23.6563574780851,-32.017126031541,-32.017126031541));
#41245=CARTESIAN_POINT('Ctrl Pts',(23.6563574780851,0.,-32.017126031541));
#41246=CARTESIAN_POINT('Ctrl Pts',(23.6563574780851,30.6195533053014,-32.017126031541));
#41247=CARTESIAN_POINT('Ctrl Pts',(23.6563574780851,31.9852629652417,-1.42804494464108));
#41248=CARTESIAN_POINT('Ctrl Pts',(22.5073180101405,31.5864702700101,-1.41024006077928));
#41249=CARTESIAN_POINT('Ctrl Pts',(22.5073180101405,31.6179360671638,-0.705471068634138));
#41250=CARTESIAN_POINT('Ctrl Pts',(22.5073180101405,31.6179360671638,0.));
#41251=CARTESIAN_POINT('Ctrl Pts',(22.5073180101405,31.6179360671638,31.6179360671638));
#41252=CARTESIAN_POINT('Ctrl Pts',(22.5073180101405,0.,31.6179360671638));
#41253=CARTESIAN_POINT('Ctrl Pts',(22.5073180101405,-31.6179360671638,31.6179360671638));
#41254=CARTESIAN_POINT('Ctrl Pts',(22.5073180101405,-31.6179360671638,0.));
#41255=CARTESIAN_POINT('Ctrl Pts',(22.5073180101405,-31.6179360671638,-31.6179360671638));
#41256=CARTESIAN_POINT('Ctrl Pts',(22.5073180101405,0.,-31.6179360671638));
#41257=CARTESIAN_POINT('Ctrl Pts',(22.5073180101405,30.237788296751,-31.6179360671638));
#41258=CARTESIAN_POINT('Ctrl Pts',(22.5073180101405,31.5864702700101,-1.41024006077928));
#41259=CARTESIAN_POINT('Ctrl Pts',(21.3125219557939,31.2336232862855,-1.39448651353199));
#41260=CARTESIAN_POINT('Ctrl Pts',(21.3125219557939,31.264737584474,-0.697590373623121));
#41261=CARTESIAN_POINT('Ctrl Pts',(21.3125219557939,31.264737584474,0.));
#41262=CARTESIAN_POINT('Ctrl Pts',(21.3125219557939,31.264737584474,31.264737584474));
#41263=CARTESIAN_POINT('Ctrl Pts',(21.3125219557939,0.,31.264737584474));
#41264=CARTESIAN_POINT('Ctrl Pts',(21.3125219557939,-31.264737584474,31.264737584474));
#41265=CARTESIAN_POINT('Ctrl Pts',(21.3125219557939,-31.264737584474,0.));
#41266=CARTESIAN_POINT('Ctrl Pts',(21.3125219557939,-31.264737584474,-31.264737584474));
#41267=CARTESIAN_POINT('Ctrl Pts',(21.3125219557939,0.,-31.264737584474));
#41268=CARTESIAN_POINT('Ctrl Pts',(21.3125219557939,29.9000072055494,-31.264737584474));
#41269=CARTESIAN_POINT('Ctrl Pts',(21.3125219557939,31.2336232862855,-1.39448651353199));
#41270=CARTESIAN_POINT('Ctrl Pts',(20.0742472323676,30.9363148057487,-1.3812125919422));
#41271=CARTESIAN_POINT('Ctrl Pts',(20.0742472323676,30.9671329312955,-0.690950108671533));
#41272=CARTESIAN_POINT('Ctrl Pts',(20.0742472323676,30.9671329312955,0.));
#41273=CARTESIAN_POINT('Ctrl Pts',(20.0742472323676,30.9671329312955,30.9671329312955));
#41274=CARTESIAN_POINT('Ctrl Pts',(20.0742472323676,0.,30.9671329312955));
#41275=CARTESIAN_POINT('Ctrl Pts',(20.0742472323676,-30.9671329312955,30.9671329312955));
#41276=CARTESIAN_POINT('Ctrl Pts',(20.0742472323676,-30.9671329312955,0.));
#41277=CARTESIAN_POINT('Ctrl Pts',(20.0742472323676,-30.9671329312955,-30.9671329312955));
#41278=CARTESIAN_POINT('Ctrl Pts',(20.0742472323676,0.,-30.9671329312955));
#41279=CARTESIAN_POINT('Ctrl Pts',(20.0742472323676,29.6153932294878,-30.9671329312955));
#41280=CARTESIAN_POINT('Ctrl Pts',(20.0742472323676,30.9363148057487,-1.3812125919422));
#41281=CARTESIAN_POINT('Ctrl Pts',(18.7979917002302,30.6967495040754,-1.37051672808959));
#41282=CARTESIAN_POINT('Ctrl Pts',(18.7979917002302,30.727328979557,-0.685599514321027));
#41283=CARTESIAN_POINT('Ctrl Pts',(18.7979917002302,30.727328979557,0.));
#41284=CARTESIAN_POINT('Ctrl Pts',(18.7979917002302,30.727328979557,30.727328979557));
#41285=CARTESIAN_POINT('Ctrl Pts',(18.7979917002302,0.,30.727328979557));
#41286=CARTESIAN_POINT('Ctrl Pts',(18.7979917002302,-30.727328979557,30.727328979557));
#41287=CARTESIAN_POINT('Ctrl Pts',(18.7979917002302,-30.727328979557,0.));
#41288=CARTESIAN_POINT('Ctrl Pts',(18.7979917002302,-30.727328979557,-30.727328979557));
#41289=CARTESIAN_POINT('Ctrl Pts',(18.7979917002302,0.,-30.727328979557));
#41290=CARTESIAN_POINT('Ctrl Pts',(18.7979917002302,29.3860569087997,-30.727328979557));
#41291=CARTESIAN_POINT('Ctrl Pts',(18.7979917002302,30.6967495040754,-1.37051672808959));
#41292=CARTESIAN_POINT('Ctrl Pts',(17.4917404060759,30.5108523315028,-1.36221698336641));
#41293=CARTESIAN_POINT('Ctrl Pts',(17.4917404060759,30.5412466200144,-0.681447575979395));
#41294=CARTESIAN_POINT('Ctrl Pts',(17.4917404060759,30.5412466200144,0.));
#41295=CARTESIAN_POINT('Ctrl Pts',(17.4917404060759,30.5412466200144,30.5412466200144));
#41296=CARTESIAN_POINT('Ctrl Pts',(17.4917404060759,0.,30.5412466200144));
#41297=CARTESIAN_POINT('Ctrl Pts',(17.4917404060759,-30.5412466200144,30.5412466200144));
#41298=CARTESIAN_POINT('Ctrl Pts',(17.4917404060759,-30.5412466200144,0.));
#41299=CARTESIAN_POINT('Ctrl Pts',(17.4917404060759,-30.5412466200144,-30.5412466200144));
#41300=CARTESIAN_POINT('Ctrl Pts',(17.4917404060759,0.,-30.5412466200144));
#41301=CARTESIAN_POINT('Ctrl Pts',(17.4917404060759,29.2080971905671,-30.5412466200144));
#41302=CARTESIAN_POINT('Ctrl Pts',(17.4917404060759,30.5108523315028,-1.36221698336641));
#41303=CARTESIAN_POINT('Ctrl Pts',(16.1647270995715,30.3706357712668,-1.35595673938413));
#41304=CARTESIAN_POINT('Ctrl Pts',(16.1647270995715,30.4008903789023,-0.678315895682602));
#41305=CARTESIAN_POINT('Ctrl Pts',(16.1647270995715,30.4008903789023,0.));
#41306=CARTESIAN_POINT('Ctrl Pts',(16.1647270995715,30.4008903789023,30.4008903789023));
#41307=CARTESIAN_POINT('Ctrl Pts',(16.1647270995715,0.,30.4008903789023));
#41308=CARTESIAN_POINT('Ctrl Pts',(16.1647270995715,-30.4008903789023,30.4008903789023));
#41309=CARTESIAN_POINT('Ctrl Pts',(16.1647270995715,-30.4008903789023,0.));
#41310=CARTESIAN_POINT('Ctrl Pts',(16.1647270995715,-30.4008903789023,-30.4008903789023));
#41311=CARTESIAN_POINT('Ctrl Pts',(16.1647270995715,0.,-30.4008903789023));
#41312=CARTESIAN_POINT('Ctrl Pts',(16.1647270995715,29.0738676097412,-30.4008903789023));
#41313=CARTESIAN_POINT('Ctrl Pts',(16.1647270995715,30.3706357712668,-1.35595673938413));
#41314=CARTESIAN_POINT('Ctrl Pts',(14.8263876417415,30.2660684364343,-1.35128812515249));
#41315=CARTESIAN_POINT('Ctrl Pts',(14.8263876417415,30.2962188762246,-0.675980426451064));
#41316=CARTESIAN_POINT('Ctrl Pts',(14.8263876417415,30.2962188762246,0.));
#41317=CARTESIAN_POINT('Ctrl Pts',(14.8263876417415,30.2962188762245,30.2962188762245));
#41318=CARTESIAN_POINT('Ctrl Pts',(14.8263876417415,0.,30.2962188762246));
#41319=CARTESIAN_POINT('Ctrl Pts',(14.8263876417415,-30.2962188762245,30.2962188762245));
#41320=CARTESIAN_POINT('Ctrl Pts',(14.8263876417415,-30.2962188762246,0.));
#41321=CARTESIAN_POINT('Ctrl Pts',(14.8263876417415,-30.2962188762245,-30.2962188762245));
#41322=CARTESIAN_POINT('Ctrl Pts',(14.8263876417415,0.,-30.2962188762246));
#41323=CARTESIAN_POINT('Ctrl Pts',(14.8263876417415,28.9737651004582,-30.2962188762245));
#41324=CARTESIAN_POINT('Ctrl Pts',(14.8263876417415,30.2660684364343,-1.35128812515249));
#41325=CARTESIAN_POINT('Ctrl Pts',(13.4853470903953,30.186937862885,-1.34775518513426));
#41326=CARTESIAN_POINT('Ctrl Pts',(13.4853470903953,30.2170094744125,-0.674213077019289));
#41327=CARTESIAN_POINT('Ctrl Pts',(13.4853470903953,30.2170094744125,0.));
#41328=CARTESIAN_POINT('Ctrl Pts',(13.4853470903953,30.2170094744125,30.2170094744125));
#41329=CARTESIAN_POINT('Ctrl Pts',(13.4853470903953,0.,30.2170094744125));
#41330=CARTESIAN_POINT('Ctrl Pts',(13.4853470903953,-30.2170094744125,30.2170094744125));
#41331=CARTESIAN_POINT('Ctrl Pts',(13.4853470903953,-30.2170094744125,0.));
#41332=CARTESIAN_POINT('Ctrl Pts',(13.4853470903953,-30.2170094744125,-30.2170094744125));
#41333=CARTESIAN_POINT('Ctrl Pts',(13.4853470903953,0.,-30.2170094744125));
#41334=CARTESIAN_POINT('Ctrl Pts',(13.4853470903953,28.8980132513174,-30.2170094744125));
#41335=CARTESIAN_POINT('Ctrl Pts',(13.4853470903953,30.186937862885,-1.34775518513426));
#41336=CARTESIAN_POINT('Ctrl Pts',(12.1482076787549,30.1249424647305,-1.34498727870742));
#41337=CARTESIAN_POINT('Ctrl Pts',(12.1482076787549,30.1549523177074,-0.672828434816074));
#41338=CARTESIAN_POINT('Ctrl Pts',(12.1482076787549,30.1549523177074,0.));
#41339=CARTESIAN_POINT('Ctrl Pts',(12.1482076787549,30.1549523177074,30.1549523177074));
#41340=CARTESIAN_POINT('Ctrl Pts',(12.1482076787549,0.,30.1549523177074));
#41341=CARTESIAN_POINT('Ctrl Pts',(12.1482076787549,-30.1549523177074,30.1549523177074));
#41342=CARTESIAN_POINT('Ctrl Pts',(12.1482076787549,-30.1549523177074,0.));
#41343=CARTESIAN_POINT('Ctrl Pts',(12.1482076787549,-30.1549523177074,-30.1549523177074));
#41344=CARTESIAN_POINT('Ctrl Pts',(12.1482076787549,0.,-30.1549523177074));
#41345=CARTESIAN_POINT('Ctrl Pts',(12.1482076787549,28.8386649382978,-30.1549523177074));
#41346=CARTESIAN_POINT('Ctrl Pts',(12.1482076787549,30.1249424647305,-1.34498727870742));
#41347=CARTESIAN_POINT('Ctrl Pts',(10.8190675759626,30.0746904138676,-1.34274367710657));
#41348=CARTESIAN_POINT('Ctrl Pts',(10.8190675759626,30.1046502067769,-0.671706075536286));
#41349=CARTESIAN_POINT('Ctrl Pts',(10.8190675759626,30.1046502067769,0.));
#41350=CARTESIAN_POINT('Ctrl Pts',(10.8190675759626,30.1046502067769,30.1046502067769));
#41351=CARTESIAN_POINT('Ctrl Pts',(10.8190675759626,0.,30.1046502067769));
#41352=CARTESIAN_POINT('Ctrl Pts',(10.8190675759626,-30.1046502067769,30.1046502067769));
#41353=CARTESIAN_POINT('Ctrl Pts',(10.8190675759626,-30.1046502067769,0.));
#41354=CARTESIAN_POINT('Ctrl Pts',(10.8190675759626,-30.1046502067769,-30.1046502067769));
#41355=CARTESIAN_POINT('Ctrl Pts',(10.8190675759626,0.,-30.1046502067769));
#41356=CARTESIAN_POINT('Ctrl Pts',(10.8190675759626,28.7905585540618,-30.1046502067769));
#41357=CARTESIAN_POINT('Ctrl Pts',(10.8190675759626,30.0746904138676,-1.34274367710657));
#41358=CARTESIAN_POINT('Ctrl Pts',(9.50027713254189,30.032840404991,-1.34087520118769));
#41359=CARTESIAN_POINT('Ctrl Pts',(9.50027713254189,30.0627585077754,-0.670771372474115));
#41360=CARTESIAN_POINT('Ctrl Pts',(9.50027713254189,30.0627585077754,0.));
#41361=CARTESIAN_POINT('Ctrl Pts',(9.50027713254189,30.0627585077753,30.0627585077753));
#41362=CARTESIAN_POINT('Ctrl Pts',(9.50027713254189,0.,30.0627585077754));
#41363=CARTESIAN_POINT('Ctrl Pts',(9.5002771325419,-30.0627585077753,30.0627585077753));
#41364=CARTESIAN_POINT('Ctrl Pts',(9.5002771325419,-30.0627585077754,0.));
#41365=CARTESIAN_POINT('Ctrl Pts',(9.5002771325419,-30.0627585077753,-30.0627585077753));
#41366=CARTESIAN_POINT('Ctrl Pts',(9.50027713254189,0.,-30.0627585077754));
#41367=CARTESIAN_POINT('Ctrl Pts',(9.50027713254189,28.750495460661,-30.0627585077753));
#41368=CARTESIAN_POINT('Ctrl Pts',(9.50027713254189,30.032840404991,-1.34087520118769));
#41369=CARTESIAN_POINT('Ctrl Pts',(8.45435372222587,30.0047244129961,-1.33961990745209));
#41370=CARTESIAN_POINT('Ctrl Pts',(8.45435372222587,30.0346145072029,-0.670143413137449));
#41371=CARTESIAN_POINT('Ctrl Pts',(8.45435372222587,30.0346145072029,0.));
#41372=CARTESIAN_POINT('Ctrl Pts',(8.45435372222587,30.0346145072029,30.0346145072029));
#41373=CARTESIAN_POINT('Ctrl Pts',(8.45435372222587,0.,30.0346145072029));
#41374=CARTESIAN_POINT('Ctrl Pts',(8.45435372222587,-30.0346145072029,30.0346145072029));
#41375=CARTESIAN_POINT('Ctrl Pts',(8.45435372222587,-30.0346145072029,0.));
#41376=CARTESIAN_POINT('Ctrl Pts',(8.45435372222587,-30.0346145072029,-30.0346145072029));
#41377=CARTESIAN_POINT('Ctrl Pts',(8.45435372222587,0.,-30.0346145072029));
#41378=CARTESIAN_POINT('Ctrl Pts',(8.45435372222587,28.7235799678431,-30.0346145072029));
#41379=CARTESIAN_POINT('Ctrl Pts',(8.45435372222587,30.0047244129961,-1.33961990745209));
#41380=CARTESIAN_POINT('Ctrl Pts',(7.67514864245731,29.9863740491064,-1.33880061938141));
#41381=CARTESIAN_POINT('Ctrl Pts',(7.67514864245731,30.0162458630552,-0.669733565164174));
#41382=CARTESIAN_POINT('Ctrl Pts',(7.67514864245731,30.0162458630552,0.));
#41383=CARTESIAN_POINT('Ctrl Pts',(7.67514864245731,30.0162458630552,30.0162458630552));
#41384=CARTESIAN_POINT('Ctrl Pts',(7.67514864245731,0.,30.0162458630552));
#41385=CARTESIAN_POINT('Ctrl Pts',(7.67514864245731,-30.0162458630552,30.0162458630552));
#41386=CARTESIAN_POINT('Ctrl Pts',(7.67514864245731,-30.0162458630552,0.));
#41387=CARTESIAN_POINT('Ctrl Pts',(7.67514864245731,-30.0162458630552,-30.0162458630552));
#41388=CARTESIAN_POINT('Ctrl Pts',(7.67514864245731,0.,-30.0162458630552));
#41389=CARTESIAN_POINT('Ctrl Pts',(7.67514864245731,28.7060131294556,-30.0162458630552));
#41390=CARTESIAN_POINT('Ctrl Pts',(7.67514864245731,29.9863740491064,-1.33880061938141));
#41391=CARTESIAN_POINT('Ctrl Pts',(7.15799654185577,29.9753522996976,-1.33830853171149));
#41392=CARTESIAN_POINT('Ctrl Pts',(7.15799654185577,30.0052131340045,-0.669487398838302));
#41393=CARTESIAN_POINT('Ctrl Pts',(7.15799654185577,30.0052131340045,0.));
#41394=CARTESIAN_POINT('Ctrl Pts',(7.15799654185577,30.0052131340045,30.0052131340045));
#41395=CARTESIAN_POINT('Ctrl Pts',(7.15799654185577,0.,30.0052131340045));
#41396=CARTESIAN_POINT('Ctrl Pts',(7.15799654185577,-30.0052131340045,30.0052131340045));
#41397=CARTESIAN_POINT('Ctrl Pts',(7.15799654185577,-30.0052131340045,0.));
#41398=CARTESIAN_POINT('Ctrl Pts',(7.15799654185577,-30.0052131340045,-30.0052131340045));
#41399=CARTESIAN_POINT('Ctrl Pts',(7.15799654185577,0.,-30.0052131340045));
#41400=CARTESIAN_POINT('Ctrl Pts',(7.15799654185577,28.695461987703,-30.0052131340045));
#41401=CARTESIAN_POINT('Ctrl Pts',(7.15799654185577,29.9753522996976,-1.33830853171149));
#41402=CARTESIAN_POINT('Ctrl Pts',(6.9,29.9701443537426,-1.33807601272607));
#41403=CARTESIAN_POINT('Ctrl Pts',(6.9,30.,-0.669371081466754));
#41404=CARTESIAN_POINT('Ctrl Pts',(6.9,30.,0.));
#41405=CARTESIAN_POINT('Ctrl Pts',(6.9,30.,30.));
#41406=CARTESIAN_POINT('Ctrl Pts',(6.9,0.,30.));
#41407=CARTESIAN_POINT('Ctrl Pts',(6.9,-30.,30.));
#41408=CARTESIAN_POINT('Ctrl Pts',(6.9,-30.,0.));
#41409=CARTESIAN_POINT('Ctrl Pts',(6.9,-30.,-30.));
#41410=CARTESIAN_POINT('Ctrl Pts',(6.9,0.,-30.));
#41411=CARTESIAN_POINT('Ctrl Pts',(6.9,28.6904764110968,-30.));
#41412=CARTESIAN_POINT('Ctrl Pts',(6.9,29.9701443537426,-1.33807601272607));
#41413=CARTESIAN_POINT('Ctrl Pts',(6.9,20.5775906479515,21.8303175223207));
#41414=CARTESIAN_POINT('Ctrl Pts',(7.85773098116326,22.0288565043892,20.4889265372405));
#41415=CARTESIAN_POINT('Ctrl Pts',(8.88781981167334,23.3171626725998,19.0414114324084));
#41416=CARTESIAN_POINT('Ctrl Pts',(10.5914578196776,25.1150390010341,16.6247285680552));
#41417=CARTESIAN_POINT('Ctrl Pts',(11.2365058953701,25.7254166302984,15.703976734769));
#41418=CARTESIAN_POINT('Ctrl Pts',(12.0558885382926,26.3926147460599,14.5853792872662));
#41419=CARTESIAN_POINT('Ctrl Pts',(12.1875764958397,26.4963665374952,14.4076425286694));
#41420=CARTESIAN_POINT('Ctrl Pts',(13.194901830313,27.2691057169114,13.0552778456719));
#41421=CARTESIAN_POINT('Ctrl Pts',(14.2258982134098,27.991732600527,11.6381637544796));
#41422=CARTESIAN_POINT('Ctrl Pts',(18.2616480823244,29.9350198014187,6.95587410790868));
#41423=CARTESIAN_POINT('Ctrl Pts',(21.0496416709525,30.7693084982877,4.29983295736294));
#41424=CARTESIAN_POINT('Ctrl Pts',(25.8000196361138,32.8040277065106,1.93741001991749));
#41425=CARTESIAN_POINT('Ctrl Pts',(26.8976561124457,33.3305524688301,1.74039351523169));
#41426=CARTESIAN_POINT('Ctrl Pts',(28.0045908801237,33.8378020212277,1.58669630450145));
#41427=CARTESIAN_POINT('Ctrl Pts',(28.5235971652406,34.0754855762016,1.54532623843659));
#41428=CARTESIAN_POINT('Ctrl Pts',(29.0834839543824,34.3307100593381,1.49828854871271));
#41429=CARTESIAN_POINT('Ctrl Pts',(29.1146288039499,34.3449058451715,1.49562082188434));
#41430=CARTESIAN_POINT('Ctrl Pts',(29.5949306848436,34.5637016811193,1.45589225448014));
#41431=CARTESIAN_POINT('Ctrl Pts',(30.0492939924726,34.7685410859787,1.44682754698748));
#41432=CARTESIAN_POINT('Ctrl Pts',(30.5,34.9699609326822,1.44976976333442));
#41433=CARTESIAN_POINT('Ctrl Pts',(6.45331003273164,6.83943894028999,8.65286216739172));
#41434=CARTESIAN_POINT('Ctrl Pts',(7.20830533428676,7.28712780725476,8.29622318255583));
#41435=CARTESIAN_POINT('Ctrl Pts',(7.99924796920644,7.69991572864563,7.91909532230128));
#41436=CARTESIAN_POINT('Ctrl Pts',(9.76163642871393,8.50127829248443,7.07028372020711));
#41437=CARTESIAN_POINT('Ctrl Pts',(10.7316626231511,8.87935281282541,6.57783879792861));
#41438=CARTESIAN_POINT('Ctrl Pts',(12.6608237755523,9.49392179513702,5.67260683532433));
#41439=CARTESIAN_POINT('Ctrl Pts',(13.6376935580087,9.74868549844379,5.20677839827646));
#41440=CARTESIAN_POINT('Ctrl Pts',(14.8683081444882,10.0072371758851,4.68571756497415));
#41441=CARTESIAN_POINT('Ctrl Pts',(15.814981546047,10.1933420307132,4.28615487511135));
#41442=CARTESIAN_POINT('Ctrl Pts',(16.7774761024725,10.3417484740057,3.90183726466219));
#41443=CARTESIAN_POINT('Ctrl Pts',(18.4438470226174,10.5575964922698,3.30966453460613));
#41444=CARTESIAN_POINT('Ctrl Pts',(19.4166260537866,10.6478897990577,2.98271399009538));
#41445=CARTESIAN_POINT('Ctrl Pts',(20.8624415465505,10.7552000633453,2.58750630277728));
#41446=CARTESIAN_POINT('Ctrl Pts',(21.8144010701942,10.8125125199158,2.34040933534242));
#41447=CARTESIAN_POINT('Ctrl Pts',(22.7817704456172,10.8543372932886,2.13286375196526));
#41448=CARTESIAN_POINT('Ctrl Pts',(23.3296603631192,10.875372496282,2.03163991938105));
#41449=CARTESIAN_POINT('Ctrl Pts',(23.4469280425865,10.8796667005721,2.01025391532514));
#41450=CARTESIAN_POINT('Ctrl Pts',(23.681028881355,10.8878000542955,1.96865773783261));
#41451=CARTESIAN_POINT('Ctrl Pts',(24.09412141496,10.9009272596694,1.89824222375213));
#41452=CARTESIAN_POINT('Ctrl Pts',(24.6899984645713,10.9167861221077,1.80575737992302));
#41453=CARTESIAN_POINT('Ctrl Pts',(25.4117472347962,10.9320835607492,1.7102381255629));
#41454=CARTESIAN_POINT('Ctrl Pts',(25.8944359856995,10.9403877892626,1.65861072075243));
#41455=CARTESIAN_POINT('Ctrl Pts',(26.36694263196,10.947884133746,1.61476081138875));
#41456=CARTESIAN_POINT('Ctrl Pts',(27.2927605647397,10.9593568588011,1.54499465236547));
#41457=CARTESIAN_POINT('Ctrl Pts',(28.2852623623167,10.9616475307267,1.51981821556059));
#41458=CARTESIAN_POINT('Ctrl Pts',(29.2044123671999,10.9652006081482,1.49506529955051));
#41459=CARTESIAN_POINT('Ctrl Pts',(29.5205491106405,10.9661656603817,1.48868169066078));
#41460=CARTESIAN_POINT('Ctrl Pts',(30.1691034959588,10.9670510696507,1.48263221141176));
#41461=CARTESIAN_POINT('Ctrl Pts',(31.3134334344235,10.9664912432219,1.4864605825931));
#41462=CARTESIAN_POINT('Ctrl Pts',(32.3203424123248,10.9645690748214,1.49997009105207));
#41463=CARTESIAN_POINT('Ctrl Pts',(33.1675465322483,10.9645713457497,1.49998069520819));
#41464=CARTESIAN_POINT('Ctrl Pts',(33.4947519346946,10.9645717110255,1.49998093738942));
#41465=CARTESIAN_POINT('Ctrl Pts',(34.1540738134337,10.9645721532421,1.49998231763443));
#41466=CARTESIAN_POINT('Ctrl Pts',(34.8114511007501,10.9645737361772,1.49998580542901));
#41467=CARTESIAN_POINT('Ctrl Pts',(35.7991041415375,10.9645740230236,1.49998654292928));
#41468=CARTESIAN_POINT('Ctrl Pts',(37.7734954411133,10.9645758157225,1.49999064614178));
#41469=CARTESIAN_POINT('Ctrl Pts',(39.5833333333333,10.9645797934319,1.5));
#41470=CARTESIAN_POINT('Ctrl Pts',(40.9,10.9645797934319,1.5));
#41471=CARTESIAN_POINT('Ctrl Pts',(6.63336813585096,9.34202246898051,11.0008793183436));
#41472=CARTESIAN_POINT('Ctrl Pts',(7.389696336477,9.9106502389341,10.5126404716241));
#41473=CARTESIAN_POINT('Ctrl Pts',(8.18028889045472,10.4323217834721,10.0000669136624));
#41474=CARTESIAN_POINT('Ctrl Pts',(9.94159575574686,11.439192222287,8.85353468669098));
#41475=CARTESIAN_POINT('Ctrl Pts',(10.9109419422817,11.9102705993651,8.192010210379));
#41476=CARTESIAN_POINT('Ctrl Pts',(12.8335218625484,12.6683977976686,6.98387303125938));
#41477=CARTESIAN_POINT('Ctrl Pts',(13.8091851210584,12.9798296118147,6.36343771133683));
#41478=CARTESIAN_POINT('Ctrl Pts',(15.031077490038,13.2915570052696,5.67481209887734));
#41479=CARTESIAN_POINT('Ctrl Pts',(15.9749773134882,13.5160612446606,5.14536755152679));
#41480=CARTESIAN_POINT('Ctrl Pts',(16.930312943506,13.6911692618856,4.63930769376668));
#41481=CARTESIAN_POINT('Ctrl Pts',(18.5806860927911,13.9445588072222,3.86175938608204));
#41482=CARTESIAN_POINT('Ctrl Pts',(19.5487190419049,14.0476485209229,3.43185831734754));
#41483=CARTESIAN_POINT('Ctrl Pts',(20.9744115808251,14.1690991173096,2.9163969121787));
#41484=CARTESIAN_POINT('Ctrl Pts',(21.9189583606343,14.2328177454446,2.59280390983885));
#41485=CARTESIAN_POINT('Ctrl Pts',(22.8721113115926,14.2778669302764,2.3228415983607));
#41486=CARTESIAN_POINT('Ctrl Pts',(23.4111206282026,14.3007194584988,2.19132406241537));
#41487=CARTESIAN_POINT('Ctrl Pts',(23.5272640974126,14.3053783578069,2.16340494095902));
#41488=CARTESIAN_POINT('Ctrl Pts',(23.7586042074431,14.3141392731536,2.10919630050473));
#41489=CARTESIAN_POINT('Ctrl Pts',(24.1668594457501,14.328140925801,2.01743796447886));
#41490=CARTESIAN_POINT('Ctrl Pts',(24.7549510427123,14.3447231768684,1.89707890772752));
#41491=CARTESIAN_POINT('Ctrl Pts',(25.4661619742722,14.3604369110457,1.77296928480103));
#41492=CARTESIAN_POINT('Ctrl Pts',(25.9407936523078,14.368979185674,1.70601541029858));
#41493=CARTESIAN_POINT('Ctrl Pts',(26.4047985025954,14.3768131131951,1.64920950338613));
#41494=CARTESIAN_POINT('Ctrl Pts',(27.3109130873599,14.3886741790608,1.55899536298033));
#41495=CARTESIAN_POINT('Ctrl Pts',(28.2968127703991,14.3906288624531,1.52586579774316));
#41496=CARTESIAN_POINT('Ctrl Pts',(29.216365869052,14.3942351181099,1.49337715415662));
#41497=CARTESIAN_POINT('Ctrl Pts',(29.5273677411776,14.3952146919186,1.48510498656914));
#41498=CARTESIAN_POINT('Ctrl Pts',(30.1704748351474,14.3961140069303,1.47720108681952));
#41499=CARTESIAN_POINT('Ctrl Pts',(31.3076822233502,14.3955480332033,1.48219673215098));
#41500=CARTESIAN_POINT('Ctrl Pts',(32.3162781940782,14.3936026936296,1.49994928257769));
#41501=CARTESIAN_POINT('Ctrl Pts',(33.1684720644414,14.3936066618447,1.49996698297726));
#41502=CARTESIAN_POINT('Ctrl Pts',(33.4950641584123,14.3936073001223,1.49996744488464));
#41503=CARTESIAN_POINT('Ctrl Pts',(34.1546952525894,14.3936080728485,1.49996977575843));
#41504=CARTESIAN_POINT('Ctrl Pts',(34.8117737683131,14.3936108388537,1.49997575137036));
#41505=CARTESIAN_POINT('Ctrl Pts',(35.7994747102213,14.3936113400866,1.49997700611746));
#41506=CARTESIAN_POINT('Ctrl Pts',(37.7736758948775,14.3936144726314,1.499984023326));
#41507=CARTESIAN_POINT('Ctrl Pts',(39.5833333333333,14.3936214232436,1.5));
#41508=CARTESIAN_POINT('Ctrl Pts',(40.9,14.3936214232436,1.5));
#41509=CARTESIAN_POINT('Ctrl Pts',(6.84643360079894,15.1545575883324,16.506001665025));
#41510=CARTESIAN_POINT('Ctrl Pts',(7.61273218496773,16.0159127642118,15.7040687667121));
#41511=CARTESIAN_POINT('Ctrl Pts',(8.4126771054426,16.7980113101253,14.8690272591124));
#41512=CARTESIAN_POINT('Ctrl Pts',(10.1879439641556,18.2945580567154,13.0164926384402));
#41513=CARTESIAN_POINT('Ctrl Pts',(11.1642689802371,18.9856854823124,11.9550510602025));
#41514=CARTESIAN_POINT('Ctrl Pts',(13.1036036726265,20.0861315198186,10.022452207883));
#41515=CARTESIAN_POINT('Ctrl Pts',(14.0826172183607,20.5290484396468,9.03879487952599));
#41516=CARTESIAN_POINT('Ctrl Pts',(15.3089235211201,20.9656035967448,7.95158583831005));
#41517=CARTESIAN_POINT('Ctrl Pts',(16.2536562498252,21.2790692641439,7.11690983506512));
#41518=CARTESIAN_POINT('Ctrl Pts',(17.2094234535122,21.5156901422925,6.32372298857519));
#41519=CARTESIAN_POINT('Ctrl Pts',(18.8492103514784,21.8541559656566,5.11428176787037));
#41520=CARTESIAN_POINT('Ctrl Pts',(19.8132789859545,21.9855288021883,4.44555314736777));
#41521=CARTESIAN_POINT('Ctrl Pts',(21.2105274130181,22.1378650260473,3.65671370764621));
#41522=CARTESIAN_POINT('Ctrl Pts',(22.1435262947163,22.2155499994864,3.15760868632203));
#41523=CARTESIAN_POINT('Ctrl Pts',(23.0712019161588,22.2672966100822,2.74759983583373));
#41524=CARTESIAN_POINT('Ctrl Pts',(23.5926643019344,22.2940508574533,2.54861011877022));
#41525=CARTESIAN_POINT('Ctrl Pts',(23.7065967589743,22.2995097248259,2.50584172092972));
#41526=CARTESIAN_POINT('Ctrl Pts',(23.9324349207312,22.3096292230889,2.42316535684891));
#41527=CARTESIAN_POINT('Ctrl Pts',(24.3308966188193,22.3255066595415,2.28324508302848));
#41528=CARTESIAN_POINT('Ctrl Pts',(24.9027307486986,22.3435822260676,2.1003169439008));
#41529=CARTESIAN_POINT('Ctrl Pts',(25.59120580204,22.3601136597684,1.91242242103882));
#41530=CARTESIAN_POINT('Ctrl Pts',(26.047911616652,22.3691489781575,1.81155274261714));
#41531=CARTESIAN_POINT('Ctrl Pts',(26.4927766852064,22.3777261422413,1.72621142470535));
#41532=CARTESIAN_POINT('Ctrl Pts',(27.3538144829413,22.3904445374984,1.59133675559695));
#41533=CARTESIAN_POINT('Ctrl Pts',(28.3239440765631,22.3916143651132,1.5395372712982));
#41534=CARTESIAN_POINT('Ctrl Pts',(29.2444087331683,22.3953365265065,1.48903537353034));
#41535=CARTESIAN_POINT('Ctrl Pts',(29.5434413064007,22.3963491807022,1.4765958448865));
#41536=CARTESIAN_POINT('Ctrl Pts',(30.1738228526165,22.3972793088217,1.46445321166482));
#41537=CARTESIAN_POINT('Ctrl Pts',(31.2943937060125,22.3966964278384,1.47211763918551));
#41538=CARTESIAN_POINT('Ctrl Pts',(32.3068807810286,22.3946917099991,1.49983279134389));
#41539=CARTESIAN_POINT('Ctrl Pts',(33.1706991860565,22.3946974029307,1.49988437406509));
#41540=CARTESIAN_POINT('Ctrl Pts',(33.4958573126071,22.3946983171246,1.49988713027318));
#41541=CARTESIAN_POINT('Ctrl Pts',(34.1562063695875,22.394699425001,1.49989458266055));
#41542=CARTESIAN_POINT('Ctrl Pts',(34.8125750960604,22.3947033892012,1.49991575825725));
#41543=CARTESIAN_POINT('Ctrl Pts',(35.8003855127834,22.3947041076693,1.49991999484083));
#41544=CARTESIAN_POINT('Ctrl Pts',(37.7741287617182,22.3947085973461,1.49994455667286));
#41545=CARTESIAN_POINT('Ctrl Pts',(39.5833333333333,22.394718559471,1.5));
#41546=CARTESIAN_POINT('Ctrl Pts',(40.9,22.394718559471,1.5));
#41547=CARTESIAN_POINT('Ctrl Pts',(6.90857970435318,20.8698550272217,22.1068727166734));
#41548=CARTESIAN_POINT('Ctrl Pts',(7.67983757144493,22.0336104135999,20.991774688754));
#41549=CARTESIAN_POINT('Ctrl Pts',(8.48444928201915,23.0860770683301,19.8332461961107));
#41550=CARTESIAN_POINT('Ctrl Pts',(10.2687663769551,25.0905346149111,17.2709888357559));
#41551=CARTESIAN_POINT('Ctrl Pts',(11.2490111943913,26.0108786577409,15.8072894822424));
#41552=CARTESIAN_POINT('Ctrl Pts',(13.2067599054631,27.4745835397,13.1283892637642));
#41553=CARTESIAN_POINT('Ctrl Pts',(14.1887708824686,28.0545611646472,11.7775873547894));
#41554=CARTESIAN_POINT('Ctrl Pts',(15.4301927253883,28.6258871350548,10.2708149751555));
#41555=CARTESIAN_POINT('Ctrl Pts',(16.3793034376203,29.0320485193235,9.12509880827949));
#41556=CARTESIAN_POINT('Ctrl Pts',(17.3459407209745,29.3355313348089,8.02905385413649));
#41557=CARTESIAN_POINT('Ctrl Pts',(19.00167863971,29.7645301224029,6.36442803225957));
#41558=CARTESIAN_POINT('Ctrl Pts',(19.9708024570657,29.9249381814105,5.44984750618437));
#41559=CARTESIAN_POINT('Ctrl Pts',(21.372654162153,30.1088343166973,4.37628680649795));
#41560=CARTESIAN_POINT('Ctrl Pts',(22.3059973273548,30.2002109026536,3.69883691082952));
#41561=CARTESIAN_POINT('Ctrl Pts',(23.2278577930092,30.2581794306252,3.14826448808765));
#41562=CARTESIAN_POINT('Ctrl Pts',(23.7415516356669,30.2885183156938,2.88362049576677));
#41563=CARTESIAN_POINT('Ctrl Pts',(23.8544946510477,30.2947200062411,2.82623659223919));
#41564=CARTESIAN_POINT('Ctrl Pts',(24.0777274663495,30.3060802342176,2.71573667925149));
#41565=CARTESIAN_POINT('Ctrl Pts',(24.4711727956184,30.3236351372296,2.52895535356894));
#41566=CARTESIAN_POINT('Ctrl Pts',(25.0334457271173,30.3429441514162,2.2860141148269));
#41567=CARTESIAN_POINT('Ctrl Pts',(25.7062144884658,30.3600503901634,2.03835403030805));
#41568=CARTESIAN_POINT('Ctrl Pts',(26.1486936133437,30.3694723684121,1.90670660027131));
#41569=CARTESIAN_POINT('Ctrl Pts',(26.5774366289029,30.378713979902,1.79594947825405));
#41570=CARTESIAN_POINT('Ctrl Pts',(27.3975110717082,30.3921981334468,1.62272694197857));
#41571=CARTESIAN_POINT('Ctrl Pts',(28.3508259392473,30.3926064111245,1.55227638555954));
#41572=CARTESIAN_POINT('Ctrl Pts',(29.2723062856311,30.3964396342324,1.48380439950633));
#41573=CARTESIAN_POINT('Ctrl Pts',(29.5594622066962,30.3974855836748,1.46775103384065));
#41574=CARTESIAN_POINT('Ctrl Pts',(30.1771168569175,30.3984465770314,1.45157152773897));
#41575=CARTESIAN_POINT('Ctrl Pts',(31.281071177308,30.3978463334885,1.46177125475314));
#41576=CARTESIAN_POINT('Ctrl Pts',(32.2974559939611,30.395781840626,1.49958178095819));
#41577=CARTESIAN_POINT('Ctrl Pts',(33.1729044426912,30.3957890263381,1.49970257782127));
#41578=CARTESIAN_POINT('Ctrl Pts',(33.4966295876143,30.395790177722,1.4997109685702));
#41579=CARTESIAN_POINT('Ctrl Pts',(34.1576977268015,30.3957915749199,1.4997293265115));
#41580=CARTESIAN_POINT('Ctrl Pts',(34.8133607699291,30.3957965718591,1.4997840805116));
#41581=CARTESIAN_POINT('Ctrl Pts',(35.8012813983217,30.3957974776822,1.49979479816103));
#41582=CARTESIAN_POINT('Ctrl Pts',(37.7745713511015,30.395803137258,1.49985796376524));
#41583=CARTESIAN_POINT('Ctrl Pts',(39.5833333333333,30.3958156956984,1.5));
#41584=CARTESIAN_POINT('Ctrl Pts',(40.9,30.3958156956984,1.5));
#41585=CARTESIAN_POINT('Ctrl Pts',(6.93528330520032,24.1234099037007,25.3195110382618));
#41586=CARTESIAN_POINT('Ctrl Pts',(7.70864561497005,25.4600205488393,24.0266258397084));
#41587=CARTESIAN_POINT('Ctrl Pts',(8.51531156164572,26.6675788409113,22.6840056101462));
#41588=CARTESIAN_POINT('Ctrl Pts',(10.3033767345502,28.9634999585434,19.7178334181139));
#41589=CARTESIAN_POINT('Ctrl Pts',(11.2853975328499,30.0157138764656,18.024966824446));
#41590=CARTESIAN_POINT('Ctrl Pts',(13.2504656206425,31.6887121402305,14.920608256729));
#41591=CARTESIAN_POINT('Ctrl Pts',(14.2338911783743,32.3479754973602,13.3603265157411));
#41592=CARTESIAN_POINT('Ctrl Pts',(15.4814489736579,32.9977120049687,11.6128587845954));
#41593=CARTESIAN_POINT('Ctrl Pts',(16.4323633322631,33.457701559807,10.2891584164032));
#41594=CARTESIAN_POINT('Ctrl Pts',(17.4036580739674,33.8004278805126,9.0188416170732));
#41595=CARTESIAN_POINT('Ctrl Pts',(19.0672887678301,34.2828730898378,7.09001985912387));
#41596=CARTESIAN_POINT('Ctrl Pts',(20.039114991915,34.4604737318841,6.03348815316115));
#41597=CARTESIAN_POINT('Ctrl Pts',(21.446277848711,34.6632929668278,4.79159535501521));
#41598=CARTESIAN_POINT('Ctrl Pts',(22.3811728101676,34.7627792680184,4.01020122074906));
#41599=CARTESIAN_POINT('Ctrl Pts',(23.303259548489,34.8244923190151,3.37635643636734));
#41600=CARTESIAN_POINT('Ctrl Pts',(23.8149974822579,34.8569118346704,3.07312481135071));
#41601=CARTESIAN_POINT('Ctrl Pts',(23.9276845297169,34.8635414236982,3.00725282827679));
#41602=CARTESIAN_POINT('Ctrl Pts',(24.1501932465706,34.8756163196439,2.88055633977634));
#41603=CARTESIAN_POINT('Ctrl Pts',(24.542110623408,34.8941314993691,2.6665697947521));
#41604=CARTESIAN_POINT('Ctrl Pts',(25.1010166003944,34.9141289755488,2.38896069563576));
#41605=CARTESIAN_POINT('Ctrl Pts',(25.7673676623319,34.9315307898226,2.10719515267297));
#41606=CARTESIAN_POINT('Ctrl Pts',(26.2032614590241,34.9411502230498,1.95837832513289));
#41607=CARTESIAN_POINT('Ctrl Pts',(26.6241220770204,34.9507523611203,1.83365744353246));
#41608=CARTESIAN_POINT('Ctrl Pts',(27.4227877709102,34.9646463474544,1.64008822157602));
#41609=CARTESIAN_POINT('Ctrl Pts',(28.3660425122777,34.9646178111256,1.55920845841383));
#41610=CARTESIAN_POINT('Ctrl Pts',(29.288154079426,34.9685099768711,1.48047877405357));
#41611=CARTESIAN_POINT('Ctrl Pts',(29.5685743108623,34.9695745039167,1.46254110097229));
#41612=CARTESIAN_POINT('Ctrl Pts',(30.178956622871,34.9705522790041,1.44412472938078));
#41613=CARTESIAN_POINT('Ctrl Pts',(31.2734286330481,34.9699406754865,1.45573528147979));
#41614=CARTESIAN_POINT('Ctrl Pts',(32.2920480078112,34.9678391394654,1.49937027232429));
#41615=CARTESIAN_POINT('Ctrl Pts',(33.1741467941407,34.9678459524318,1.4995472544355));
#41616=CARTESIAN_POINT('Ctrl Pts',(33.4970538821706,34.9678470414556,1.49956078207587));
#41617=CARTESIAN_POINT('Ctrl Pts',(34.1585338443543,34.967848364944,1.49958825610694));
#41618=CARTESIAN_POINT('Ctrl Pts',(34.8137969787744,34.9678530956497,1.49967176946748));
#41619=CARTESIAN_POINT('Ctrl Pts',(35.8017811867035,34.9678539534014,1.49968797974804));
#41620=CARTESIAN_POINT('Ctrl Pts',(37.7748158892396,34.9678593117154,1.49978412416472));
#41621=CARTESIAN_POINT('Ctrl Pts',(39.5833333333333,34.967871202114,1.5));
#41622=CARTESIAN_POINT('Ctrl Pts',(40.9,34.967871202114,1.5));
#41623=CARTESIAN_POINT('Origin',(0.3,5.20850103220104,-6.86619553270279));
#41624=CARTESIAN_POINT('',(0.6,5.35130101070365,-7.13002912825054));
#41625=CARTESIAN_POINT('',(0.,5.06570105369843,-6.60236193715504));
#41626=CARTESIAN_POINT('Origin',(0.,-8.88651760185943,-2.38113521494319));
#41627=CARTESIAN_POINT('',(6.5,-8.84627910967765,-0.918184763087449));
#41628=CARTESIAN_POINT('Origin',(0.,-6.50538238691624,-6.50538238691624));
#41629=CARTESIAN_POINT('',(6.5,-5.88386150345169,-7.65368850791103));
#41630=CARTESIAN_POINT('Origin',(0.,-2.38113521494319,-8.88651760185943));
#41631=CARTESIAN_POINT('',(6.5,0.492874024900538,-10.6529279712533));
#41632=CARTESIAN_POINT('Origin',(0.,2.38113521494319,-8.88651760185943));
#41633=CARTESIAN_POINT('',(6.5,6.56519030397928,-9.00160015149379));
#41634=CARTESIAN_POINT('Origin',(0.,6.50538238691624,-6.50538238691624));
#41635=CARTESIAN_POINT('',(6.5,9.60513338590479,-4.82764163104316));
#41636=CARTESIAN_POINT('Origin',(0.,8.88651760185943,-2.38113521494319));
#41637=CARTESIAN_POINT('',(6.5,9.70736730835527,-1.04558506087479));
#41638=CARTESIAN_POINT('Origin',(0.,0.,0.));
#41639=CARTESIAN_POINT('Origin',(0.,-6.50538238691624,6.50538238691624));
#41640=CARTESIAN_POINT('',(6.5,-1.09746863550251,9.43241662545793));
#41641=CARTESIAN_POINT('Origin',(0.,-2.38113521494319,8.88651760185943));
#41642=CARTESIAN_POINT('',(6.5,4.42649419509641,8.69927356878582));
#41643=CARTESIAN_POINT('Origin',(0.,2.38113521494319,8.88651760185943));
#41644=CARTESIAN_POINT('',(6.5,7.49114572377286,5.7458263941306));
#41645=CARTESIAN_POINT('Origin',(0.,6.50538238691624,6.50538238691624));
#41646=CARTESIAN_POINT('',(6.5,8.3761967530494,3.04891351349626));
#41647=CARTESIAN_POINT('Origin',(0.,8.88651760185943,2.38113521494319));
#41648=CARTESIAN_POINT('',(6.5,8.85459461060197,1.22051134579542));
#41649=CARTESIAN_POINT('Origin',(0.,-8.88651760185943,2.38113521494319));
#41650=CARTESIAN_POINT('',(6.5,-6.69138705702868,5.95268663799753));
#41651=CARTESIAN_POINT('Origin',(6.5,11.,0.));
#41652=CARTESIAN_POINT('Origin',(41.85,0.,0.));
#41653=CARTESIAN_POINT('',(42.2,-12.,-1.46957615897682E-15));
#41654=CARTESIAN_POINT('Origin',(42.2,0.,0.));
#41655=CARTESIAN_POINT('',(41.85,-13.,-1.59204083889156E-15));
#41656=CARTESIAN_POINT('Origin',(42.6,0.,0.));
#41657=CARTESIAN_POINT('',(42.6,-11.3,-1.38385088303651E-15));
#41658=CARTESIAN_POINT('Origin',(44.2,0.,0.));
#41659=CARTESIAN_POINT('',(44.2,-9.,-1.10218211923262E-15));
#41660=CARTESIAN_POINT('Origin',(55.3,0.,0.));
#41661=CARTESIAN_POINT('',(55.5,-8.79999999999999,-1.07768918324967E-15));
#41662=CARTESIAN_POINT('Origin',(55.5,0.,0.));
#41663=CARTESIAN_POINT('',(55.3,-9.,-1.10218211923262E-15));
#41664=CARTESIAN_POINT('Origin',(55.5,7.2,0.));
#41665=CARTESIAN_POINT('',(55.5,-7.19999999999999,-8.81745695386093E-16));
#41666=CARTESIAN_POINT('Origin',(55.5,0.,0.));
#41667=CARTESIAN_POINT('Origin',(56.,0.,0.));
#41668=CARTESIAN_POINT('',(56.5,-6.2,-7.59281015471359E-16));
#41669=CARTESIAN_POINT('Origin',(56.5,0.,0.));
#41670=CARTESIAN_POINT('',(56.,-6.7,-8.20513355428727E-16));
#41671=CARTESIAN_POINT('Origin',(56.75,0.,0.));
#41672=CARTESIAN_POINT('',(57.,-5.50000000000001,-6.73555739531045E-16));
#41673=CARTESIAN_POINT('Origin',(57.,0.,0.));
#41674=CARTESIAN_POINT('',(56.75,-5.85,-7.16418377501202E-16));
#41675=CARTESIAN_POINT('Origin',(85.35,0.,0.));
#41676=CARTESIAN_POINT('',(113.7,-5.5,-6.73555739531044E-16));
#41677=CARTESIAN_POINT('Origin',(113.7,0.,0.));
#41678=CARTESIAN_POINT('',(85.35,-5.5,-6.73555739531044E-16));
#41679=CARTESIAN_POINT('Origin',(113.85,0.,0.));
#41680=CARTESIAN_POINT('',(114.,-5.2,-6.36816335556624E-16));
#41681=CARTESIAN_POINT('Origin',(114.,0.,0.));
#41682=CARTESIAN_POINT('',(113.85,-5.35,-6.55186037543834E-16));
#41683=CARTESIAN_POINT('Origin',(114.,3.3,0.));
#41684=CARTESIAN_POINT('',(114.,-3.3,-4.04133443718627E-16));
#41685=CARTESIAN_POINT('Origin',(114.,0.,0.));
#41686=CARTESIAN_POINT('Origin',(114.3,0.,0.));
#41687=CARTESIAN_POINT('',(114.6,-3.3,-4.04133443718627E-16));
#41688=CARTESIAN_POINT('Origin',(114.6,0.,0.));
#41689=CARTESIAN_POINT('',(114.3,-3.3,-4.04133443718627E-16));
#41690=CARTESIAN_POINT('Origin',(114.7,0.,0.));
#41691=CARTESIAN_POINT('',(114.8,-3.5,-4.28626379701574E-16));
#41692=CARTESIAN_POINT('Origin',(114.8,0.,0.));
#41693=CARTESIAN_POINT('',(114.7,-3.4,-4.163799117101E-16));
#41694=CARTESIAN_POINT('Origin',(135.1,0.,0.));
#41695=CARTESIAN_POINT('',(155.4,-3.5,-4.28626379701574E-16));
#41696=CARTESIAN_POINT('Origin',(155.4,0.,0.));
#41697=CARTESIAN_POINT('',(135.1,-3.5,-4.28626379701574E-16));
#41698=CARTESIAN_POINT('Origin',(155.5,0.,0.));
#41699=CARTESIAN_POINT('',(155.6,-2.9,-3.55147571752733E-16));
#41700=CARTESIAN_POINT('Origin',(155.6,0.,0.));
#41701=CARTESIAN_POINT('',(155.5,-3.2,-3.91886975727153E-16));
#41702=CARTESIAN_POINT('Origin',(156.15,0.,0.));
#41703=CARTESIAN_POINT('',(156.7,-2.9,-3.55147571752732E-16));
#41704=CARTESIAN_POINT('Origin',(156.7,0.,0.));
#41705=CARTESIAN_POINT('',(156.15,-2.9,-3.55147571752732E-16));
#41706=CARTESIAN_POINT('Origin',(156.85,0.,0.));
#41707=CARTESIAN_POINT('',(156.85,-3.2,-3.91886975727153E-16));
#41708=CARTESIAN_POINT('Origin',(165.,0.,0.));
#41709=CARTESIAN_POINT('Origin',(173.058,0.,0.));
#41710=CARTESIAN_POINT('Origin',(173.25,0.,0.));
#41711=CARTESIAN_POINT('',(173.5,-3.00000000000001,-3.67394039744207E-16));
#41712=CARTESIAN_POINT('Origin',(173.5,0.,0.));
#41713=CARTESIAN_POINT('',(173.25,-3.25,-3.9801020972289E-16));
#41714=CARTESIAN_POINT('Origin',(173.5,0.,0.));
#41715=CARTESIAN_POINT('',(0.,0.,0.));
#41716=CARTESIAN_POINT('Ctrl Pts',(1.5,9.34792819335158,0.196820971183211));
#41717=CARTESIAN_POINT('Ctrl Pts',(1.5,9.31857873039711,1.58780851273504));
#41718=CARTESIAN_POINT('Ctrl Pts',(1.5,8.63089363219759,4.34947211834324));
#41719=CARTESIAN_POINT('Ctrl Pts',(1.5,5.91232099870426,7.64758018279904));
#41720=CARTESIAN_POINT('Ctrl Pts',(1.5,2.03684458018563,9.44764359291464));
#41721=CARTESIAN_POINT('Ctrl Pts',(1.5,-2.23465367101115,9.40328083925727));
#41722=CARTESIAN_POINT('Ctrl Pts',(1.5,-6.07247560093714,7.5197369392284));
#41723=CARTESIAN_POINT('Ctrl Pts',(1.5,-8.42352750439441,4.54058319300765));
#41724=CARTESIAN_POINT('Ctrl Pts',(1.5,-9.66239336793898,0.50765700696431));
#41725=CARTESIAN_POINT('Ctrl Pts',(1.5,-9.0914057647348,-3.31385015859821));
#41726=CARTESIAN_POINT('Ctrl Pts',(1.5,-6.46482759358799,-7.19978040884221));
#41727=CARTESIAN_POINT('Ctrl Pts',(1.5,-2.7147574693153,-9.40315161601262));
#41728=CARTESIAN_POINT('Ctrl Pts',(1.5,2.03893109606151,-9.44584841818117));
#41729=CARTESIAN_POINT('Ctrl Pts',(1.5,5.91067968856048,-7.64792860715505));
#41730=CARTESIAN_POINT('Ctrl Pts',(1.5,8.63155746153459,-4.34908545280644));
#41731=CARTESIAN_POINT('Ctrl Pts',(1.5,9.3185787303843,-1.58780851274609));
#41732=CARTESIAN_POINT('Ctrl Pts',(1.5,9.34792819335161,-0.196820971181858));
#41733=CARTESIAN_POINT('Ctrl Pts',(1.45,9.39791706710028,0.197875722972423));
#41734=CARTESIAN_POINT('Ctrl Pts',(1.45,9.36841130719358,1.59627079745483));
#41735=CARTESIAN_POINT('Ctrl Pts',(1.45000000000001,8.67704692960724,4.37273923776376));
#41736=CARTESIAN_POINT('Ctrl Pts',(1.45,5.94393811041667,7.68847040785079));
#41737=CARTESIAN_POINT('Ctrl Pts',(1.45,2.0477365935102,9.49816718220173));
#41738=CARTESIAN_POINT('Ctrl Pts',(1.45,-2.24660356695236,9.45356424486553));
#41739=CARTESIAN_POINT('Ctrl Pts',(1.45,-6.10494877909688,7.55994984692236));
#41740=CARTESIAN_POINT('Ctrl Pts',(1.45,-8.46857308722318,4.56486422226556));
#41741=CARTESIAN_POINT('Ctrl Pts',(1.45,-9.71406393286648,0.510371735787382));
#41742=CARTESIAN_POINT('Ctrl Pts',(1.45,-9.14002288270658,-3.33157108555998));
#41743=CARTESIAN_POINT('Ctrl Pts',(1.45,-6.49939890496966,-7.2382822672017));
#41744=CARTESIAN_POINT('Ctrl Pts',(1.45,-2.72927477425517,-9.45343444662248));
#41745=CARTESIAN_POINT('Ctrl Pts',(1.45,2.04983424399026,-9.49636284253881));
#41746=CARTESIAN_POINT('Ctrl Pts',(1.45,5.94228810749773,-7.6888194897843));
#41747=CARTESIAN_POINT('Ctrl Pts',(1.45,8.67771429107584,-4.37235077790246));
#41748=CARTESIAN_POINT('Ctrl Pts',(1.45,9.36841130718074,-1.59627079746426));
#41749=CARTESIAN_POINT('Ctrl Pts',(1.45,9.3979170671003,-0.197875722971522));
#41750=CARTESIAN_POINT('Ctrl Pts',(1.4,9.44790594084898,0.198930474761635));
#41751=CARTESIAN_POINT('Ctrl Pts',(1.4,9.41824388399005,1.60473308217462));
#41752=CARTESIAN_POINT('Ctrl Pts',(1.40000000000001,8.72320022701689,4.39600635718428));
#41753=CARTESIAN_POINT('Ctrl Pts',(1.4,5.97555522212907,7.72936063290253));
#41754=CARTESIAN_POINT('Ctrl Pts',(1.4,2.05862860683477,9.54869077148881));
#41755=CARTESIAN_POINT('Ctrl Pts',(1.4,-2.25855346289357,9.50384765047379));
#41756=CARTESIAN_POINT('Ctrl Pts',(1.4,-6.13742195725662,7.60016275461633));
#41757=CARTESIAN_POINT('Ctrl Pts',(1.4,-8.51361867005195,4.58914525152347));
#41758=CARTESIAN_POINT('Ctrl Pts',(1.4,-9.76573449779398,0.513086464610454));
#41759=CARTESIAN_POINT('Ctrl Pts',(1.4,-9.18864000067837,-3.34929201252174));
#41760=CARTESIAN_POINT('Ctrl Pts',(1.4,-6.53397021635133,-7.27678412556119));
#41761=CARTESIAN_POINT('Ctrl Pts',(1.4,-2.74379207919505,-9.50371727723233));
#41762=CARTESIAN_POINT('Ctrl Pts',(1.4,2.06073739191902,-9.54687726689644));
#41763=CARTESIAN_POINT('Ctrl Pts',(1.4,5.97389652643498,-7.72971037241354));
#41764=CARTESIAN_POINT('Ctrl Pts',(1.4,8.72387112061707,-4.39561610299849));
#41765=CARTESIAN_POINT('Ctrl Pts',(1.4,9.41824388397717,-1.60473308218242));
#41766=CARTESIAN_POINT('Ctrl Pts',(1.4,9.44790594084899,-0.198930474761186));
#41767=CARTESIAN_POINT('Ctrl Pts',(1.35,9.49789481459768,0.199985226550847));
#41768=CARTESIAN_POINT('Ctrl Pts',(1.35,9.46807646078652,1.61319536689441));
#41769=CARTESIAN_POINT('Ctrl Pts',(1.35000000000002,8.76935352442654,4.4192734766048));
#41770=CARTESIAN_POINT('Ctrl Pts',(1.35,6.00717233384148,7.77025085795428));
#41771=CARTESIAN_POINT('Ctrl Pts',(1.35,2.06952062015934,9.59921436077589));
#41772=CARTESIAN_POINT('Ctrl Pts',(1.35,-2.27050335883478,9.55413105608205));
#41773=CARTESIAN_POINT('Ctrl Pts',(1.35,-6.16989513541637,7.64037566231029));
#41774=CARTESIAN_POINT('Ctrl Pts',(1.35,-8.55866425288072,4.61342628078139));
#41775=CARTESIAN_POINT('Ctrl Pts',(1.35,-9.81740506272147,0.515801193433526));
#41776=CARTESIAN_POINT('Ctrl Pts',(1.35,-9.23725711865016,-3.3670129394835));
#41777=CARTESIAN_POINT('Ctrl Pts',(1.35,-6.568541527733,-7.31528598392068));
#41778=CARTESIAN_POINT('Ctrl Pts',(1.35,-2.75830938413493,-9.55400010784217));
#41779=CARTESIAN_POINT('Ctrl Pts',(1.35,2.07164053984778,-9.59739169125409));
#41780=CARTESIAN_POINT('Ctrl Pts',(1.35,6.00550494537223,-7.77060125504278));
#41781=CARTESIAN_POINT('Ctrl Pts',(1.35,8.77002795015831,-4.41888142809452));
#41782=CARTESIAN_POINT('Ctrl Pts',(1.35,9.46807646077361,-1.61319536690059));
#41783=CARTESIAN_POINT('Ctrl Pts',(1.35,9.49789481459768,-0.19998522655085));
#41784=CARTESIAN_POINT('',(1.35,9.49789481459768,-0.19998522655085));
#41785=CARTESIAN_POINT('',(1.5,9.3479280542199,-0.196827565075829));
#41786=CARTESIAN_POINT('Ctrl Pts',(1.35,9.49789481459768,-0.19998522655085));
#41787=CARTESIAN_POINT('Ctrl Pts',(1.4,9.44790594084899,-0.198930474761186));
#41788=CARTESIAN_POINT('Ctrl Pts',(1.45,9.3979170671003,-0.197875722971522));
#41789=CARTESIAN_POINT('Ctrl Pts',(1.5,9.34792819335161,-0.196820971181858));
#41790=CARTESIAN_POINT('',(1.5,9.3479280542199,0.196827565075824));
#41791=CARTESIAN_POINT('Ctrl Pts',(1.5,9.34792805421988,-0.196827565075189));
#41792=CARTESIAN_POINT('Ctrl Pts',(1.5,9.31857764478916,-1.58781287596857));
#41793=CARTESIAN_POINT('Ctrl Pts',(1.5,8.63155602840585,-4.34908719035855));
#41794=CARTESIAN_POINT('Ctrl Pts',(1.5,5.91067968856048,-7.64792860715505));
#41795=CARTESIAN_POINT('Ctrl Pts',(1.5,2.03893109606151,-9.44584841818117));
#41796=CARTESIAN_POINT('Ctrl Pts',(1.5,-2.7147574693153,-9.40315161601262));
#41797=CARTESIAN_POINT('Ctrl Pts',(1.5,-6.46482759358799,-7.19978040884221));
#41798=CARTESIAN_POINT('Ctrl Pts',(1.5,-9.0914057647348,-3.31385015859821));
#41799=CARTESIAN_POINT('Ctrl Pts',(1.5,-9.66239336793898,0.50765700696431));
#41800=CARTESIAN_POINT('Ctrl Pts',(1.5,-8.42352750439441,4.54058319300765));
#41801=CARTESIAN_POINT('Ctrl Pts',(1.5,-6.07247560093714,7.5197369392284));
#41802=CARTESIAN_POINT('Ctrl Pts',(1.5,-2.23465367101115,9.40328083925727));
#41803=CARTESIAN_POINT('Ctrl Pts',(1.5,2.03684458018563,9.44764359291464));
#41804=CARTESIAN_POINT('Ctrl Pts',(1.5,5.91232099870426,7.64758018279904));
#41805=CARTESIAN_POINT('Ctrl Pts',(1.5,8.63089076836887,4.34947559267255));
#41806=CARTESIAN_POINT('Ctrl Pts',(1.5,9.31857655710787,1.58781724039989));
#41807=CARTESIAN_POINT('Ctrl Pts',(1.5,9.34792791508345,0.196834158967628));
#41808=CARTESIAN_POINT('',(1.35,9.49789481459768,0.199985226550847));
#41809=CARTESIAN_POINT('Ctrl Pts',(1.5,9.34792805421986,0.196827565076001));
#41810=CARTESIAN_POINT('Ctrl Pts',(1.45,9.39791692722763,0.197882351980178));
#41811=CARTESIAN_POINT('Ctrl Pts',(1.4,9.4479058002354,0.198937138884354));
#41812=CARTESIAN_POINT('Ctrl Pts',(1.35,9.49789467324317,0.199991925788531));
#41813=CARTESIAN_POINT('Ctrl Pts',(1.35,9.49789481459768,0.199985226550847));
#41814=CARTESIAN_POINT('Ctrl Pts',(1.35,9.46807646078652,1.61319536689441));
#41815=CARTESIAN_POINT('Ctrl Pts',(1.35000000000002,8.76935352442654,4.4192734766048));
#41816=CARTESIAN_POINT('Ctrl Pts',(1.35,6.00717233384148,7.77025085795428));
#41817=CARTESIAN_POINT('Ctrl Pts',(1.35,2.06952062015934,9.59921436077589));
#41818=CARTESIAN_POINT('Ctrl Pts',(1.35,-2.27050335883478,9.55413105608205));
#41819=CARTESIAN_POINT('Ctrl Pts',(1.35,-6.16989513541637,7.64037566231029));
#41820=CARTESIAN_POINT('Ctrl Pts',(1.35,-8.55866425288072,4.61342628078139));
#41821=CARTESIAN_POINT('Ctrl Pts',(1.35,-9.81740506272147,0.515801193433526));
#41822=CARTESIAN_POINT('Ctrl Pts',(1.35,-9.23725711865016,-3.3670129394835));
#41823=CARTESIAN_POINT('Ctrl Pts',(1.35,-6.568541527733,-7.31528598392068));
#41824=CARTESIAN_POINT('Ctrl Pts',(1.35,-2.75830938413493,-9.55400010784217));
#41825=CARTESIAN_POINT('Ctrl Pts',(1.35,2.07164053984778,-9.59739169125409));
#41826=CARTESIAN_POINT('Ctrl Pts',(1.35,6.00550494537223,-7.77060125504278));
#41827=CARTESIAN_POINT('Ctrl Pts',(1.35,8.77002795015831,-4.41888142809452));
#41828=CARTESIAN_POINT('Ctrl Pts',(1.35,9.46807646077361,-1.61319536690059));
#41829=CARTESIAN_POINT('Ctrl Pts',(1.35,9.49789481459768,-0.19998522655085));
#41830=CARTESIAN_POINT('Origin',(0.,9.49789481459768,-0.19998522655085));
#41831=CARTESIAN_POINT('',(0.15,9.49789474391925,-0.1999885761703));
#41832=CARTESIAN_POINT('',(0.,9.49789481459768,-0.19998522655085));
#41833=CARTESIAN_POINT('',(0.,9.3479280542199,-0.196827565075894));
#41834=CARTESIAN_POINT('Ctrl Pts',(0.,9.3479280542199,-0.196827565075896));
#41835=CARTESIAN_POINT('Ctrl Pts',(0.05,9.39791692722766,-0.197882351980531));
#41836=CARTESIAN_POINT('Ctrl Pts',(0.1,9.44790580023542,-0.198937138885166));
#41837=CARTESIAN_POINT('Ctrl Pts',(0.15,9.49789467324318,-0.199991925789801));
#41838=CARTESIAN_POINT('',(0.,8.14819397266823,-0.171566273307202));
#41839=CARTESIAN_POINT('',(0.,9.49789481459768,-0.19998522655085));
#41840=CARTESIAN_POINT('',(0.15,7.99822721229277,-0.168408611832295));
#41841=CARTESIAN_POINT('Ctrl Pts',(0.15,7.99822721229278,-0.168408611832294));
#41842=CARTESIAN_POINT('Ctrl Pts',(0.125000000000001,8.02322167235535,-0.168934888744779));
#41843=CARTESIAN_POINT('Ctrl Pts',(0.1,8.04821613241793,-0.169461165657263));
#41844=CARTESIAN_POINT('Ctrl Pts',(0.0500000000000007,8.09820505254308,
-0.170513719482233));
#41845=CARTESIAN_POINT('Ctrl Pts',(0.0250000000000003,8.12319951260566,
-0.171039996394718));
#41846=CARTESIAN_POINT('Ctrl Pts',(0.,8.14819397266823,-0.171566273307203));
#41847=CARTESIAN_POINT('',(1.35,7.99822721229278,-0.168408611832294));
#41848=CARTESIAN_POINT('',(0.,7.99822721229278,-0.168408611832294));
#41849=CARTESIAN_POINT('',(1.5,8.14819397266823,-0.171566273307202));
#41850=CARTESIAN_POINT('Ctrl Pts',(1.5,8.14819397266823,-0.171566273307202));
#41851=CARTESIAN_POINT('Ctrl Pts',(1.475,8.12319951260566,-0.171039996394717));
#41852=CARTESIAN_POINT('Ctrl Pts',(1.45,8.09820505254308,-0.170513719482232));
#41853=CARTESIAN_POINT('Ctrl Pts',(1.4,8.04821613241793,-0.169461165657263));
#41854=CARTESIAN_POINT('Ctrl Pts',(1.375,8.02322167235535,-0.168934888744779));
#41855=CARTESIAN_POINT('Ctrl Pts',(1.35,7.99822721229278,-0.168408611832294));
#41856=CARTESIAN_POINT('',(1.5,9.49789481459768,-0.19998522655085));
#41857=CARTESIAN_POINT('Ctrl Pts',(0.,9.49789481459768,0.199985226550847));
#41858=CARTESIAN_POINT('Ctrl Pts',(1.5,9.49789481459768,0.199985226550847));
#41859=CARTESIAN_POINT('Ctrl Pts',(0.,9.49719905300875,0.23296012982553));
#41860=CARTESIAN_POINT('Ctrl Pts',(1.5,9.49719905300875,0.23296012982553));
#41861=CARTESIAN_POINT('Ctrl Pts',(0.,9.49552283633777,0.298887663038565));
#41862=CARTESIAN_POINT('Ctrl Pts',(1.5,9.49552283633777,0.298887663038565));
#41863=CARTESIAN_POINT('Ctrl Pts',(0.,9.49215443085195,0.397712142849129));
#41864=CARTESIAN_POINT('Ctrl Pts',(1.5,9.49215443085195,0.397712142849129));
#41865=CARTESIAN_POINT('Ctrl Pts',(0.,9.48595504112623,0.529344474233868));
#41866=CARTESIAN_POINT('Ctrl Pts',(1.5,9.48595504112623,0.529344474233868));
#41867=CARTESIAN_POINT('Ctrl Pts',(0.,9.47535906724825,0.693659210071412));
#41868=CARTESIAN_POINT('Ctrl Pts',(1.5,9.47535906724825,0.693659210071412));
#41869=CARTESIAN_POINT('Ctrl Pts',(0.,9.46191727310055,0.857739457490273));
#41870=CARTESIAN_POINT('Ctrl Pts',(1.5,9.46191727310055,0.857739457490273));
#41871=CARTESIAN_POINT('Ctrl Pts',(0.,9.44563165255892,1.02156760869831));
#41872=CARTESIAN_POINT('Ctrl Pts',(1.5,9.44563165255892,1.02156760869831));
#41873=CARTESIAN_POINT('Ctrl Pts',(0.,9.42650567192302,1.18511432783379));
#41874=CARTESIAN_POINT('Ctrl Pts',(1.5,9.42650567192302,1.18511432783379));
#41875=CARTESIAN_POINT('Ctrl Pts',(0.,9.40454466499295,1.34833562021875));
#41876=CARTESIAN_POINT('Ctrl Pts',(1.5,9.40454466499295,1.34833562021875));
#41877=CARTESIAN_POINT('Ctrl Pts',(0.,9.37975553550412,1.51117719524862));
#41878=CARTESIAN_POINT('Ctrl Pts',(1.5,9.37975553550412,1.51117719524862));
#41879=CARTESIAN_POINT('Ctrl Pts',(0.,9.3521464596427,1.67357882889248));
#41880=CARTESIAN_POINT('Ctrl Pts',(1.5,9.3521464596427,1.67357882889248));
#41881=CARTESIAN_POINT('Ctrl Pts',(0.,9.32172658862998,1.83547872597431));
#41882=CARTESIAN_POINT('Ctrl Pts',(1.5,9.32172658862998,1.83547872597431));
#41883=CARTESIAN_POINT('Ctrl Pts',(0.,9.28850575136458,1.99681788239688));
#41884=CARTESIAN_POINT('Ctrl Pts',(1.5,9.28850575136458,1.99681788239688));
#41885=CARTESIAN_POINT('Ctrl Pts',(0.,9.25249415711072,2.15754444747772));
#41886=CARTESIAN_POINT('Ctrl Pts',(1.5,9.25249415711072,2.15754444747772));
#41887=CARTESIAN_POINT('Ctrl Pts',(0.,9.21370252437557,2.31761173346451));
#41888=CARTESIAN_POINT('Ctrl Pts',(1.5,9.21370252437557,2.31761173346451));
#41889=CARTESIAN_POINT('Ctrl Pts',(0.,9.17214220982581,2.47697622525282));
#41890=CARTESIAN_POINT('Ctrl Pts',(1.5,9.17214220982581,2.47697622525282));
#41891=CARTESIAN_POINT('Ctrl Pts',(0.,9.12782533724969,2.63559559022678));
#41892=CARTESIAN_POINT('Ctrl Pts',(1.5,9.12782533724969,2.63559559022678));
#41893=CARTESIAN_POINT('Ctrl Pts',(0.,9.08076492656775,2.7934266881506));
#41894=CARTESIAN_POINT('Ctrl Pts',(1.5,9.08076492656775,2.7934266881506));
#41895=CARTESIAN_POINT('Ctrl Pts',(0.,9.03097502289868,2.95042358103354));
#41896=CARTESIAN_POINT('Ctrl Pts',(1.5,9.03097502289868,2.95042358103354));
#41897=CARTESIAN_POINT('Ctrl Pts',(0.,8.97847063443715,3.10653841617385));
#41898=CARTESIAN_POINT('Ctrl Pts',(1.5,8.97847063443715,3.10653841617385));
#41899=CARTESIAN_POINT('Ctrl Pts',(0.,8.92326767038838,3.26172230913519));
#41900=CARTESIAN_POINT('Ctrl Pts',(1.5,8.92326767038838,3.26172230913519));
#41901=CARTESIAN_POINT('Ctrl Pts',(0.,8.86538287895681,3.41592622669136));
#41902=CARTESIAN_POINT('Ctrl Pts',(1.5,8.86538287895681,3.41592622669136));
#41903=CARTESIAN_POINT('Ctrl Pts',(0.,8.80483378538669,3.56910186977197));
#41904=CARTESIAN_POINT('Ctrl Pts',(1.5,8.80483378538669,3.56910186977197));
#41905=CARTESIAN_POINT('Ctrl Pts',(0.,8.74163863005133,3.7212025564438));
#41906=CARTESIAN_POINT('Ctrl Pts',(1.5,8.74163863005133,3.7212025564438));
#41907=CARTESIAN_POINT('Ctrl Pts',(0.,8.67581638707764,3.8721828611177));
#41908=CARTESIAN_POINT('Ctrl Pts',(1.5,8.67581638707764,3.8721828611177));
#41909=CARTESIAN_POINT('Ctrl Pts',(0.,8.60738678301798,4.02199825381135));
#41910=CARTESIAN_POINT('Ctrl Pts',(1.5,8.60738678301798,4.02199825381135));
#41911=CARTESIAN_POINT('Ctrl Pts',(0.,8.53637031556992,4.17060473945411));
#41912=CARTESIAN_POINT('Ctrl Pts',(1.5,8.53637031556992,4.17060473945411));
#41913=CARTESIAN_POINT('Ctrl Pts',(0.,8.46278827234408,4.31795849722051));
#41914=CARTESIAN_POINT('Ctrl Pts',(1.5,8.46278827234408,4.31795849722051));
#41915=CARTESIAN_POINT('Ctrl Pts',(0.,8.38666274968139,4.46401551987939));
#41916=CARTESIAN_POINT('Ctrl Pts',(1.5,8.38666274968139,4.46401551987939));
#41917=CARTESIAN_POINT('Ctrl Pts',(0.,8.30801663482879,4.60873178803206));
#41918=CARTESIAN_POINT('Ctrl Pts',(1.5,8.30801663482879,4.60873178803206));
#41919=CARTESIAN_POINT('Ctrl Pts',(0.,8.22687358816372,4.75206344435896));
#41920=CARTESIAN_POINT('Ctrl Pts',(1.5,8.22687358816372,4.75206344435896));
#41921=CARTESIAN_POINT('Ctrl Pts',(0.,8.14325802546687,4.89396696788329));
#41922=CARTESIAN_POINT('Ctrl Pts',(1.5,8.14325802546687,4.89396696788329));
#41923=CARTESIAN_POINT('Ctrl Pts',(0.,8.05719510024166,5.03439934825727));
#41924=CARTESIAN_POINT('Ctrl Pts',(1.5,8.05719510024166,5.03439934825727));
#41925=CARTESIAN_POINT('Ctrl Pts',(0.,7.96871068608006,5.17331826007837));
#41926=CARTESIAN_POINT('Ctrl Pts',(1.5,7.96871068608006,5.17331826007837));
#41927=CARTESIAN_POINT('Ctrl Pts',(0.,7.87783137293423,5.31068200583127));
#41928=CARTESIAN_POINT('Ctrl Pts',(1.5,7.87783137293423,5.31068200583127));
#41929=CARTESIAN_POINT('Ctrl Pts',(0.,7.78458446343339,5.44644945886476));
#41930=CARTESIAN_POINT('Ctrl Pts',(1.5,7.78458446343339,5.44644945886476));
#41931=CARTESIAN_POINT('Ctrl Pts',(0.,7.68899796924526,5.58058000640172));
#41932=CARTESIAN_POINT('Ctrl Pts',(1.5,7.68899796924526,5.58058000640172));
#41933=CARTESIAN_POINT('Ctrl Pts',(0.,7.59110060748197,5.7130334925803));
#41934=CARTESIAN_POINT('Ctrl Pts',(1.5,7.59110060748197,5.7130334925803));
#41935=CARTESIAN_POINT('Ctrl Pts',(0.,7.49092179714982,5.84377016152442));
#41936=CARTESIAN_POINT('Ctrl Pts',(1.5,7.49092179714982,5.84377016152442));
#41937=CARTESIAN_POINT('Ctrl Pts',(0.,7.38849164783963,5.97275069881958));
#41938=CARTESIAN_POINT('Ctrl Pts',(1.5,7.38849164783963,5.97275069881958));
#41939=CARTESIAN_POINT('Ctrl Pts',(0.,7.28384094846006,6.09993627301787));
#41940=CARTESIAN_POINT('Ctrl Pts',(1.5,7.28384094846006,6.09993627301787));
#41941=CARTESIAN_POINT('Ctrl Pts',(0.,7.17700115601342,6.22528857717439));
#41942=CARTESIAN_POINT('Ctrl Pts',(1.5,7.17700115601342,6.22528857717439));
#41943=CARTESIAN_POINT('Ctrl Pts',(0.,7.06800438441268,6.34876987041675));
#41944=CARTESIAN_POINT('Ctrl Pts',(1.5,7.06800438441268,6.34876987041675));
#41945=CARTESIAN_POINT('Ctrl Pts',(0.,6.95688339333978,6.47034301954938));
#41946=CARTESIAN_POINT('Ctrl Pts',(1.5,6.95688339333978,6.47034301954938));
#41947=CARTESIAN_POINT('Ctrl Pts',(0.,6.84367157878497,6.58997149692307));
#41948=CARTESIAN_POINT('Ctrl Pts',(1.5,6.84367157878497,6.58997149692307));
#41949=CARTESIAN_POINT('Ctrl Pts',(0.,6.72840296362591,6.70761937834073));
#41950=CARTESIAN_POINT('Ctrl Pts',(1.5,6.72840296362591,6.70761937834073));
#41951=CARTESIAN_POINT('Ctrl Pts',(0.,6.61111218824589,6.82325134100059));
#41952=CARTESIAN_POINT('Ctrl Pts',(1.5,6.61111218824589,6.82325134100059));
#41953=CARTESIAN_POINT('Ctrl Pts',(0.,6.4918345011908,6.93683266147689));
#41954=CARTESIAN_POINT('Ctrl Pts',(1.5,6.4918345011908,6.93683266147689));
#41955=CARTESIAN_POINT('Ctrl Pts',(0.,6.37060574986377,7.04832921373777));
#41956=CARTESIAN_POINT('Ctrl Pts',(1.5,6.37060574986377,7.04832921373777));
#41957=CARTESIAN_POINT('Ctrl Pts',(0.,6.24746236896056,7.15770748449017));
#41958=CARTESIAN_POINT('Ctrl Pts',(1.5,6.24746236896056,7.15770748449017));
#41959=CARTESIAN_POINT('Ctrl Pts',(0.,6.12244136894179,7.26493458856336));
#41960=CARTESIAN_POINT('Ctrl Pts',(1.5,6.12244136894179,7.26493458856336));
#41961=CARTESIAN_POINT('Ctrl Pts',(0.,5.99558032454086,7.3699782843317));
#41962=CARTESIAN_POINT('Ctrl Pts',(1.5,5.99558032454086,7.3699782843317));
#41963=CARTESIAN_POINT('Ctrl Pts',(0.,5.86691736330732,7.47280698917791));
#41964=CARTESIAN_POINT('Ctrl Pts',(1.5,5.86691736330732,7.47280698917791));
#41965=CARTESIAN_POINT('Ctrl Pts',(0.,5.73649115418445,7.57338979499723));
#41966=CARTESIAN_POINT('Ctrl Pts',(1.5,5.73649115418445,7.57338979499723));
#41967=CARTESIAN_POINT('Ctrl Pts',(0.,5.60434089566038,7.67169647460986));
#41968=CARTESIAN_POINT('Ctrl Pts',(1.5,5.60434089566038,7.67169647460986));
#41969=CARTESIAN_POINT('Ctrl Pts',(0.,5.47050630395207,7.76769748821551));
#41970=CARTESIAN_POINT('Ctrl Pts',(1.5,5.47050630395207,7.76769748821551));
#41971=CARTESIAN_POINT('Ctrl Pts',(0.,5.33502760122167,7.86136398989113));
#41972=CARTESIAN_POINT('Ctrl Pts',(1.5,5.33502760122167,7.86136398989113));
#41973=CARTESIAN_POINT('Ctrl Pts',(0.,5.1979455038246,7.95266783413171));
#41974=CARTESIAN_POINT('Ctrl Pts',(1.5,5.1979455038246,7.95266783413171));
#41975=CARTESIAN_POINT('Ctrl Pts',(0.,5.0593012105884,8.04158158243497));
#41976=CARTESIAN_POINT('Ctrl Pts',(1.5,5.0593012105884,8.04158158243497));
#41977=CARTESIAN_POINT('Ctrl Pts',(0.,4.9191363900222,8.12807851205385));
#41978=CARTESIAN_POINT('Ctrl Pts',(1.5,4.9191363900222,8.12807851205385));
#41979=CARTESIAN_POINT('Ctrl Pts',(0.,4.77749316755553,8.21213262479377));
#41980=CARTESIAN_POINT('Ctrl Pts',(1.5,4.77749316755553,8.21213262479377));
#41981=CARTESIAN_POINT('Ctrl Pts',(0.,4.63441411280564,8.29371865585536));
#41982=CARTESIAN_POINT('Ctrl Pts',(1.5,4.63441411280564,8.29371865585536));
#41983=CARTESIAN_POINT('Ctrl Pts',(0.,4.48994222687257,8.37281208272277));
#41984=CARTESIAN_POINT('Ctrl Pts',(1.5,4.48994222687257,8.37281208272277));
#41985=CARTESIAN_POINT('Ctrl Pts',(0.,4.34412092966134,8.44938913409869));
#41986=CARTESIAN_POINT('Ctrl Pts',(1.5,4.34412092966134,8.44938913409869));
#41987=CARTESIAN_POINT('Ctrl Pts',(0.,4.19699404656719,8.52342679605714));
#41988=CARTESIAN_POINT('Ctrl Pts',(1.5,4.19699404656719,8.52342679605714));
#41989=CARTESIAN_POINT('Ctrl Pts',(0.,4.04860579518617,8.59490281824345));
#41990=CARTESIAN_POINT('Ctrl Pts',(1.5,4.04860579518617,8.59490281824345));
#41991=CARTESIAN_POINT('Ctrl Pts',(0.,3.89900077205028,8.66379572012202));
#41992=CARTESIAN_POINT('Ctrl Pts',(1.5,3.89900077205028,8.66379572012202));
#41993=CARTESIAN_POINT('Ctrl Pts',(0.,3.74822393938623,8.73008479727191));
#41994=CARTESIAN_POINT('Ctrl Pts',(1.5,3.74822393938623,8.73008479727191));
#41995=CARTESIAN_POINT('Ctrl Pts',(0.,3.59632061189705,8.79375012773102));
#41996=CARTESIAN_POINT('Ctrl Pts',(1.5,3.59632061189705,8.79375012773102));
#41997=CARTESIAN_POINT('Ctrl Pts',(0.,3.44333644288472,8.85477257760155));
#41998=CARTESIAN_POINT('Ctrl Pts',(1.5,3.44333644288472,8.85477257760155));
#41999=CARTESIAN_POINT('Ctrl Pts',(0.,3.28931741039412,8.91313380670472));
#42000=CARTESIAN_POINT('Ctrl Pts',(1.5,3.28931741039412,8.91313380670472));
#42001=CARTESIAN_POINT('Ctrl Pts',(0.,3.13430980337712,8.96881627428495));
#42002=CARTESIAN_POINT('Ctrl Pts',(1.5,3.13430980337712,8.96881627428495));
#42003=CARTESIAN_POINT('Ctrl Pts',(0.,2.97836020787617,9.02180324476397));
#42004=CARTESIAN_POINT('Ctrl Pts',(1.5,2.97836020787617,9.02180324476397));
#42005=CARTESIAN_POINT('Ctrl Pts',(0.,2.82151549322663,9.07207879354553));
#42006=CARTESIAN_POINT('Ctrl Pts',(1.5,2.82151549322663,9.07207879354553));
#42007=CARTESIAN_POINT('Ctrl Pts',(0.,2.66382279778062,9.11962781112771));
#42008=CARTESIAN_POINT('Ctrl Pts',(1.5,2.66382279778062,9.11962781112771));
#42009=CARTESIAN_POINT('Ctrl Pts',(0.,2.50532951464783,9.16443600726607));
#42010=CARTESIAN_POINT('Ctrl Pts',(1.5,2.50532951464783,9.16443600726607));
#42011=CARTESIAN_POINT('Ctrl Pts',(0.,2.3460832774521,9.20648991518802));
#42012=CARTESIAN_POINT('Ctrl Pts',(1.5,2.3460832774521,9.20648991518802));
#42013=CARTESIAN_POINT('Ctrl Pts',(0.,2.18613194610305,9.24577689585874));
#42014=CARTESIAN_POINT('Ctrl Pts',(1.5,2.18613194610305,9.24577689585874));
#42015=CARTESIAN_POINT('Ctrl Pts',(0.,2.0255235925818,9.28228514229881));
#42016=CARTESIAN_POINT('Ctrl Pts',(1.5,2.0255235925818,9.28228514229881));
#42017=CARTESIAN_POINT('Ctrl Pts',(0.,1.86430648634783,9.31600368256167));
#42018=CARTESIAN_POINT('Ctrl Pts',(1.5,1.86430648634783,9.31600368256167));
#42019=CARTESIAN_POINT('Ctrl Pts',(0.,1.70252907975812,9.34692238276349));
#42020=CARTESIAN_POINT('Ctrl Pts',(1.5,1.70252907975812,9.34692238276349));
#42021=CARTESIAN_POINT('Ctrl Pts',(0.,1.5402399934977,9.3750319501651));
#42022=CARTESIAN_POINT('Ctrl Pts',(1.5,1.5402399934977,9.3750319501651));
#42023=CARTESIAN_POINT('Ctrl Pts',(0.,1.37748800202051,9.4003239363065));
#42024=CARTESIAN_POINT('Ctrl Pts',(1.5,1.37748800202051,9.4003239363065));
#42025=CARTESIAN_POINT('Ctrl Pts',(0.,1.21432201899992,9.42279074019417));
#42026=CARTESIAN_POINT('Ctrl Pts',(1.5,1.21432201899992,9.42279074019417));
#42027=CARTESIAN_POINT('Ctrl Pts',(0.,1.05079108253882,9.44242560995382));
#42028=CARTESIAN_POINT('Ctrl Pts',(1.5,1.05079108253882,9.44242560995382));
#42029=CARTESIAN_POINT('Ctrl Pts',(0.,0.886944340387567,9.45922264453625));
#42030=CARTESIAN_POINT('Ctrl Pts',(1.5,0.886944340387567,9.45922264453625));
#42031=CARTESIAN_POINT('Ctrl Pts',(0.,0.722831035168742,9.47317679547619));
#42032=CARTESIAN_POINT('Ctrl Pts',(1.5,0.722831035168742,9.47317679547619));
#42033=CARTESIAN_POINT('Ctrl Pts',(0.,0.558500489607787,9.48428386870474));
#42034=CARTESIAN_POINT('Ctrl Pts',(1.5,0.558500489607787,9.48428386870474));
#42035=CARTESIAN_POINT('Ctrl Pts',(0.,0.3940020917686,9.49254052641465));
#42036=CARTESIAN_POINT('Ctrl Pts',(1.5,0.3940020917686,9.49254052641465));
#42037=CARTESIAN_POINT('Ctrl Pts',(0.,0.229385280173572,9.49794428744835));
#42038=CARTESIAN_POINT('Ctrl Pts',(1.5,0.229385280173572,9.49794428744835));
#42039=CARTESIAN_POINT('Ctrl Pts',(0.,0.0646995289263127,9.5004935277393));
#42040=CARTESIAN_POINT('Ctrl Pts',(1.5,0.0646995289263127,9.5004935277393));
#42041=CARTESIAN_POINT('Ctrl Pts',(0.,-0.100005667163057,9.50018748080671));
#42042=CARTESIAN_POINT('Ctrl Pts',(1.5,-0.100005667163057,9.50018748080671));
#42043=CARTESIAN_POINT('Ctrl Pts',(0.,-0.264680807451436,9.49702623830398));
#42044=CARTESIAN_POINT('Ctrl Pts',(1.5,-0.264680807451436,9.49702623830398));
#42045=CARTESIAN_POINT('Ctrl Pts',(0.,-0.42927640033591,9.49101075062043));
#42046=CARTESIAN_POINT('Ctrl Pts',(1.5,-0.42927640033591,9.49101075062043));
#42047=CARTESIAN_POINT('Ctrl Pts',(0.,-0.593742978110499,9.48214282597012));
#42048=CARTESIAN_POINT('Ctrl Pts',(1.5,-0.593742978110499,9.48214282597012));
#42049=CARTESIAN_POINT('Ctrl Pts',(0.,-0.75803111182441,9.47042512953441));
#42050=CARTESIAN_POINT('Ctrl Pts',(1.5,-0.75803111182441,9.47042512953441));
#42051=CARTESIAN_POINT('Ctrl Pts',(0.,-0.922091426142622,9.45586118265776));
#42052=CARTESIAN_POINT('Ctrl Pts',(1.5,-0.922091426142622,9.45586118265776));
#42053=CARTESIAN_POINT('Ctrl Pts',(0.,-1.08587461420981,9.43845536209725));
#42054=CARTESIAN_POINT('Ctrl Pts',(1.5,-1.08587461420981,9.43845536209725));
#42055=CARTESIAN_POINT('Ctrl Pts',(0.,-1.24933145251863,9.41821289932518));
#42056=CARTESIAN_POINT('Ctrl Pts',(1.5,-1.24933145251863,9.41821289932518));
#42057=CARTESIAN_POINT('Ctrl Pts',(0.,-1.41241281563231,9.39513987833922));
#42058=CARTESIAN_POINT('Ctrl Pts',(1.5,-1.41241281563231,9.39513987833922));
#42059=CARTESIAN_POINT('Ctrl Pts',(0.,-1.57506969091331,9.36924323352564));
#42060=CARTESIAN_POINT('Ctrl Pts',(1.5,-1.57506969091331,9.36924323352564));
#42061=CARTESIAN_POINT('Ctrl Pts',(0.,-1.73725319325894,9.34053074757567));
#42062=CARTESIAN_POINT('Ctrl Pts',(1.5,-1.73725319325894,9.34053074757567));
#42063=CARTESIAN_POINT('Ctrl Pts',(0.,-1.89891457984514,9.30901104945495));
#42064=CARTESIAN_POINT('Ctrl Pts',(1.5,-1.89891457984514,9.30901104945495));
#42065=CARTESIAN_POINT('Ctrl Pts',(0.,-2.06000526487899,9.27469361242572));
#42066=CARTESIAN_POINT('Ctrl Pts',(1.5,-2.06000526487899,9.27469361242572));
#42067=CARTESIAN_POINT('Ctrl Pts',(0.,-2.22047683407631,9.23758875058882));
#42068=CARTESIAN_POINT('Ctrl Pts',(1.5,-2.22047683407631,9.23758875058882));
#42069=CARTESIAN_POINT('Ctrl Pts',(0.,-2.38028105914987,9.19770761547813));
#42070=CARTESIAN_POINT('Ctrl Pts',(1.5,-2.38028105914987,9.19770761547813));
#42071=CARTESIAN_POINT('Ctrl Pts',(0.,-2.53936991230918,9.15506219270728));
#42072=CARTESIAN_POINT('Ctrl Pts',(1.5,-2.53936991230918,9.15506219270728));
#42073=CARTESIAN_POINT('Ctrl Pts',(0.,-2.69769558077273,9.1096652986684));
#42074=CARTESIAN_POINT('Ctrl Pts',(1.5,-2.69769558077273,9.1096652986684));
#42075=CARTESIAN_POINT('Ctrl Pts',(0.,-2.85521048129368,9.06153057728299));
#42076=CARTESIAN_POINT('Ctrl Pts',(1.5,-2.85521048129368,9.06153057728299));
#42077=CARTESIAN_POINT('Ctrl Pts',(0.,-3.01186727428374,9.01067249530426));
#42078=CARTESIAN_POINT('Ctrl Pts',(1.5,-3.01186727428374,9.01067249530426));
#42079=CARTESIAN_POINT('Ctrl Pts',(0.,-3.16761887795222,8.95710633767099));
#42080=CARTESIAN_POINT('Ctrl Pts',(1.5,-3.16761887795222,8.95710633767099));
#42081=CARTESIAN_POINT('Ctrl Pts',(0.,-3.32241848246116,8.90084820291227));
#42082=CARTESIAN_POINT('Ctrl Pts',(1.5,-3.32241848246116,8.90084820291227));
#42083=CARTESIAN_POINT('Ctrl Pts',(0.,-3.47621956409756,8.84191499860308));
#42084=CARTESIAN_POINT('Ctrl Pts',(1.5,-3.47621956409756,8.84191499860308));
#42085=CARTESIAN_POINT('Ctrl Pts',(0.,-3.62897589946335,8.78032443687033));
#42086=CARTESIAN_POINT('Ctrl Pts',(1.5,-3.62897589946335,8.78032443687033));
#42087=CARTESIAN_POINT('Ctrl Pts',(0.,-3.78064157913952,8.71609502848983));
#42088=CARTESIAN_POINT('Ctrl Pts',(1.5,-3.78064157913952,8.71609502848983));
#42089=CARTESIAN_POINT('Ctrl Pts',(0.,-3.93117102136967,8.649246077033));
#42090=CARTESIAN_POINT('Ctrl Pts',(1.5,-3.93117102136967,8.649246077033));
#42091=CARTESIAN_POINT('Ctrl Pts',(0.,-4.08051898576423,8.57979767306322));
#42092=CARTESIAN_POINT('Ctrl Pts',(1.5,-4.08051898576423,8.57979767306322));
#42093=CARTESIAN_POINT('Ctrl Pts',(0.,-4.22864058702597,8.50777068838111));
#42094=CARTESIAN_POINT('Ctrl Pts',(1.5,-4.22864058702597,8.50777068838111));
#42095=CARTESIAN_POINT('Ctrl Pts',(0.,-4.37549130869752,8.43318677031893));
#42096=CARTESIAN_POINT('Ctrl Pts',(1.5,-4.37549130869752,8.43318677031893));
#42097=CARTESIAN_POINT('Ctrl Pts',(0.,-4.52102701626319,8.35606833467688));
#42098=CARTESIAN_POINT('Ctrl Pts',(1.5,-4.52102701626319,8.35606833467688));
#42099=CARTESIAN_POINT('Ctrl Pts',(0.,-4.66520397027454,8.27643855870735));
#42100=CARTESIAN_POINT('Ctrl Pts',(1.5,-4.66520397027454,8.27643855870735));
#42101=CARTESIAN_POINT('Ctrl Pts',(0.,-4.8079788395007,8.19432137414672));
#42102=CARTESIAN_POINT('Ctrl Pts',(1.5,-4.8079788395007,8.19432137414672));
#42103=CARTESIAN_POINT('Ctrl Pts',(0.,-4.94930871410412,8.1097414602942));
#42104=CARTESIAN_POINT('Ctrl Pts',(1.5,-4.94930871410412,8.1097414602942));
#42105=CARTESIAN_POINT('Ctrl Pts',(0.,-5.08915111884261,8.0227242371374));
#42106=CARTESIAN_POINT('Ctrl Pts',(1.5,-5.08915111884261,8.0227242371374));
#42107=CARTESIAN_POINT('Ctrl Pts',(0.,-5.22746402551034,7.93329585718089));
#42108=CARTESIAN_POINT('Ctrl Pts',(1.5,-5.22746402551034,7.93329585718089));
#42109=CARTESIAN_POINT('Ctrl Pts',(0.,-5.36420586540681,7.84148319732023));
#42110=CARTESIAN_POINT('Ctrl Pts',(1.5,-5.36420586540681,7.84148319732023));
#42111=CARTESIAN_POINT('Ctrl Pts',(0.,-5.4993355418344,7.74731385076152));
#42112=CARTESIAN_POINT('Ctrl Pts',(1.5,-5.4993355418344,7.74731385076152));
#42113=CARTESIAN_POINT('Ctrl Pts',(0.,-5.63281244262548,7.65081611898552));
#42114=CARTESIAN_POINT('Ctrl Pts',(1.5,-5.63281244262548,7.65081611898552));
#42115=CARTESIAN_POINT('Ctrl Pts',(0.,-5.76459645269993,7.55201900375617));
#42116=CARTESIAN_POINT('Ctrl Pts',(1.5,-5.76459645269993,7.55201900375617));
#42117=CARTESIAN_POINT('Ctrl Pts',(0.,-5.89464796575187,7.45095219790274));
#42118=CARTESIAN_POINT('Ctrl Pts',(1.5,-5.89464796575187,7.45095219790274));
#42119=CARTESIAN_POINT('Ctrl Pts',(0.,-6.02292789596841,7.34764607614508));
#42120=CARTESIAN_POINT('Ctrl Pts',(1.5,-6.02292789596841,7.34764607614508));
#42121=CARTESIAN_POINT('Ctrl Pts',(0.,-6.14939768978061,7.24213168596133));
#42122=CARTESIAN_POINT('Ctrl Pts',(1.5,-6.14939768978061,7.24213168596133));
#42123=CARTESIAN_POINT('Ctrl Pts',(0.,-6.27401933764807,7.13444073849797));
#42124=CARTESIAN_POINT('Ctrl Pts',(1.5,-6.27401933764807,7.13444073849797));
#42125=CARTESIAN_POINT('Ctrl Pts',(0.,-6.39675538587714,7.02460559952098));
#42126=CARTESIAN_POINT('Ctrl Pts',(1.5,-6.39675538587714,7.02460559952098));
#42127=CARTESIAN_POINT('Ctrl Pts',(0.,-6.51756894746593,6.91265927922077));
#42128=CARTESIAN_POINT('Ctrl Pts',(1.5,-6.51756894746593,6.91265927922077));
#42129=CARTESIAN_POINT('Ctrl Pts',(0.,-6.63642371298477,6.79863542205745));
#42130=CARTESIAN_POINT('Ctrl Pts',(1.5,-6.63642371298477,6.79863542205745));
#42131=CARTESIAN_POINT('Ctrl Pts',(0.,-6.75328396149252,6.68256829664553));
#42132=CARTESIAN_POINT('Ctrl Pts',(1.5,-6.75328396149252,6.68256829664553));
#42133=CARTESIAN_POINT('Ctrl Pts',(0.,-6.86811457148982,6.56449278567769));
#42134=CARTESIAN_POINT('Ctrl Pts',(1.5,-6.86811457148982,6.56449278567769));
#42135=CARTESIAN_POINT('Ctrl Pts',(0.,-6.98088103190964,6.44444437588688));
#42136=CARTESIAN_POINT('Ctrl Pts',(1.5,-6.98088103190964,6.44444437588688));
#42137=CARTESIAN_POINT('Ctrl Pts',(0.,-7.091549452039,6.32245914695077));
#42138=CARTESIAN_POINT('Ctrl Pts',(1.5,-7.091549452039,6.32245914695077));
#42139=CARTESIAN_POINT('Ctrl Pts',(0.,-7.20008657147919,6.19857376043315));
#42140=CARTESIAN_POINT('Ctrl Pts',(1.5,-7.20008657147919,6.19857376043315));
#42141=CARTESIAN_POINT('Ctrl Pts',(0.,-7.30645977014568,6.07282544876163));
#42142=CARTESIAN_POINT('Ctrl Pts',(1.5,-7.30645977014568,6.07282544876163));
#42143=CARTESIAN_POINT('Ctrl Pts',(0.,-7.41063707830778,5.94525200424091));
#42144=CARTESIAN_POINT('Ctrl Pts',(1.5,-7.41063707830778,5.94525200424091));
#42145=CARTESIAN_POINT('Ctrl Pts',(0.,-7.51258718666891,5.81589176810111));
#42146=CARTESIAN_POINT('Ctrl Pts',(1.5,-7.51258718666891,5.81589176810111));
#42147=CARTESIAN_POINT('Ctrl Pts',(0.,-7.61227945529051,5.68478361858479));
#42148=CARTESIAN_POINT('Ctrl Pts',(1.5,-7.61227945529051,5.68478361858479));
#42149=CARTESIAN_POINT('Ctrl Pts',(0.,-7.70968392255762,5.55196695906749));
#42150=CARTESIAN_POINT('Ctrl Pts',(1.5,-7.70968392255762,5.55196695906749));
#42151=CARTESIAN_POINT('Ctrl Pts',(0.,-7.80477131418672,5.41748170621113));
#42152=CARTESIAN_POINT('Ctrl Pts',(1.5,-7.80477131418672,5.41748170621113));
#42153=CARTESIAN_POINT('Ctrl Pts',(0.,-7.89751305227678,5.28136827814941));
#42154=CARTESIAN_POINT('Ctrl Pts',(1.5,-7.89751305227678,5.28136827814941));
#42155=CARTESIAN_POINT('Ctrl Pts',(0.,-7.98788126440345,5.14366758270466));
#42156=CARTESIAN_POINT('Ctrl Pts',(1.5,-7.98788126440345,5.14366758270466));
#42157=CARTESIAN_POINT('Ctrl Pts',(0.,-8.07584879147818,5.0044210047471));
#42158=CARTESIAN_POINT('Ctrl Pts',(1.5,-8.07584879147818,5.0044210047471));
#42159=CARTESIAN_POINT('Ctrl Pts',(0.,-8.16138919565165,4.86367039358384));
#42160=CARTESIAN_POINT('Ctrl Pts',(1.5,-8.16138919565165,4.86367039358384));
#42161=CARTESIAN_POINT('Ctrl Pts',(0.,-8.24447676826226,4.72145805037682));
#42162=CARTESIAN_POINT('Ctrl Pts',(1.5,-8.24447676826226,4.72145805037682));
#42163=CARTESIAN_POINT('Ctrl Pts',(0.,-8.32508653783021,4.57782671558903));
#42164=CARTESIAN_POINT('Ctrl Pts',(1.5,-8.32508653783021,4.57782671558903));
#42165=CARTESIAN_POINT('Ctrl Pts',(0.,-8.40319427809773,4.43281955645805));
#42166=CARTESIAN_POINT('Ctrl Pts',(1.5,-8.40319427809773,4.43281955645805));
#42167=CARTESIAN_POINT('Ctrl Pts',(0.,-8.47877651476408,4.28648015372245));
#42168=CARTESIAN_POINT('Ctrl Pts',(1.5,-8.47877651476408,4.28648015372245));
#42169=CARTESIAN_POINT('Ctrl Pts',(0.,-8.55181053226761,4.13885248837393));
#42170=CARTESIAN_POINT('Ctrl Pts',(1.5,-8.55181053226761,4.13885248837393));
#42171=CARTESIAN_POINT('Ctrl Pts',(0.,-8.6222743806152,3.98998092843449));
#42172=CARTESIAN_POINT('Ctrl Pts',(1.5,-8.6222743806152,3.98998092843449));
#42173=CARTESIAN_POINT('Ctrl Pts',(0.,-8.69014688225944,3.83991021575771));
#42174=CARTESIAN_POINT('Ctrl Pts',(1.5,-8.69014688225944,3.83991021575771));
#42175=CARTESIAN_POINT('Ctrl Pts',(0.,-8.75540763902411,3.68868545285334));
#42176=CARTESIAN_POINT('Ctrl Pts',(1.5,-8.75540763902411,3.68868545285334));
#42177=CARTESIAN_POINT('Ctrl Pts',(0.,-8.81803703766495,3.53635208908032));
#42178=CARTESIAN_POINT('Ctrl Pts',(1.5,-8.81803703766495,3.53635208908032));
#42179=CARTESIAN_POINT('Ctrl Pts',(0.,-8.87801625547928,3.38295590686148));
#42180=CARTESIAN_POINT('Ctrl Pts',(1.5,-8.87801625547928,3.38295590686148));
#42181=CARTESIAN_POINT('Ctrl Pts',(0.,-8.93532726596516,3.22854300791913));
#42182=CARTESIAN_POINT('Ctrl Pts',(1.5,-8.93532726596516,3.22854300791913));
#42183=CARTESIAN_POINT('Ctrl Pts',(0.,-8.98995284452996,3.07315979953049));
#42184=CARTESIAN_POINT('Ctrl Pts',(1.5,-8.98995284452996,3.07315979953049));
#42185=CARTESIAN_POINT('Ctrl Pts',(0.,-9.04187657424922,2.91685298080215));
#42186=CARTESIAN_POINT('Ctrl Pts',(1.5,-9.04187657424922,2.91685298080215));
#42187=CARTESIAN_POINT('Ctrl Pts',(0.,-9.09108285021124,2.75966952843368));
#42188=CARTESIAN_POINT('Ctrl Pts',(1.5,-9.09108285021124,2.75966952843368));
#42189=CARTESIAN_POINT('Ctrl Pts',(0.,-9.13755688391226,2.60165668249849));
#42190=CARTESIAN_POINT('Ctrl Pts',(1.5,-9.13755688391226,2.60165668249849));
#42191=CARTESIAN_POINT('Ctrl Pts',(0.,-9.18128470770249,2.44286193224103));
#42192=CARTESIAN_POINT('Ctrl Pts',(1.5,-9.18128470770249,2.44286193224103));
#42193=CARTESIAN_POINT('Ctrl Pts',(0.,-9.2222531792836,2.28333300188963));
#42194=CARTESIAN_POINT('Ctrl Pts',(1.5,-9.2222531792836,2.28333300188963));
#42195=CARTESIAN_POINT('Ctrl Pts',(0.,-9.26044998625764,2.12311783648397));
#42196=CARTESIAN_POINT('Ctrl Pts',(1.5,-9.26044998625764,2.12311783648397));
#42197=CARTESIAN_POINT('Ctrl Pts',(0.,-9.29586364922275,1.96226458731596));
#42198=CARTESIAN_POINT('Ctrl Pts',(1.5,-9.29586364922275,1.96226458731596));
#42199=CARTESIAN_POINT('Ctrl Pts',(0.,-9.32848352492098,1.80082159738338));
#42200=CARTESIAN_POINT('Ctrl Pts',(1.5,-9.32848352492098,1.80082159738338));
#42201=CARTESIAN_POINT('Ctrl Pts',(0.,-9.35829980943804,1.63883738685563));
#42202=CARTESIAN_POINT('Ctrl Pts',(1.5,-9.35829980943804,1.63883738685563));
#42203=CARTESIAN_POINT('Ctrl Pts',(0.,-9.38530354145569,1.47636063855043));
#42204=CARTESIAN_POINT('Ctrl Pts',(1.5,-9.38530354145569,1.47636063855043));
#42205=CARTESIAN_POINT('Ctrl Pts',(0.,-9.40948660555648,1.31344018342081));
#42206=CARTESIAN_POINT('Ctrl Pts',(1.5,-9.40948660555648,1.31344018342081));
#42207=CARTESIAN_POINT('Ctrl Pts',(0.,-9.43084173404745,1.15012498578247));
#42208=CARTESIAN_POINT('Ctrl Pts',(1.5,-9.43084173404745,1.15012498578247));
#42209=CARTESIAN_POINT('Ctrl Pts',(0.,-9.44936250883668,0.986464128549687));
#42210=CARTESIAN_POINT('Ctrl Pts',(1.5,-9.44936250883668,0.986464128549687));
#42211=CARTESIAN_POINT('Ctrl Pts',(0.,-9.46504336336294,0.822506798478501));
#42212=CARTESIAN_POINT('Ctrl Pts',(1.5,-9.46504336336294,0.822506798478501));
#42213=CARTESIAN_POINT('Ctrl Pts',(0.,-9.4778795845785,0.658302271416469));
#42214=CARTESIAN_POINT('Ctrl Pts',(1.5,-9.4778795845785,0.658302271416469));
#42215=CARTESIAN_POINT('Ctrl Pts',(0.,-9.48786731498507,0.493899897557971));
#42216=CARTESIAN_POINT('Ctrl Pts',(1.5,-9.48786731498507,0.493899897557971));
#42217=CARTESIAN_POINT('Ctrl Pts',(0.,-9.49500355317182,0.329349086569191));
#42218=CARTESIAN_POINT('Ctrl Pts',(1.5,-9.49500355317182,0.329349086569191));
#42219=CARTESIAN_POINT('Ctrl Pts',(0.,-9.49928615440655,0.164699292716903));
#42220=CARTESIAN_POINT('Ctrl Pts',(1.5,-9.49928615440655,0.164699292716903));
#42221=CARTESIAN_POINT('Ctrl Pts',(0.,-9.50071383128047,6.88023856637576E-14));
#42222=CARTESIAN_POINT('Ctrl Pts',(1.5,-9.50071383128047,6.88023856637576E-14));
#42223=CARTESIAN_POINT('Ctrl Pts',(0.,-9.49928615440671,-0.164699292716751));
#42224=CARTESIAN_POINT('Ctrl Pts',(1.5,-9.49928615440671,-0.164699292716751));
#42225=CARTESIAN_POINT('Ctrl Pts',(0.,-9.49500355317206,-0.329349086569028));
#42226=CARTESIAN_POINT('Ctrl Pts',(1.5,-9.49500355317206,-0.329349086569028));
#42227=CARTESIAN_POINT('Ctrl Pts',(0.,-9.48786731498525,-0.493899897557803));
#42228=CARTESIAN_POINT('Ctrl Pts',(1.5,-9.48786731498525,-0.493899897557803));
#42229=CARTESIAN_POINT('Ctrl Pts',(0.,-9.4778795845786,-0.658302271416311));
#42230=CARTESIAN_POINT('Ctrl Pts',(1.5,-9.4778795845786,-0.658302271416311));
#42231=CARTESIAN_POINT('Ctrl Pts',(0.,-9.46504336336295,-0.822506798478354));
#42232=CARTESIAN_POINT('Ctrl Pts',(1.5,-9.46504336336295,-0.822506798478354));
#42233=CARTESIAN_POINT('Ctrl Pts',(0.,-9.44936250883662,-0.986464128549568));
#42234=CARTESIAN_POINT('Ctrl Pts',(1.5,-9.44936250883662,-0.986464128549568));
#42235=CARTESIAN_POINT('Ctrl Pts',(0.,-9.43084173404737,-1.15012498578238));
#42236=CARTESIAN_POINT('Ctrl Pts',(1.5,-9.43084173404737,-1.15012498578238));
#42237=CARTESIAN_POINT('Ctrl Pts',(0.,-9.40948660555644,-1.31344018342071));
#42238=CARTESIAN_POINT('Ctrl Pts',(1.5,-9.40948660555644,-1.31344018342071));
#42239=CARTESIAN_POINT('Ctrl Pts',(0.,-9.38530354145571,-1.47636063855032));
#42240=CARTESIAN_POINT('Ctrl Pts',(1.5,-9.38530354145571,-1.47636063855032));
#42241=CARTESIAN_POINT('Ctrl Pts',(0.,-9.35829980943809,-1.63883738685548));
#42242=CARTESIAN_POINT('Ctrl Pts',(1.5,-9.35829980943809,-1.63883738685548));
#42243=CARTESIAN_POINT('Ctrl Pts',(0.,-9.32848352492095,-1.80082159738323));
#42244=CARTESIAN_POINT('Ctrl Pts',(1.5,-9.32848352492095,-1.80082159738323));
#42245=CARTESIAN_POINT('Ctrl Pts',(0.,-9.29586364922265,-1.96226458731583));
#42246=CARTESIAN_POINT('Ctrl Pts',(1.5,-9.29586364922265,-1.96226458731583));
#42247=CARTESIAN_POINT('Ctrl Pts',(0.,-9.26044998625752,-2.12311783648386));
#42248=CARTESIAN_POINT('Ctrl Pts',(1.5,-9.26044998625752,-2.12311783648386));
#42249=CARTESIAN_POINT('Ctrl Pts',(0.,-9.22225317928356,-2.28333300188952));
#42250=CARTESIAN_POINT('Ctrl Pts',(1.5,-9.22225317928356,-2.28333300188952));
#42251=CARTESIAN_POINT('Ctrl Pts',(0.,-9.18128470770254,-2.44286193224091));
#42252=CARTESIAN_POINT('Ctrl Pts',(1.5,-9.18128470770254,-2.44286193224091));
#42253=CARTESIAN_POINT('Ctrl Pts',(0.,-9.13755688391234,-2.60165668249832));
#42254=CARTESIAN_POINT('Ctrl Pts',(1.5,-9.13755688391234,-2.60165668249832));
#42255=CARTESIAN_POINT('Ctrl Pts',(0.,-9.09108285021127,-2.75966952843345));
#42256=CARTESIAN_POINT('Ctrl Pts',(1.5,-9.09108285021127,-2.75966952843345));
#42257=CARTESIAN_POINT('Ctrl Pts',(0.,-9.04187657424916,-2.91685298080189));
#42258=CARTESIAN_POINT('Ctrl Pts',(1.5,-9.04187657424916,-2.91685298080189));
#42259=CARTESIAN_POINT('Ctrl Pts',(0.,-8.9899528445299,-3.07315979953029));
#42260=CARTESIAN_POINT('Ctrl Pts',(1.5,-8.9899528445299,-3.07315979953029));
#42261=CARTESIAN_POINT('Ctrl Pts',(0.,-8.9353272659652,-3.22854300791901));
#42262=CARTESIAN_POINT('Ctrl Pts',(1.5,-8.9353272659652,-3.22854300791901));
#42263=CARTESIAN_POINT('Ctrl Pts',(0.,-8.87801625547945,-3.38295590686141));
#42264=CARTESIAN_POINT('Ctrl Pts',(1.5,-8.87801625547945,-3.38295590686141));
#42265=CARTESIAN_POINT('Ctrl Pts',(0.,-8.81803703766518,-3.53635208908027));
#42266=CARTESIAN_POINT('Ctrl Pts',(1.5,-8.81803703766518,-3.53635208908027));
#42267=CARTESIAN_POINT('Ctrl Pts',(0.,-8.75540763902434,-3.68868545285331));
#42268=CARTESIAN_POINT('Ctrl Pts',(1.5,-8.75540763902434,-3.68868545285331));
#42269=CARTESIAN_POINT('Ctrl Pts',(0.,-8.6901468822596,-3.83991021575765));
#42270=CARTESIAN_POINT('Ctrl Pts',(1.5,-8.6901468822596,-3.83991021575765));
#42271=CARTESIAN_POINT('Ctrl Pts',(0.,-8.62227438061525,-3.98998092843437));
#42272=CARTESIAN_POINT('Ctrl Pts',(1.5,-8.62227438061525,-3.98998092843437));
#42273=CARTESIAN_POINT('Ctrl Pts',(0.,-8.55181053226757,-4.13885248837375));
#42274=CARTESIAN_POINT('Ctrl Pts',(1.5,-8.55181053226757,-4.13885248837375));
#42275=CARTESIAN_POINT('Ctrl Pts',(0.,-8.47877651476402,-4.28648015372226));
#42276=CARTESIAN_POINT('Ctrl Pts',(1.5,-8.47877651476402,-4.28648015372226));
#42277=CARTESIAN_POINT('Ctrl Pts',(0.,-8.40319427809771,-4.43281955645792));
#42278=CARTESIAN_POINT('Ctrl Pts',(1.5,-8.40319427809771,-4.43281955645792));
#42279=CARTESIAN_POINT('Ctrl Pts',(0.,-8.32508653783024,-4.57782671558895));
#42280=CARTESIAN_POINT('Ctrl Pts',(1.5,-8.32508653783024,-4.57782671558895));
#42281=CARTESIAN_POINT('Ctrl Pts',(0.,-8.24447676826233,-4.72145805037673));
#42282=CARTESIAN_POINT('Ctrl Pts',(1.5,-8.24447676826233,-4.72145805037673));
#42283=CARTESIAN_POINT('Ctrl Pts',(0.,-8.16138919565173,-4.86367039358363));
#42284=CARTESIAN_POINT('Ctrl Pts',(1.5,-8.16138919565173,-4.86367039358363));
#42285=CARTESIAN_POINT('Ctrl Pts',(0.,-8.07584879147822,-5.00442100474676));
#42286=CARTESIAN_POINT('Ctrl Pts',(1.5,-8.07584879147822,-5.00442100474676));
#42287=CARTESIAN_POINT('Ctrl Pts',(0.,-7.98788126440344,-5.14366758270425));
#42288=CARTESIAN_POINT('Ctrl Pts',(1.5,-7.98788126440344,-5.14366758270425));
#42289=CARTESIAN_POINT('Ctrl Pts',(0.,-7.89751305227676,-5.28136827814908));
#42290=CARTESIAN_POINT('Ctrl Pts',(1.5,-7.89751305227676,-5.28136827814908));
#42291=CARTESIAN_POINT('Ctrl Pts',(0.,-7.80477131418679,-5.41748170621101));
#42292=CARTESIAN_POINT('Ctrl Pts',(1.5,-7.80477131418679,-5.41748170621101));
#42293=CARTESIAN_POINT('Ctrl Pts',(0.,-7.7096839225578,-5.55196695906763));
#42294=CARTESIAN_POINT('Ctrl Pts',(1.5,-7.7096839225578,-5.55196695906763));
#42295=CARTESIAN_POINT('Ctrl Pts',(0.,-7.61227945529079,-5.68478361858509));
#42296=CARTESIAN_POINT('Ctrl Pts',(1.5,-7.61227945529079,-5.68478361858509));
#42297=CARTESIAN_POINT('Ctrl Pts',(0.,-7.51258718666918,-5.81589176810141));
#42298=CARTESIAN_POINT('Ctrl Pts',(1.5,-7.51258718666918,-5.81589176810141));
#42299=CARTESIAN_POINT('Ctrl Pts',(0.,-7.41063707830798,-5.94525200424106));
#42300=CARTESIAN_POINT('Ctrl Pts',(1.5,-7.41063707830798,-5.94525200424106));
#42301=CARTESIAN_POINT('Ctrl Pts',(0.,-7.30645977014577,-6.07282544876153));
#42302=CARTESIAN_POINT('Ctrl Pts',(1.5,-7.30645977014577,-6.07282544876153));
#42303=CARTESIAN_POINT('Ctrl Pts',(0.,-7.20008657147914,-6.19857376043277));
#42304=CARTESIAN_POINT('Ctrl Pts',(1.5,-7.20008657147914,-6.19857376043277));
#42305=CARTESIAN_POINT('Ctrl Pts',(0.,-7.09154945203894,-6.32245914695025));
#42306=CARTESIAN_POINT('Ctrl Pts',(1.5,-7.09154945203894,-6.32245914695025));
#42307=CARTESIAN_POINT('Ctrl Pts',(0.,-6.98088103190963,-6.44444437588636));
#42308=CARTESIAN_POINT('Ctrl Pts',(1.5,-6.98088103190963,-6.44444437588636));
#42309=CARTESIAN_POINT('Ctrl Pts',(0.,-6.86811457148987,-6.56449278567735));
#42310=CARTESIAN_POINT('Ctrl Pts',(1.5,-6.86811457148987,-6.56449278567735));
#42311=CARTESIAN_POINT('Ctrl Pts',(0.,-6.75328396149262,-6.68256829664545));
#42312=CARTESIAN_POINT('Ctrl Pts',(1.5,-6.75328396149262,-6.68256829664545));
#42313=CARTESIAN_POINT('Ctrl Pts',(0.,-6.63642371298489,-6.79863542205757));
#42314=CARTESIAN_POINT('Ctrl Pts',(1.5,-6.63642371298489,-6.79863542205757));
#42315=CARTESIAN_POINT('Ctrl Pts',(0.,-6.51756894746606,-6.91265927922096));
#42316=CARTESIAN_POINT('Ctrl Pts',(1.5,-6.51756894746606,-6.91265927922096));
#42317=CARTESIAN_POINT('Ctrl Pts',(0.,-6.39675538587726,-7.02460559952114));
#42318=CARTESIAN_POINT('Ctrl Pts',(1.5,-6.39675538587726,-7.02460559952114));
#42319=CARTESIAN_POINT('Ctrl Pts',(0.,-6.27401933764821,-7.13444073849804));
#42320=CARTESIAN_POINT('Ctrl Pts',(1.5,-6.27401933764821,-7.13444073849804));
#42321=CARTESIAN_POINT('Ctrl Pts',(0.,-6.14939768978072,-7.24213168596124));
#42322=CARTESIAN_POINT('Ctrl Pts',(1.5,-6.14939768978072,-7.24213168596124));
#42323=CARTESIAN_POINT('Ctrl Pts',(0.,-6.02292789596846,-7.34764607614482));
#42324=CARTESIAN_POINT('Ctrl Pts',(1.5,-6.02292789596846,-7.34764607614482));
#42325=CARTESIAN_POINT('Ctrl Pts',(0.,-5.89464796575191,-7.45095219790239));
#42326=CARTESIAN_POINT('Ctrl Pts',(1.5,-5.89464796575191,-7.45095219790239));
#42327=CARTESIAN_POINT('Ctrl Pts',(0.,-5.76459645269994,-7.55201900375578));
#42328=CARTESIAN_POINT('Ctrl Pts',(1.5,-5.76459645269994,-7.55201900375578));
#42329=CARTESIAN_POINT('Ctrl Pts',(0.,-5.63281244262552,-7.65081611898521));
#42330=CARTESIAN_POINT('Ctrl Pts',(1.5,-5.63281244262552,-7.65081611898521));
#42331=CARTESIAN_POINT('Ctrl Pts',(0.,-5.4993355418345,-7.74731385076143));
#42332=CARTESIAN_POINT('Ctrl Pts',(1.5,-5.4993355418345,-7.74731385076143));
#42333=CARTESIAN_POINT('Ctrl Pts',(0.,-5.36420586540701,-7.84148319732041));
#42334=CARTESIAN_POINT('Ctrl Pts',(1.5,-5.36420586540701,-7.84148319732041));
#42335=CARTESIAN_POINT('Ctrl Pts',(0.,-5.22746402551057,-7.93329585718124));
#42336=CARTESIAN_POINT('Ctrl Pts',(1.5,-5.22746402551057,-7.93329585718124));
#42337=CARTESIAN_POINT('Ctrl Pts',(0.,-5.08915111884281,-8.02272423713777));
#42338=CARTESIAN_POINT('Ctrl Pts',(1.5,-5.08915111884281,-8.02272423713777));
#42339=CARTESIAN_POINT('Ctrl Pts',(0.,-4.94930871410428,-8.1097414602944));
#42340=CARTESIAN_POINT('Ctrl Pts',(1.5,-4.94930871410428,-8.1097414602944));
#42341=CARTESIAN_POINT('Ctrl Pts',(0.,-4.80797883950082,-8.19432137414666));
#42342=CARTESIAN_POINT('Ctrl Pts',(1.5,-4.80797883950082,-8.19432137414666));
#42343=CARTESIAN_POINT('Ctrl Pts',(0.,-4.66520397027463,-8.27643855870703));
#42344=CARTESIAN_POINT('Ctrl Pts',(1.5,-4.66520397027463,-8.27643855870703));
#42345=CARTESIAN_POINT('Ctrl Pts',(0.,-4.52102701626329,-8.35606833467635));
#42346=CARTESIAN_POINT('Ctrl Pts',(1.5,-4.52102701626329,-8.35606833467635));
#42347=CARTESIAN_POINT('Ctrl Pts',(0.,-4.37549130869765,-8.43318677031836));
#42348=CARTESIAN_POINT('Ctrl Pts',(1.5,-4.37549130869765,-8.43318677031836));
#42349=CARTESIAN_POINT('Ctrl Pts',(0.,-4.22864058702611,-8.50777068838071));
#42350=CARTESIAN_POINT('Ctrl Pts',(1.5,-4.22864058702611,-8.50777068838071));
#42351=CARTESIAN_POINT('Ctrl Pts',(0.,-4.08051898576436,-8.57979767306315));
#42352=CARTESIAN_POINT('Ctrl Pts',(1.5,-4.08051898576436,-8.57979767306315));
#42353=CARTESIAN_POINT('Ctrl Pts',(0.,-3.93117102136977,-8.64924607703331));
#42354=CARTESIAN_POINT('Ctrl Pts',(1.5,-3.93117102136977,-8.64924607703331));
#42355=CARTESIAN_POINT('Ctrl Pts',(0.,-3.78064157913962,-8.71609502849035));
#42356=CARTESIAN_POINT('Ctrl Pts',(1.5,-3.78064157913962,-8.71609502849035));
#42357=CARTESIAN_POINT('Ctrl Pts',(0.,-3.62897589946344,-8.78032443687085));
#42358=CARTESIAN_POINT('Ctrl Pts',(1.5,-3.62897589946344,-8.78032443687085));
#42359=CARTESIAN_POINT('Ctrl Pts',(0.,-3.47621956409764,-8.84191499860338));
#42360=CARTESIAN_POINT('Ctrl Pts',(1.5,-3.47621956409764,-8.84191499860338));
#42361=CARTESIAN_POINT('Ctrl Pts',(0.,-3.32241848246127,-8.90084820291222));
#42362=CARTESIAN_POINT('Ctrl Pts',(1.5,-3.32241848246127,-8.90084820291222));
#42363=CARTESIAN_POINT('Ctrl Pts',(0.,-3.16761887795243,-8.95710633767057));
#42364=CARTESIAN_POINT('Ctrl Pts',(1.5,-3.16761887795243,-8.95710633767057));
#42365=CARTESIAN_POINT('Ctrl Pts',(0.,-3.01186727428406,-9.01067249530362));
#42366=CARTESIAN_POINT('Ctrl Pts',(1.5,-3.01186727428406,-9.01067249530362));
#42367=CARTESIAN_POINT('Ctrl Pts',(0.,-2.85521048129404,-9.06153057728234));
#42368=CARTESIAN_POINT('Ctrl Pts',(1.5,-2.85521048129404,-9.06153057728234));
#42369=CARTESIAN_POINT('Ctrl Pts',(0.,-2.69769558077302,-9.10966529866801));
#42370=CARTESIAN_POINT('Ctrl Pts',(1.5,-2.69769558077302,-9.10966529866801));
#42371=CARTESIAN_POINT('Ctrl Pts',(0.,-2.53936991230932,-9.15506219270726));
#42372=CARTESIAN_POINT('Ctrl Pts',(1.5,-2.53936991230932,-9.15506219270726));
#42373=CARTESIAN_POINT('Ctrl Pts',(0.,-2.38028105914982,-9.19770761547843));
#42374=CARTESIAN_POINT('Ctrl Pts',(1.5,-2.38028105914982,-9.19770761547843));
#42375=CARTESIAN_POINT('Ctrl Pts',(0.,-2.22047683407611,-9.23758875058925));
#42376=CARTESIAN_POINT('Ctrl Pts',(1.5,-2.22047683407611,-9.23758875058925));
#42377=CARTESIAN_POINT('Ctrl Pts',(0.,-2.06000526487878,-9.27469361242608));
#42378=CARTESIAN_POINT('Ctrl Pts',(1.5,-2.06000526487878,-9.27469361242608));
#42379=CARTESIAN_POINT('Ctrl Pts',(0.,-1.89891457984506,-9.30901104945512));
#42380=CARTESIAN_POINT('Ctrl Pts',(1.5,-1.89891457984506,-9.30901104945512));
#42381=CARTESIAN_POINT('Ctrl Pts',(0.,-1.73725319325908,-9.34053074757563));
#42382=CARTESIAN_POINT('Ctrl Pts',(1.5,-1.73725319325908,-9.34053074757563));
#42383=CARTESIAN_POINT('Ctrl Pts',(0.,-1.57506969091364,-9.36924323352547));
#42384=CARTESIAN_POINT('Ctrl Pts',(1.5,-1.57506969091364,-9.36924323352547));
#42385=CARTESIAN_POINT('Ctrl Pts',(0.,-1.41241281563273,-9.39513987833904));
#42386=CARTESIAN_POINT('Ctrl Pts',(1.5,-1.41241281563273,-9.39513987833904));
#42387=CARTESIAN_POINT('Ctrl Pts',(0.,-1.249331452519,-9.41821289932504));
#42388=CARTESIAN_POINT('Ctrl Pts',(1.5,-1.249331452519,-9.41821289932504));
#42389=CARTESIAN_POINT('Ctrl Pts',(0.,-1.08587461421005,-9.43845536209718));
#42390=CARTESIAN_POINT('Ctrl Pts',(1.5,-1.08587461421005,-9.43845536209718));
#42391=CARTESIAN_POINT('Ctrl Pts',(0.,-0.922091426142751,-9.45586118265774));
#42392=CARTESIAN_POINT('Ctrl Pts',(1.5,-0.922091426142751,-9.45586118265774));
#42393=CARTESIAN_POINT('Ctrl Pts',(0.,-0.758031111824466,-9.47042512953444));
#42394=CARTESIAN_POINT('Ctrl Pts',(1.5,-0.758031111824466,-9.47042512953444));
#42395=CARTESIAN_POINT('Ctrl Pts',(0.,-0.593742978110514,-9.48214282597024));
#42396=CARTESIAN_POINT('Ctrl Pts',(1.5,-0.593742978110514,-9.48214282597024));
#42397=CARTESIAN_POINT('Ctrl Pts',(0.,-0.429276400335928,-9.49101075062059));
#42398=CARTESIAN_POINT('Ctrl Pts',(1.5,-0.429276400335928,-9.49101075062059));
#42399=CARTESIAN_POINT('Ctrl Pts',(0.,-0.264680807451509,-9.49702623830412));
#42400=CARTESIAN_POINT('Ctrl Pts',(1.5,-0.264680807451509,-9.49702623830412));
#42401=CARTESIAN_POINT('Ctrl Pts',(0.,-0.100005667163201,-9.50018748080672));
#42402=CARTESIAN_POINT('Ctrl Pts',(1.5,-0.100005667163201,-9.50018748080672));
#42403=CARTESIAN_POINT('Ctrl Pts',(0.,0.0646995289261013,-9.5004935277391));
#42404=CARTESIAN_POINT('Ctrl Pts',(1.5,0.0646995289261013,-9.5004935277391));
#42405=CARTESIAN_POINT('Ctrl Pts',(0.,0.229385280173316,-9.49794428744803));
#42406=CARTESIAN_POINT('Ctrl Pts',(1.5,0.229385280173316,-9.49794428744803));
#42407=CARTESIAN_POINT('Ctrl Pts',(0.,0.394002091768334,-9.49254052641434));
#42408=CARTESIAN_POINT('Ctrl Pts',(1.5,0.394002091768334,-9.49254052641434));
#42409=CARTESIAN_POINT('Ctrl Pts',(0.,0.558500489607537,-9.48428386870457));
#42410=CARTESIAN_POINT('Ctrl Pts',(1.5,0.558500489607537,-9.48428386870457));
#42411=CARTESIAN_POINT('Ctrl Pts',(0.,0.722831035168601,-9.47317679547622));
#42412=CARTESIAN_POINT('Ctrl Pts',(1.5,0.722831035168601,-9.47317679547622));
#42413=CARTESIAN_POINT('Ctrl Pts',(0.,0.886944340387529,-9.45922264453641));
#42414=CARTESIAN_POINT('Ctrl Pts',(1.5,0.886944340387529,-9.45922264453641));
#42415=CARTESIAN_POINT('Ctrl Pts',(0.,1.05079108253884,-9.4424256099541));
#42416=CARTESIAN_POINT('Ctrl Pts',(1.5,1.05079108253884,-9.4424256099541));
#42417=CARTESIAN_POINT('Ctrl Pts',(0.,1.21432201899996,-9.42279074019445));
#42418=CARTESIAN_POINT('Ctrl Pts',(1.5,1.21432201899996,-9.42279074019445));
#42419=CARTESIAN_POINT('Ctrl Pts',(0.,1.3774880020205,-9.40032393630669));
#42420=CARTESIAN_POINT('Ctrl Pts',(1.5,1.3774880020205,-9.40032393630669));
#42421=CARTESIAN_POINT('Ctrl Pts',(0.,1.54023999349757,-9.37503195016512));
#42422=CARTESIAN_POINT('Ctrl Pts',(1.5,1.54023999349757,-9.37503195016512));
#42423=CARTESIAN_POINT('Ctrl Pts',(0.,1.70252907975783,-9.34692238276336));
#42424=CARTESIAN_POINT('Ctrl Pts',(1.5,1.70252907975783,-9.34692238276336));
#42425=CARTESIAN_POINT('Ctrl Pts',(0.,1.86430648634745,-9.31600368256141));
#42426=CARTESIAN_POINT('Ctrl Pts',(1.5,1.86430648634745,-9.31600368256141));
#42427=CARTESIAN_POINT('Ctrl Pts',(0.,2.02552359258146,-9.28228514229854));
#42428=CARTESIAN_POINT('Ctrl Pts',(1.5,2.02552359258146,-9.28228514229854));
#42429=CARTESIAN_POINT('Ctrl Pts',(0.,2.18613194610285,-9.24577689585861));
#42430=CARTESIAN_POINT('Ctrl Pts',(1.5,2.18613194610285,-9.24577689585861));
#42431=CARTESIAN_POINT('Ctrl Pts',(0.,2.34608327745199,-9.20648991518806));
#42432=CARTESIAN_POINT('Ctrl Pts',(1.5,2.34608327745199,-9.20648991518806));
#42433=CARTESIAN_POINT('Ctrl Pts',(0.,2.50532951464769,-9.16443600726627));
#42434=CARTESIAN_POINT('Ctrl Pts',(1.5,2.50532951464769,-9.16443600726627));
#42435=CARTESIAN_POINT('Ctrl Pts',(0.,2.66382279778037,-9.11962781112798));
#42436=CARTESIAN_POINT('Ctrl Pts',(1.5,2.66382279778037,-9.11962781112798));
#42437=CARTESIAN_POINT('Ctrl Pts',(0.,2.82151549322629,-9.07207879354574));
#42438=CARTESIAN_POINT('Ctrl Pts',(1.5,2.82151549322629,-9.07207879354574));
#42439=CARTESIAN_POINT('Ctrl Pts',(0.,2.97836020787586,-9.02180324476405));
#42440=CARTESIAN_POINT('Ctrl Pts',(1.5,2.97836020787586,-9.02180324476405));
#42441=CARTESIAN_POINT('Ctrl Pts',(0.,3.13430980337695,-8.96881627428497));
#42442=CARTESIAN_POINT('Ctrl Pts',(1.5,3.13430980337695,-8.96881627428497));
#42443=CARTESIAN_POINT('Ctrl Pts',(0.,3.2893174103942,-8.9131338067048));
#42444=CARTESIAN_POINT('Ctrl Pts',(1.5,3.2893174103942,-8.9131338067048));
#42445=CARTESIAN_POINT('Ctrl Pts',(0.,3.44333644288495,-8.85477257760172));
#42446=CARTESIAN_POINT('Ctrl Pts',(1.5,3.44333644288495,-8.85477257760172));
#42447=CARTESIAN_POINT('Ctrl Pts',(0.,3.59632061189727,-8.79375012773123));
#42448=CARTESIAN_POINT('Ctrl Pts',(1.5,3.59632061189727,-8.79375012773123));
#42449=CARTESIAN_POINT('Ctrl Pts',(0.,3.74822393938631,-8.73008479727211));
#42450=CARTESIAN_POINT('Ctrl Pts',(1.5,3.74822393938631,-8.73008479727211));
#42451=CARTESIAN_POINT('Ctrl Pts',(0.,3.89900077205013,-8.6637957201221));
#42452=CARTESIAN_POINT('Ctrl Pts',(1.5,3.89900077205013,-8.6637957201221));
#42453=CARTESIAN_POINT('Ctrl Pts',(0.,4.04860579518584,-8.59490281824332));
#42454=CARTESIAN_POINT('Ctrl Pts',(1.5,4.04860579518584,-8.59490281824332));
#42455=CARTESIAN_POINT('Ctrl Pts',(0.,4.19699404656678,-8.52342679605681));
#42456=CARTESIAN_POINT('Ctrl Pts',(1.5,4.19699404656678,-8.52342679605681));
#42457=CARTESIAN_POINT('Ctrl Pts',(0.,4.34412092966095,-8.4493891340983));
#42458=CARTESIAN_POINT('Ctrl Pts',(1.5,4.34412092966095,-8.4493891340983));
#42459=CARTESIAN_POINT('Ctrl Pts',(0.,4.48994222687229,-8.37281208272251));
#42460=CARTESIAN_POINT('Ctrl Pts',(1.5,4.48994222687229,-8.37281208272251));
#42461=CARTESIAN_POINT('Ctrl Pts',(0.,4.63441411280551,-8.29371865585542));
#42462=CARTESIAN_POINT('Ctrl Pts',(1.5,4.63441411280551,-8.29371865585542));
#42463=CARTESIAN_POINT('Ctrl Pts',(0.,4.77749316755556,-8.21213262479421));
#42464=CARTESIAN_POINT('Ctrl Pts',(1.5,4.77749316755556,-8.21213262479421));
#42465=CARTESIAN_POINT('Ctrl Pts',(0.,4.91913639002231,-8.12807851205451));
#42466=CARTESIAN_POINT('Ctrl Pts',(1.5,4.91913639002231,-8.12807851205451));
#42467=CARTESIAN_POINT('Ctrl Pts',(0.,5.05930121058847,-8.04158158243562));
#42468=CARTESIAN_POINT('Ctrl Pts',(1.5,5.05930121058847,-8.04158158243562));
#42469=CARTESIAN_POINT('Ctrl Pts',(0.,5.19794550382457,-7.95266783413212));
#42470=CARTESIAN_POINT('Ctrl Pts',(1.5,5.19794550382457,-7.95266783413212));
#42471=CARTESIAN_POINT('Ctrl Pts',(0.,5.33502760122154,-7.86136398989119));
#42472=CARTESIAN_POINT('Ctrl Pts',(1.5,5.33502760122154,-7.86136398989119));
#42473=CARTESIAN_POINT('Ctrl Pts',(0.,5.47050630395188,-7.7676974882153));
#42474=CARTESIAN_POINT('Ctrl Pts',(1.5,5.47050630395188,-7.7676974882153));
#42475=CARTESIAN_POINT('Ctrl Pts',(0.,5.60434089566018,-7.6716964746095));
#42476=CARTESIAN_POINT('Ctrl Pts',(1.5,5.60434089566018,-7.6716964746095));
#42477=CARTESIAN_POINT('Ctrl Pts',(0.,5.73649115418427,-7.57338979499691));
#42478=CARTESIAN_POINT('Ctrl Pts',(1.5,5.73649115418427,-7.57338979499691));
#42479=CARTESIAN_POINT('Ctrl Pts',(0.,5.86691736330717,-7.47280698917772));
#42480=CARTESIAN_POINT('Ctrl Pts',(1.5,5.86691736330717,-7.47280698917772));
#42481=CARTESIAN_POINT('Ctrl Pts',(0.,5.99558032454076,-7.36997828433179));
#42482=CARTESIAN_POINT('Ctrl Pts',(1.5,5.99558032454076,-7.36997828433179));
#42483=CARTESIAN_POINT('Ctrl Pts',(0.,6.1224413689417,-7.26493458856375));
#42484=CARTESIAN_POINT('Ctrl Pts',(1.5,6.1224413689417,-7.26493458856375));
#42485=CARTESIAN_POINT('Ctrl Pts',(0.,6.24746236896048,-7.15770748449079));
#42486=CARTESIAN_POINT('Ctrl Pts',(1.5,6.24746236896048,-7.15770748449079));
#42487=CARTESIAN_POINT('Ctrl Pts',(0.,6.3706057498637,-7.04832921373843));
#42488=CARTESIAN_POINT('Ctrl Pts',(1.5,6.3706057498637,-7.04832921373843));
#42489=CARTESIAN_POINT('Ctrl Pts',(0.,6.49183450119073,-6.93683266147738));
#42490=CARTESIAN_POINT('Ctrl Pts',(1.5,6.49183450119073,-6.93683266147738));
#42491=CARTESIAN_POINT('Ctrl Pts',(0.,6.61111218824578,-6.82325134100072));
#42492=CARTESIAN_POINT('Ctrl Pts',(1.5,6.61111218824578,-6.82325134100072));
#42493=CARTESIAN_POINT('Ctrl Pts',(0.,6.72840296362575,-6.70761937834039));
#42494=CARTESIAN_POINT('Ctrl Pts',(1.5,6.72840296362575,-6.70761937834039));
#42495=CARTESIAN_POINT('Ctrl Pts',(0.,6.84367157878482,-6.58997149692243));
#42496=CARTESIAN_POINT('Ctrl Pts',(1.5,6.84367157878482,-6.58997149692243));
#42497=CARTESIAN_POINT('Ctrl Pts',(0.,6.95688339333968,-6.47034301954872));
#42498=CARTESIAN_POINT('Ctrl Pts',(1.5,6.95688339333968,-6.47034301954872));
#42499=CARTESIAN_POINT('Ctrl Pts',(0.,7.06800438441262,-6.34876987041636));
#42500=CARTESIAN_POINT('Ctrl Pts',(1.5,7.06800438441262,-6.34876987041636));
#42501=CARTESIAN_POINT('Ctrl Pts',(0.,7.17700115601334,-6.22528857717452));
#42502=CARTESIAN_POINT('Ctrl Pts',(1.5,7.17700115601334,-6.22528857717452));
#42503=CARTESIAN_POINT('Ctrl Pts',(0.,7.28384094845988,-6.09993627301844));
#42504=CARTESIAN_POINT('Ctrl Pts',(1.5,7.28384094845988,-6.09993627301844));
#42505=CARTESIAN_POINT('Ctrl Pts',(0.,7.38849164783933,-5.97275069882039));
#42506=CARTESIAN_POINT('Ctrl Pts',(1.5,7.38849164783933,-5.97275069882039));
#42507=CARTESIAN_POINT('Ctrl Pts',(0.,7.49092179714954,-5.84377016152519));
#42508=CARTESIAN_POINT('Ctrl Pts',(1.5,7.49092179714954,-5.84377016152519));
#42509=CARTESIAN_POINT('Ctrl Pts',(0.,7.59110060748179,-5.71303349258081));
#42510=CARTESIAN_POINT('Ctrl Pts',(1.5,7.59110060748179,-5.71303349258081));
#42511=CARTESIAN_POINT('Ctrl Pts',(0.,7.68899796924518,-5.58058000640184));
#42512=CARTESIAN_POINT('Ctrl Pts',(1.5,7.68899796924518,-5.58058000640184));
#42513=CARTESIAN_POINT('Ctrl Pts',(0.,7.78458446343338,-5.44644945886454));
#42514=CARTESIAN_POINT('Ctrl Pts',(1.5,7.78458446343338,-5.44644945886454));
#42515=CARTESIAN_POINT('Ctrl Pts',(0.,7.87783137293427,-5.31068200583085));
#42516=CARTESIAN_POINT('Ctrl Pts',(1.5,7.87783137293427,-5.31068200583085));
#42517=CARTESIAN_POINT('Ctrl Pts',(0.,7.96871068608008,-5.17331826007796));
#42518=CARTESIAN_POINT('Ctrl Pts',(1.5,7.96871068608008,-5.17331826007796));
#42519=CARTESIAN_POINT('Ctrl Pts',(0.,8.05719510024161,-5.03439934825706));
#42520=CARTESIAN_POINT('Ctrl Pts',(1.5,8.05719510024161,-5.03439934825706));
#42521=CARTESIAN_POINT('Ctrl Pts',(0.,8.14325802546676,-4.89396696788343));
#42522=CARTESIAN_POINT('Ctrl Pts',(1.5,8.14325802546676,-4.89396696788343));
#42523=CARTESIAN_POINT('Ctrl Pts',(0.,8.22687358816365,-4.75206344435944));
#42524=CARTESIAN_POINT('Ctrl Pts',(1.5,8.22687358816365,-4.75206344435944));
#42525=CARTESIAN_POINT('Ctrl Pts',(0.,8.30801663482882,-4.60873178803278));
#42526=CARTESIAN_POINT('Ctrl Pts',(1.5,8.30801663482882,-4.60873178803278));
#42527=CARTESIAN_POINT('Ctrl Pts',(0.,8.38666274968152,-4.46401551988012));
#42528=CARTESIAN_POINT('Ctrl Pts',(1.5,8.38666274968152,-4.46401551988012));
#42529=CARTESIAN_POINT('Ctrl Pts',(0.,8.46278827234415,-4.31795849722095));
#42530=CARTESIAN_POINT('Ctrl Pts',(1.5,8.46278827234415,-4.31795849722095));
#42531=CARTESIAN_POINT('Ctrl Pts',(0.,8.53637031556984,-4.17060473945423));
#42532=CARTESIAN_POINT('Ctrl Pts',(1.5,8.53637031556984,-4.17060473945423));
#42533=CARTESIAN_POINT('Ctrl Pts',(0.,8.60738678301777,-4.02199825381128));
#42534=CARTESIAN_POINT('Ctrl Pts',(1.5,8.60738678301777,-4.02199825381128));
#42535=CARTESIAN_POINT('Ctrl Pts',(0.,8.67581638707736,-3.87218286111754));
#42536=CARTESIAN_POINT('Ctrl Pts',(1.5,8.67581638707736,-3.87218286111754));
#42537=CARTESIAN_POINT('Ctrl Pts',(0.,8.74163863005112,-3.7212025564437));
#42538=CARTESIAN_POINT('Ctrl Pts',(1.5,8.74163863005112,-3.7212025564437));
#42539=CARTESIAN_POINT('Ctrl Pts',(0.,8.8048337853866,-3.569101869772));
#42540=CARTESIAN_POINT('Ctrl Pts',(1.5,8.8048337853866,-3.569101869772));
#42541=CARTESIAN_POINT('Ctrl Pts',(0.,8.86538287895677,-3.41592622669153));
#42542=CARTESIAN_POINT('Ctrl Pts',(1.5,8.86538287895677,-3.41592622669153));
#42543=CARTESIAN_POINT('Ctrl Pts',(0.,8.92326767038829,-3.26172230913547));
#42544=CARTESIAN_POINT('Ctrl Pts',(1.5,8.92326767038829,-3.26172230913547));
#42545=CARTESIAN_POINT('Ctrl Pts',(0.,8.97847063443704,-3.10653841617418));
#42546=CARTESIAN_POINT('Ctrl Pts',(1.5,8.97847063443704,-3.10653841617418));
#42547=CARTESIAN_POINT('Ctrl Pts',(0.,9.03097502289857,-2.95042358103383));
#42548=CARTESIAN_POINT('Ctrl Pts',(1.5,9.03097502289857,-2.95042358103383));
#42549=CARTESIAN_POINT('Ctrl Pts',(0.,9.08076492656766,-2.79342668815082));
#42550=CARTESIAN_POINT('Ctrl Pts',(1.5,9.08076492656766,-2.79342668815082));
#42551=CARTESIAN_POINT('Ctrl Pts',(0.,9.12782533724964,-2.63559559022695));
#42552=CARTESIAN_POINT('Ctrl Pts',(1.5,9.12782533724964,-2.63559559022695));
#42553=CARTESIAN_POINT('Ctrl Pts',(0.,9.17214220982579,-2.47697622525295));
#42554=CARTESIAN_POINT('Ctrl Pts',(1.5,9.17214220982579,-2.47697622525295));
#42555=CARTESIAN_POINT('Ctrl Pts',(0.,9.21370252437545,-2.31761173346462));
#42556=CARTESIAN_POINT('Ctrl Pts',(1.5,9.21370252437545,-2.31761173346462));
#42557=CARTESIAN_POINT('Ctrl Pts',(0.,9.25249415711055,-2.15754444747782));
#42558=CARTESIAN_POINT('Ctrl Pts',(1.5,9.25249415711055,-2.15754444747782));
#42559=CARTESIAN_POINT('Ctrl Pts',(0.,9.28850575136439,-1.99681788239702));
#42560=CARTESIAN_POINT('Ctrl Pts',(1.5,9.28850575136439,-1.99681788239702));
#42561=CARTESIAN_POINT('Ctrl Pts',(0.,9.32172658862992,-1.8354787259745));
#42562=CARTESIAN_POINT('Ctrl Pts',(1.5,9.32172658862992,-1.8354787259745));
#42563=CARTESIAN_POINT('Ctrl Pts',(0.,9.35214645964288,-1.67357882889265));
#42564=CARTESIAN_POINT('Ctrl Pts',(1.5,9.35214645964288,-1.67357882889265));
#42565=CARTESIAN_POINT('Ctrl Pts',(0.,9.37975553550456,-1.51117719524876));
#42566=CARTESIAN_POINT('Ctrl Pts',(1.5,9.37975553550456,-1.51117719524876));
#42567=CARTESIAN_POINT('Ctrl Pts',(0.,9.40454466499353,-1.34833562021881));
#42568=CARTESIAN_POINT('Ctrl Pts',(1.5,9.40454466499353,-1.34833562021881));
#42569=CARTESIAN_POINT('Ctrl Pts',(0.,9.42650567192347,-1.18511432783383));
#42570=CARTESIAN_POINT('Ctrl Pts',(1.5,9.42650567192347,-1.18511432783383));
#42571=CARTESIAN_POINT('Ctrl Pts',(0.,9.44563165255895,-1.02156760869846));
#42572=CARTESIAN_POINT('Ctrl Pts',(1.5,9.44563165255895,-1.02156760869846));
#42573=CARTESIAN_POINT('Ctrl Pts',(0.,9.46191727309995,-0.857739457490668));
#42574=CARTESIAN_POINT('Ctrl Pts',(1.5,9.46191727309995,-0.857739457490668));
#42575=CARTESIAN_POINT('Ctrl Pts',(0.,9.475359067247,-0.69365921007208));
#42576=CARTESIAN_POINT('Ctrl Pts',(1.5,9.475359067247,-0.69365921007208));
#42577=CARTESIAN_POINT('Ctrl Pts',(0.,9.48595504112471,-0.529344474234685));
#42578=CARTESIAN_POINT('Ctrl Pts',(1.5,9.48595504112471,-0.529344474234685));
#42579=CARTESIAN_POINT('Ctrl Pts',(0.,9.49215443085059,-0.397712142849856));
#42580=CARTESIAN_POINT('Ctrl Pts',(1.5,9.49215443085059,-0.397712142849856));
#42581=CARTESIAN_POINT('Ctrl Pts',(0.,9.49552283633695,-0.298887663039026));
#42582=CARTESIAN_POINT('Ctrl Pts',(1.5,9.49552283633695,-0.298887663039026));
#42583=CARTESIAN_POINT('Ctrl Pts',(0.,9.49719905300845,-0.232960129825712));
#42584=CARTESIAN_POINT('Ctrl Pts',(1.5,9.49719905300845,-0.232960129825712));
#42585=CARTESIAN_POINT('Ctrl Pts',(0.,9.49789481459768,-0.19998522655085));
#42586=CARTESIAN_POINT('Ctrl Pts',(1.5,9.49789481459768,-0.19998522655085));
#42587=CARTESIAN_POINT('',(0.15,9.49789481459768,0.19998522655078));
#42588=CARTESIAN_POINT('',(0.,9.49789481459768,0.199985226550847));
#42589=CARTESIAN_POINT('Ctrl Pts',(0.15,9.49789467324318,-0.199991925789801));
#42590=CARTESIAN_POINT('Ctrl Pts',(0.15,9.46807533126202,-1.61320182906088));
#42591=CARTESIAN_POINT('Ctrl Pts',(0.15,8.76936042330201,-4.41924950926567));
#42592=CARTESIAN_POINT('Ctrl Pts',(0.15,6.00716218277886,-7.7702406804142));
#42593=CARTESIAN_POINT('Ctrl Pts',(0.15,2.06951231035037,-9.59921473442292));
#42594=CARTESIAN_POINT('Ctrl Pts',(0.15,-2.27052730117003,-9.55414177959014));
#42595=CARTESIAN_POINT('Ctrl Pts',(0.15,-6.16993267085606,-7.64037775456781));
#42596=CARTESIAN_POINT('Ctrl Pts',(0.15,-8.55868308240392,-4.61342308628249));
#42597=CARTESIAN_POINT('Ctrl Pts',(0.15,-9.81741474111766,-0.515781321759936));
#42598=CARTESIAN_POINT('Ctrl Pts',(0.15,-9.23735151866284,3.36699645272176));
#42599=CARTESIAN_POINT('Ctrl Pts',(0.15,-6.56839683600959,7.31525710391206));
#42600=CARTESIAN_POINT('Ctrl Pts',(0.15,-2.7590783122695,9.55398857169003));
#42601=CARTESIAN_POINT('Ctrl Pts',(0.15,2.07186156931854,9.59716037348304));
#42602=CARTESIAN_POINT('Ctrl Pts',(0.15,6.00595373869092,7.771189481248));
#42603=CARTESIAN_POINT('Ctrl Pts',(0.15,8.76999259869694,4.41871090089412));
#42604=CARTESIAN_POINT('Ctrl Pts',(0.15,9.46807646415204,1.61319520738852));
#42605=CARTESIAN_POINT('Ctrl Pts',(0.15,9.49789481459768,0.199985226550645));
#42606=CARTESIAN_POINT('Ctrl Pts',(0.15,9.49789481459768,0.199985226550645));
#42607=CARTESIAN_POINT('Ctrl Pts',(0.15,9.46807646415204,1.61319520738852));
#42608=CARTESIAN_POINT('Ctrl Pts',(0.15,8.76999259869694,4.41871090089412));
#42609=CARTESIAN_POINT('Ctrl Pts',(0.15,6.00595373869092,7.771189481248));
#42610=CARTESIAN_POINT('Ctrl Pts',(0.15,2.07186156931854,9.59716037348304));
#42611=CARTESIAN_POINT('Ctrl Pts',(0.15,-2.7590783122695,9.55398857169003));
#42612=CARTESIAN_POINT('Ctrl Pts',(0.15,-6.56839683600959,7.31525710391206));
#42613=CARTESIAN_POINT('Ctrl Pts',(0.15,-9.23735151866284,3.36699645272176));
#42614=CARTESIAN_POINT('Ctrl Pts',(0.15,-9.81741474111766,-0.515781321759936));
#42615=CARTESIAN_POINT('Ctrl Pts',(0.15,-8.55868308240392,-4.61342308628249));
#42616=CARTESIAN_POINT('Ctrl Pts',(0.15,-6.16993267085606,-7.64037775456781));
#42617=CARTESIAN_POINT('Ctrl Pts',(0.15,-2.27052730117003,-9.55414177959014));
#42618=CARTESIAN_POINT('Ctrl Pts',(0.15,2.06951231035037,-9.59921473442292));
#42619=CARTESIAN_POINT('Ctrl Pts',(0.15,6.00716218277886,-7.7702406804142));
#42620=CARTESIAN_POINT('Ctrl Pts',(0.15,8.76936042330201,-4.41924950926567));
#42621=CARTESIAN_POINT('Ctrl Pts',(0.15,9.46807533126202,-1.61320182906088));
#42622=CARTESIAN_POINT('Ctrl Pts',(0.15,9.49789467324318,-0.199991925789801));
#42623=CARTESIAN_POINT('Ctrl Pts',(0.1,9.44790594084898,0.198930474761433));
#42624=CARTESIAN_POINT('Ctrl Pts',(0.1,9.41824388733793,1.60473292350496));
#42625=CARTESIAN_POINT('Ctrl Pts',(0.1,8.72383591777496,4.39544649470378));
#42626=CARTESIAN_POINT('Ctrl Pts',(0.1,5.97434304623036,7.73029415185335));
#42627=CARTESIAN_POINT('Ctrl Pts',(0.1,2.06095722088225,9.54664763134213));
#42628=CARTESIAN_POINT('Ctrl Pts',(0.1,-2.74455695981483,9.50370569266413));
#42629=CARTESIAN_POINT('Ctrl Pts',(0.1,-6.53382629000873,7.2767554489634));
#42630=CARTESIAN_POINT('Ctrl Pts',(0.1,-9.18873390374524,3.34927559427278));
#42631=CARTESIAN_POINT('Ctrl Pts',(0.1,-9.76574412542408,-0.513066686274358));
#42632=CARTESIAN_POINT('Ctrl Pts',(0.1,-8.51363740045374,-4.58914207119684));
#42633=CARTESIAN_POINT('Ctrl Pts',(0.1,-6.1374592951313,-7.6001648172806));
#42634=CARTESIAN_POINT('Ctrl Pts',(0.1,-2.25857727887409,-9.5038582888179));
#42635=CARTESIAN_POINT('Ctrl Pts',(0.1,2.05862033931887,-9.54869104361738));
#42636=CARTESIAN_POINT('Ctrl Pts',(0.1,5.97554512181216,-7.72935044055577));
#42637=CARTESIAN_POINT('Ctrl Pts',(0.1,8.72320707333466,-4.39598222754933));
#42638=CARTESIAN_POINT('Ctrl Pts',(0.1,9.41824276040486,-1.60473950957998));
#42639=CARTESIAN_POINT('Ctrl Pts',(0.1,9.44790580023542,-0.198937138885166));
#42640=CARTESIAN_POINT('Ctrl Pts',(0.05,9.39791706710029,0.197875722972221));
#42641=CARTESIAN_POINT('Ctrl Pts',(0.05,9.36841131052381,1.5962706396214));
#42642=CARTESIAN_POINT('Ctrl Pts',(0.05,8.67767923685297,4.37218208851344));
#42643=CARTESIAN_POINT('Ctrl Pts',(0.05,5.9427323537698,7.6893988224587));
#42644=CARTESIAN_POINT('Ctrl Pts',(0.05,2.05005287244595,9.49613488920121));
#42645=CARTESIAN_POINT('Ctrl Pts',(0.05,-2.73003560736016,9.45342281363823));
#42646=CARTESIAN_POINT('Ctrl Pts',(0.05,-6.49925574400788,7.23825379401473));
#42647=CARTESIAN_POINT('Ctrl Pts',(0.05,-9.14011628882764,3.3315547358238));
#42648=CARTESIAN_POINT('Ctrl Pts',(0.05,-9.7140735097305,-0.51035205078877));
#42649=CARTESIAN_POINT('Ctrl Pts',(0.05,-8.46859171850355,-4.5648610561112));
#42650=CARTESIAN_POINT('Ctrl Pts',(0.05,-6.10498591940654,-7.55995187999338));
#42651=CARTESIAN_POINT('Ctrl Pts',(0.05,-2.24662725657814,-9.45357479804566));
#42652=CARTESIAN_POINT('Ctrl Pts',(0.05,2.04772836828738,-9.49816735281183));
#42653=CARTESIAN_POINT('Ctrl Pts',(0.05,5.94392806084546,-7.68846020069733));
#42654=CARTESIAN_POINT('Ctrl Pts',(0.05,8.67705372336733,-4.372714945833));
#42655=CARTESIAN_POINT('Ctrl Pts',(0.05,9.3684101895477,-1.59627719009908));
#42656=CARTESIAN_POINT('Ctrl Pts',(0.05,9.39791692722766,-0.197882351980531));
#42657=CARTESIAN_POINT('Ctrl Pts',(0.,9.34792819335159,0.196820971183008));
#42658=CARTESIAN_POINT('Ctrl Pts',(0.,9.3185787337097,1.58780835573784));
#42659=CARTESIAN_POINT('Ctrl Pts',(0.,8.63152255593099,4.34891768232309));
#42660=CARTESIAN_POINT('Ctrl Pts',(0.,5.91112166130923,7.64850349306405));
#42661=CARTESIAN_POINT('Ctrl Pts',(0.,2.03914852400966,9.4456221470603));
#42662=CARTESIAN_POINT('Ctrl Pts',(0.,-2.71551425490549,9.40313993461232));
#42663=CARTESIAN_POINT('Ctrl Pts',(0.,-6.46468519800702,7.19975213906607));
#42664=CARTESIAN_POINT('Ctrl Pts',(0.,-9.09149867391003,3.31383387737481));
#42665=CARTESIAN_POINT('Ctrl Pts',(0.,-9.66240289403692,-0.50763741530319));
#42666=CARTESIAN_POINT('Ctrl Pts',(0.,-8.42354603655337,-4.54058004102555));
#42667=CARTESIAN_POINT('Ctrl Pts',(0.,-6.07251254368177,-7.51973894270617));
#42668=CARTESIAN_POINT('Ctrl Pts',(0.,-2.2346772342822,-9.40329130727341));
#42669=CARTESIAN_POINT('Ctrl Pts',(0.,2.03683639725588,-9.44764366200629));
#42670=CARTESIAN_POINT('Ctrl Pts',(0.,5.91231099987876,-7.64756996083891));
#42671=CARTESIAN_POINT('Ctrl Pts',(0.,8.63090037339999,-4.34944766411667));
#42672=CARTESIAN_POINT('Ctrl Pts',(0.,9.31857761869054,-1.58781487061818));
#42673=CARTESIAN_POINT('Ctrl Pts',(0.,9.3479280542199,-0.196827565075896));
#42674=CARTESIAN_POINT('',(0.,9.34792805421991,0.196827565075895));
#42675=CARTESIAN_POINT('Ctrl Pts',(0.15,9.49789481459768,0.199985226550846));
#42676=CARTESIAN_POINT('Ctrl Pts',(0.1,9.44790594084898,0.198930474761633));
#42677=CARTESIAN_POINT('Ctrl Pts',(0.05,9.39791706710028,0.19787572297242));
#42678=CARTESIAN_POINT('Ctrl Pts',(0.,9.34792819335158,0.196820971183207));
#42679=CARTESIAN_POINT('Ctrl Pts',(0.,9.34792805421987,0.196827565076008));
#42680=CARTESIAN_POINT('Ctrl Pts',(0.,9.31857764805933,1.58781271869574));
#42681=CARTESIAN_POINT('Ctrl Pts',(0.,8.63152112305334,4.34891942026648));
#42682=CARTESIAN_POINT('Ctrl Pts',(0.,5.91112166130923,7.64850349306405));
#42683=CARTESIAN_POINT('Ctrl Pts',(0.,2.03914852400966,9.4456221470603));
#42684=CARTESIAN_POINT('Ctrl Pts',(0.,-2.71551425490549,9.40313993461232));
#42685=CARTESIAN_POINT('Ctrl Pts',(0.,-6.46468519800702,7.19975213906607));
#42686=CARTESIAN_POINT('Ctrl Pts',(0.,-9.09149867391003,3.31383387737481));
#42687=CARTESIAN_POINT('Ctrl Pts',(0.,-9.66240289403692,-0.50763741530319));
#42688=CARTESIAN_POINT('Ctrl Pts',(0.,-8.42354603655337,-4.54058004102555));
#42689=CARTESIAN_POINT('Ctrl Pts',(0.,-6.07251254368177,-7.51973894270617));
#42690=CARTESIAN_POINT('Ctrl Pts',(0.,-2.2346772342822,-9.40329130727341));
#42691=CARTESIAN_POINT('Ctrl Pts',(0.,2.03683639725588,-9.44764366200629));
#42692=CARTESIAN_POINT('Ctrl Pts',(0.,5.91231099987876,-7.64756996083891));
#42693=CARTESIAN_POINT('Ctrl Pts',(0.,8.63090037339999,-4.34944766411667));
#42694=CARTESIAN_POINT('Ctrl Pts',(0.,9.31857761869054,-1.58781487061818));
#42695=CARTESIAN_POINT('Ctrl Pts',(0.,9.3479280542199,-0.196827565075896));
#42696=CARTESIAN_POINT('Ctrl Pts',(1.5,8.14819397266823,-0.171566273307202));
#42697=CARTESIAN_POINT('Ctrl Pts',(1.5,8.13256980638789,-0.912057527264844));
#42698=CARTESIAN_POINT('Ctrl Pts',(1.5,7.82167697943358,-2.8606390589131));
#42699=CARTESIAN_POINT('Ctrl Pts',(1.5,6.2437277562345,-5.63228319243984));
#42700=CARTESIAN_POINT('Ctrl Pts',(1.5,3.27411598702021,-7.75142033677142));
#42701=CARTESIAN_POINT('Ctrl Pts',(1.5,-0.306947971306406,-8.40596108242038));
#42702=CARTESIAN_POINT('Ctrl Pts',(1.5,-3.83187577666327,-7.49038443259283));
#42703=CARTESIAN_POINT('Ctrl Pts',(1.5,-6.63683129723738,-5.16900547712466));
#42704=CARTESIAN_POINT('Ctrl Pts',(1.5,-8.34751515590091,-1.57539769915707));
#42705=CARTESIAN_POINT('Ctrl Pts',(1.5,-8.11584947195258,2.79986176826081));
#42706=CARTESIAN_POINT('Ctrl Pts',(1.5,-5.40342015315134,6.67067944450257));
#42707=CARTESIAN_POINT('Ctrl Pts',(1.5,-1.05510724703267,8.51840124378108));
#42708=CARTESIAN_POINT('Ctrl Pts',(1.5,3.61325431606088,7.78925162987645));
#42709=CARTESIAN_POINT('Ctrl Pts',(1.5,7.18672995402067,4.69400338747101));
#42710=CARTESIAN_POINT('Ctrl Pts',(1.5,8.11619629477138,1.68806323182392));
#42711=CARTESIAN_POINT('Ctrl Pts',(1.5,8.14819383353886,0.171572867200535));
#42712=CARTESIAN_POINT('Ctrl Pts',(1.49821428571429,8.14640865574864,-0.171528603600415));
#42713=CARTESIAN_POINT('Ctrl Pts',(1.49821428571429,8.13078803910471,-0.911854951429866));
#42714=CARTESIAN_POINT('Ctrl Pts',(1.49821428571429,7.81996304417322,-2.86001277316043));
#42715=CARTESIAN_POINT('Ctrl Pts',(1.49821428571429,6.24235987703551,-5.63104745342254));
#42716=CARTESIAN_POINT('Ctrl Pts',(1.49821428571429,3.27339861384903,-7.74972230254187));
#42717=CARTESIAN_POINT('Ctrl Pts',(1.49821428571429,-0.306880734144998,
-8.4041189576045));
#42718=CARTESIAN_POINT('Ctrl Pts',(1.49821428571429,-3.83103616047986,-7.48874329992843));
#42719=CARTESIAN_POINT('Ctrl Pts',(1.49821428571429,-6.63537718766757,-5.16787287967044));
#42720=CARTESIAN_POINT('Ctrl Pts',(1.49821428571429,-8.34568614737968,-1.5750525297584));
#42721=CARTESIAN_POINT('Ctrl Pts',(1.49821428571429,-8.1140712179393,2.79924829077486));
#42722=CARTESIAN_POINT('Ctrl Pts',(1.49821428571429,-5.40223627158938,6.66921785365957));
#42723=CARTESIAN_POINT('Ctrl Pts',(1.49821428571429,-1.05487600617258,8.51653458003634));
#42724=CARTESIAN_POINT('Ctrl Pts',(1.49821428571429,3.61246244976634,7.78754536608789));
#42725=CARTESIAN_POINT('Ctrl Pts',(1.49821428571429,7.18515561436926,4.69297470505487));
#42726=CARTESIAN_POINT('Ctrl Pts',(1.49821428571429,8.11441723405578,1.68769381933928));
#42727=CARTESIAN_POINT('Ctrl Pts',(1.49821428571429,8.14640851661926,0.171535197493771));
#42728=CARTESIAN_POINT('Ctrl Pts',(1.49464285714286,8.14283802190945,-0.171453264186841));
#42729=CARTESIAN_POINT('Ctrl Pts',(1.49464285714286,8.12721912363431,-0.911699781432996));
#42730=CARTESIAN_POINT('Ctrl Pts',(1.49464285714286,7.81653656299143,-2.85870506455113));
#42731=CARTESIAN_POINT('Ctrl Pts',(1.49464285714286,6.23962066743289,-5.6287311498091));
#42732=CARTESIAN_POINT('Ctrl Pts',(1.49464285714286,3.27196431819506,-7.74630401160597));
#42733=CARTESIAN_POINT('Ctrl Pts',(1.49464285714286,-0.306746719965775,
-8.4004583023455));
#42734=CARTESIAN_POINT('Ctrl Pts',(1.49464285714286,-3.8293568117723,-7.48545336015222));
#42735=CARTESIAN_POINT('Ctrl Pts',(1.49464285714286,-6.63246897130202,-5.16561221049837));
#42736=CARTESIAN_POINT('Ctrl Pts',(1.49464285714286,-8.34202811752249,-1.57436032443796));
#42737=CARTESIAN_POINT('Ctrl Pts',(1.49464285714286,-8.11051476861003,2.7980202100795));
#42738=CARTESIAN_POINT('Ctrl Pts',(1.49464285714286,-5.39986843519062,6.66629520618857));
#42739=CARTESIAN_POINT('Ctrl Pts',(1.49464285714286,-1.05441362653318,8.51280133885302));
#42740=CARTESIAN_POINT('Ctrl Pts',(1.49464285714286,3.61087899851321,7.7841326114491));
#42741=CARTESIAN_POINT('Ctrl Pts',(1.49464285714286,7.18200640929766,4.69091743340625));
#42742=CARTESIAN_POINT('Ctrl Pts',(1.49464285714286,8.11086021393872,1.68695621374015));
#42743=CARTESIAN_POINT('Ctrl Pts',(1.49464285714286,8.14283788278007,0.171459858080241));
#42744=CARTESIAN_POINT('Ctrl Pts',(1.48928571428572,8.13748207115066,-0.17134025506648));
#42745=CARTESIAN_POINT('Ctrl Pts',(1.48928571428572,8.12186650547007,-0.911431949339478));
#42746=CARTESIAN_POINT('Ctrl Pts',(1.48928571428571,7.81139664626853,-2.85675123840278));
#42747=CARTESIAN_POINT('Ctrl Pts',(1.48928571428572,6.23551233729744,-5.6252349205191));
#42748=CARTESIAN_POINT('Ctrl Pts',(1.48928571428571,3.26981281147411,-7.74117969343071));
#42749=CARTESIAN_POINT('Ctrl Pts',(1.48928571428572,-0.306545634130199,
-8.39496400872577));
#42750=CARTESIAN_POINT('Ctrl Pts',(1.48928571428571,-3.82683780503573,-7.48051952735625));
#42751=CARTESIAN_POINT('Ctrl Pts',(1.48928571428572,-6.62810664636446,-5.16222057169492));
#42752=CARTESIAN_POINT('Ctrl Pts',(1.48928571428571,-8.33654107453486,-1.57332227836535));
#42753=CARTESIAN_POINT('Ctrl Pts',(1.48928571428572,-8.1051800863798,2.79617824699648));
#42754=CARTESIAN_POINT('Ctrl Pts',(1.48928571428571,-5.39631669087431,6.66191116002174));
#42755=CARTESIAN_POINT('Ctrl Pts',(1.48928571428572,-1.05372004275023,8.50720146496768));
#42756=CARTESIAN_POINT('Ctrl Pts',(1.48928571428571,3.60850378215682,7.77901351135191));
#42757=CARTESIAN_POINT('Ctrl Pts',(1.48928571428572,7.17728267546545,4.68783151285791));
#42758=CARTESIAN_POINT('Ctrl Pts',(1.48928571428572,8.10552452922819,1.68584963424105));
#42759=CARTESIAN_POINT('Ctrl Pts',(1.48928571428572,8.13748193202128,0.171346848959947));
#42760=CARTESIAN_POINT('Ctrl Pts',(1.48392857142857,8.13212612039187,-0.171227245946119));
#42761=CARTESIAN_POINT('Ctrl Pts',(1.48392857142857,8.11651949934755,-0.910903397565355));
#42762=CARTESIAN_POINT('Ctrl Pts',(1.48392857142857,7.80625528052739,-2.85485491778256));
#42763=CARTESIAN_POINT('Ctrl Pts',(1.48392857142857,6.23140760661372,-5.62157685126289));
#42764=CARTESIAN_POINT('Ctrl Pts',(1.48392857142857,3.26766083470535,-7.73607855230273));
#42765=CARTESIAN_POINT('Ctrl Pts',(1.48392857142857,-0.30634406838548,-8.38944510723279));
#42766=CARTESIAN_POINT('Ctrl Pts',(1.48392857142857,-3.82431891963735,-7.47559369866491));
#42767=CARTESIAN_POINT('Ctrl Pts',(1.48392857142857,-6.62374431853364,-5.15882421275128));
#42768=CARTESIAN_POINT('Ctrl Pts',(1.48392857142857,-8.33105404491241,-1.57228617899269));
#42769=CARTESIAN_POINT('Ctrl Pts',(1.48392857142857,-8.09984534293092,2.79433745799257));
#42770=CARTESIAN_POINT('Ctrl Pts',(1.48392857142857,-5.39276502298037,6.65752655669259));
#42771=CARTESIAN_POINT('Ctrl Pts',(1.48392857142857,-1.05302635250161,8.50160150106888));
#42772=CARTESIAN_POINT('Ctrl Pts',(1.48392857142857,3.60612827237966,7.77389464806985));
#42773=CARTESIAN_POINT('Ctrl Pts',(1.48392857142857,7.17255948998649,4.68474549512318));
#42774=CARTESIAN_POINT('Ctrl Pts',(1.48392857142857,8.10018769589636,1.68474178299355));
#42775=CARTESIAN_POINT('Ctrl Pts',(1.48392857142857,8.13212598126249,0.171233839839652));
#42776=CARTESIAN_POINT('Ctrl Pts',(1.47321428571429,8.1214142188743,-0.171001227705398));
#42777=CARTESIAN_POINT('Ctrl Pts',(1.47321428571429,8.1058110766084,-0.910515765059556));
#42778=CARTESIAN_POINT('Ctrl Pts',(1.47321428571429,7.79597626980663,-2.85091461493954));
#42779=CARTESIAN_POINT('Ctrl Pts',(1.47321428571429,6.22318890264251,-5.61467628234092));
#42780=CARTESIAN_POINT('Ctrl Pts',(1.47321428571429,3.26335808814766,-7.72581675646512));
#42781=CARTESIAN_POINT('Ctrl Pts',(1.47321428571429,-0.305942169197622,
-8.37847049187623));
#42782=CARTESIAN_POINT('Ctrl Pts',(1.47321428571429,-3.81928083727071,-7.4657214884944));
#42783=CARTESIAN_POINT('Ctrl Pts',(1.47321428571429,-6.61501967030123,-5.15204361515029));
#42784=CARTESIAN_POINT('Ctrl Pts',(1.47321428571429,-8.32007995134863,-1.57020898154823));
#42785=CARTESIAN_POINT('Ctrl Pts',(1.47321428571429,-8.08917601322925,2.79065286520672));
#42786=CARTESIAN_POINT('Ctrl Pts',(1.47321428571429,-5.38566149095657,6.64875878070508));
#42787=CARTESIAN_POINT('Ctrl Pts',(1.47321428571429,-1.05163924538491,8.49040180440612));
#42788=CARTESIAN_POINT('Ctrl Pts',(1.47321428571429,3.60137800626563,7.76365631341634));
#42789=CARTESIAN_POINT('Ctrl Pts',(1.47321428571429,7.16311171097749,4.67857370920709));
#42790=CARTESIAN_POINT('Ctrl Pts',(1.47321428571429,8.08951697864065,1.68252934606993));
#42791=CARTESIAN_POINT('Ctrl Pts',(1.47321428571429,8.12141407974491,0.171007821599063));
#42792=CARTESIAN_POINT('Ctrl Pts',(1.42857142857143,8.07678129588441,-0.170059485035724));
#42793=CARTESIAN_POINT('Ctrl Pts',(1.42857142857143,8.06123667672408,-0.906855203438805));
#42794=CARTESIAN_POINT('Ctrl Pts',(1.42857142857143,7.75313569047582,-2.83494783500331));
#42795=CARTESIAN_POINT('Ctrl Pts',(1.42857142857143,6.18897254156974,-5.58465422746104));
#42796=CARTESIAN_POINT('Ctrl Pts',(1.42857142857143,3.24542628982086,-7.68324110488138));
#42797=CARTESIAN_POINT('Ctrl Pts',(1.42857142857143,-0.304263824213199,
-8.33254987154725));
#42798=CARTESIAN_POINT('Ctrl Pts',(1.42857142857143,-3.7982897793451,-7.42465007411634));
#42799=CARTESIAN_POINT('Ctrl Pts',(1.42857142857143,-6.57866694663448,-5.12375409419289));
#42800=CARTESIAN_POINT('Ctrl Pts',(1.42857142857143,-8.27435466635361,-1.56156926465683));
#42801=CARTESIAN_POINT('Ctrl Pts',(1.42857142857143,-8.04471999252646,2.77530960627787));
#42802=CARTESIAN_POINT('Ctrl Pts',(1.42857142857143,-5.3560640404145,6.61222200964727));
#42803=CARTESIAN_POINT('Ctrl Pts',(1.42857142857143,-1.04585879714263,8.44373569546135));
#42804=CARTESIAN_POINT('Ctrl Pts',(1.42857142857143,3.58158292881416,7.72099844358104));
#42805=CARTESIAN_POINT('Ctrl Pts',(1.42857142857143,7.12375026710686,4.65285717209956));
#42806=CARTESIAN_POINT('Ctrl Pts',(1.42857142857143,8.04504664545411,1.67330088163032));
#42807=CARTESIAN_POINT('Ctrl Pts',(1.42857142857143,8.07678115675501,0.170066078929943));
#42808=CARTESIAN_POINT('Ctrl Pts',(1.38571428571429,8.03393368981411,-0.169155412072838));
#42809=CARTESIAN_POINT('Ctrl Pts',(1.38571428571429,8.0182385308055,-0.912944788594306));
#42810=CARTESIAN_POINT('Ctrl Pts',(1.38571428571429,7.71206210954355,-2.81750148479799));
#42811=CARTESIAN_POINT('Ctrl Pts',(1.38571428571429,6.15599224754923,-5.56179450124059));
#42812=CARTESIAN_POINT('Ctrl Pts',(1.38571428571429,3.22822907784503,-7.64151474261234));
#42813=CARTESIAN_POINT('Ctrl Pts',(1.38571428571429,-0.302670290692921,
-8.28937251788484));
#42814=CARTESIAN_POINT('Ctrl Pts',(1.38571428571429,-3.77813389419134,-7.38492668159209));
#42815=CARTESIAN_POINT('Ctrl Pts',(1.38571428571429,-6.5437684384882,-5.09677002251735));
#42816=CARTESIAN_POINT('Ctrl Pts',(1.38571428571429,-8.23045790044569,-1.55320342889092));
#42817=CARTESIAN_POINT('Ctrl Pts',(1.38571428571429,-8.00204446766765,2.76053682998459));
#42818=CARTESIAN_POINT('Ctrl Pts',(1.38571428571429,-5.32764767284217,6.5771672327508));
#42819=CARTESIAN_POINT('Ctrl Pts',(1.38571428571429,-1.04031348854024,8.39893954655973));
#42820=CARTESIAN_POINT('Ctrl Pts',(1.38571428571429,3.56259046274421,7.68003816534915));
#42821=CARTESIAN_POINT('Ctrl Pts',(1.38571428571429,7.08594308215698,4.62817287637971));
#42822=CARTESIAN_POINT('Ctrl Pts',(1.38571428571429,8.00239743556643,1.66448840118123));
#42823=CARTESIAN_POINT('Ctrl Pts',(1.38571428571429,8.0339335506847,0.169162005967588));
#42824=CARTESIAN_POINT('Ctrl Pts',(1.35,7.99822735142219,-0.168402017937099));
#42825=CARTESIAN_POINT('Ctrl Pts',(1.35,7.98260318514185,-0.908893271894742));
#42826=CARTESIAN_POINT('Ctrl Pts',(1.35,7.67778340433625,-2.80497576974459));
#42827=CARTESIAN_POINT('Ctrl Pts',(1.35,6.12863466356929,-5.53707972089446));
#42828=CARTESIAN_POINT('Ctrl Pts',(1.35,3.21388161442135,-7.60755405802142));
#42829=CARTESIAN_POINT('Ctrl Pts',(1.35,-0.301325547464756,-8.25253002156739));
#42830=CARTESIAN_POINT('Ctrl Pts',(1.35,-3.76134157052312,-7.35210402830392));
#42831=CARTESIAN_POINT('Ctrl Pts',(1.35,-6.51468624709197,-5.07411807343295));
#42832=CARTESIAN_POINT('Ctrl Pts',(1.35,-8.19387773002112,-1.54630004091758));
#42833=CARTESIAN_POINT('Ctrl Pts',(1.35,-7.96647938740201,2.74826728026557));
#42834=CARTESIAN_POINT('Ctrl Pts',(1.35,-5.30397004160299,6.54793541589078));
#42835=CARTESIAN_POINT('Ctrl Pts',(1.35,-1.0356886713384,8.36160627166494));
#42836=CARTESIAN_POINT('Ctrl Pts',(1.35,3.5467531368535,7.64591288957791));
#42837=CARTESIAN_POINT('Ctrl Pts',(1.35,7.05445628912872,4.60759922805685));
#42838=CARTESIAN_POINT('Ctrl Pts',(1.35,7.9668162212544,1.6571001514885));
#42839=CARTESIAN_POINT('Ctrl Pts',(1.35,7.99822721229278,0.168408611832292));
#42840=CARTESIAN_POINT('',(1.35,7.99822721229278,0.168408611832292));
#42841=CARTESIAN_POINT('',(1.5,8.14819390295858,0.171569570250815));
#42842=CARTESIAN_POINT('Ctrl Pts',(1.35,7.99822721229278,0.168408611832292));
#42843=CARTESIAN_POINT('Ctrl Pts',(1.38571428571429,8.0339335506847,0.169162005967588));
#42844=CARTESIAN_POINT('Ctrl Pts',(1.42857142857143,8.07678115675501,0.170066078929943));
#42845=CARTESIAN_POINT('Ctrl Pts',(1.47321428571429,8.12141407974491,0.171007821599063));
#42846=CARTESIAN_POINT('Ctrl Pts',(1.48392857142857,8.13212598126249,0.171233839839652));
#42847=CARTESIAN_POINT('Ctrl Pts',(1.48928571428572,8.13748193202128,0.171346848959947));
#42848=CARTESIAN_POINT('Ctrl Pts',(1.49464285714286,8.14283788278007,0.171459858080241));
#42849=CARTESIAN_POINT('Ctrl Pts',(1.49821428571429,8.14640851661926,0.171535197493771));
#42850=CARTESIAN_POINT('Ctrl Pts',(1.5,8.14819383353886,0.171572867200535));
#42851=CARTESIAN_POINT('Ctrl Pts',(1.5,8.14819383353886,0.171572867200535));
#42852=CARTESIAN_POINT('Ctrl Pts',(1.5,8.11619629477138,1.68806323182392));
#42853=CARTESIAN_POINT('Ctrl Pts',(1.5,7.18672995402067,4.69400338747101));
#42854=CARTESIAN_POINT('Ctrl Pts',(1.5,3.61325431606088,7.78925162987645));
#42855=CARTESIAN_POINT('Ctrl Pts',(1.5,-1.05510724703267,8.51840124378108));
#42856=CARTESIAN_POINT('Ctrl Pts',(1.5,-5.40342015315134,6.67067944450257));
#42857=CARTESIAN_POINT('Ctrl Pts',(1.5,-8.11584947195258,2.79986176826081));
#42858=CARTESIAN_POINT('Ctrl Pts',(1.5,-8.34751515590091,-1.57539769915707));
#42859=CARTESIAN_POINT('Ctrl Pts',(1.5,-6.63683129723738,-5.16900547712466));
#42860=CARTESIAN_POINT('Ctrl Pts',(1.5,-3.83187577666327,-7.49038443259283));
#42861=CARTESIAN_POINT('Ctrl Pts',(1.5,-0.306947971306406,-8.40596108242038));
#42862=CARTESIAN_POINT('Ctrl Pts',(1.5,3.27411598702021,-7.75142033677142));
#42863=CARTESIAN_POINT('Ctrl Pts',(1.5,6.2437277562345,-5.63228319243984));
#42864=CARTESIAN_POINT('Ctrl Pts',(1.5,7.82167697943358,-2.8606390589131));
#42865=CARTESIAN_POINT('Ctrl Pts',(1.5,8.13256980638789,-0.912057527264844));
#42866=CARTESIAN_POINT('Ctrl Pts',(1.5,8.14819397266823,-0.171566273307202));
#42867=CARTESIAN_POINT('Ctrl Pts',(1.35,7.99822721229006,-0.1684086118322));
#42868=CARTESIAN_POINT('Ctrl Pts',(1.35,7.9826024818273,-0.908897646744252));
#42869=CARTESIAN_POINT('Ctrl Pts',(1.35,7.67778229520457,-2.80497772582728));
#42870=CARTESIAN_POINT('Ctrl Pts',(1.35,6.12863466356929,-5.53707972089446));
#42871=CARTESIAN_POINT('Ctrl Pts',(1.35,3.21388161442135,-7.60755405802142));
#42872=CARTESIAN_POINT('Ctrl Pts',(1.35,-0.301325547464756,-8.25253002156739));
#42873=CARTESIAN_POINT('Ctrl Pts',(1.35,-3.76134157052312,-7.35210402830392));
#42874=CARTESIAN_POINT('Ctrl Pts',(1.35,-6.51468624709197,-5.07411807343295));
#42875=CARTESIAN_POINT('Ctrl Pts',(1.35,-8.19387773002112,-1.54630004091758));
#42876=CARTESIAN_POINT('Ctrl Pts',(1.35,-7.96647938740201,2.74826728026557));
#42877=CARTESIAN_POINT('Ctrl Pts',(1.35,-5.30397004160299,6.54793541589078));
#42878=CARTESIAN_POINT('Ctrl Pts',(1.35,-1.0356886713384,8.36160627166494));
#42879=CARTESIAN_POINT('Ctrl Pts',(1.35,3.5467531368535,7.64591288957791));
#42880=CARTESIAN_POINT('Ctrl Pts',(1.35,7.05445628912872,4.60759922805685));
#42881=CARTESIAN_POINT('Ctrl Pts',(1.35,7.9668162212544,1.6571001514885));
#42882=CARTESIAN_POINT('Ctrl Pts',(1.35,7.99822721229278,0.168408611832292));
#42883=CARTESIAN_POINT('Ctrl Pts',(0.,7.99822721229278,-0.168408611832294));
#42884=CARTESIAN_POINT('Ctrl Pts',(1.5,7.99822721229278,-0.168408611832294));
#42885=CARTESIAN_POINT('Ctrl Pts',(0.,7.99764130779638,-0.196176951432016));
#42886=CARTESIAN_POINT('Ctrl Pts',(1.5,7.99764130779638,-0.196176951432016));
#42887=CARTESIAN_POINT('Ctrl Pts',(0.,7.99622975691477,-0.251694874137705));
#42888=CARTESIAN_POINT('Ctrl Pts',(1.5,7.99622975691477,-0.251694874137705));
#42889=CARTESIAN_POINT('Ctrl Pts',(0.,7.99339320492592,-0.334915488714981));
#42890=CARTESIAN_POINT('Ctrl Pts',(1.5,7.99339320492592,-0.334915488714981));
#42891=CARTESIAN_POINT('Ctrl Pts',(0.,7.98817266620921,-0.445763767775749));
#42892=CARTESIAN_POINT('Ctrl Pts',(1.5,7.98817266620921,-0.445763767775749));
#42893=CARTESIAN_POINT('Ctrl Pts',(0.,7.97924974083877,-0.584134071638914));
#42894=CARTESIAN_POINT('Ctrl Pts',(1.5,7.97924974083877,-0.584134071638914));
#42895=CARTESIAN_POINT('Ctrl Pts',(0.,7.96793033524168,-0.722306911570631));
#42896=CARTESIAN_POINT('Ctrl Pts',(1.5,7.96793033524168,-0.722306911570631));
#42897=CARTESIAN_POINT('Ctrl Pts',(0.,7.95421612847075,-0.860267459956458));
#42898=CARTESIAN_POINT('Ctrl Pts',(1.5,7.95421612847075,-0.860267459956458));
#42899=CARTESIAN_POINT('Ctrl Pts',(0.,7.93811003951485,-0.997991012912835));
#42900=CARTESIAN_POINT('Ctrl Pts',(1.5,7.93811003951485,-0.997991012912835));
#42901=CARTESIAN_POINT('Ctrl Pts',(0.,7.91961655999501,-1.1354405222898));
#42902=CARTESIAN_POINT('Ctrl Pts',(1.5,7.91961655999501,-1.1354405222898));
#42903=CARTESIAN_POINT('Ctrl Pts',(0.,7.89874150358321,-1.27257026968344));
#42904=CARTESIAN_POINT('Ctrl Pts',(1.5,7.89874150358321,-1.27257026968344));
#42905=CARTESIAN_POINT('Ctrl Pts',(0.,7.87549175548901,-1.40932954012024));
#42906=CARTESIAN_POINT('Ctrl Pts',(1.5,7.87549175548901,-1.40932954012024));
#42907=CARTESIAN_POINT('Ctrl Pts',(0.,7.84987502200417,-1.54566629555733));
#42908=CARTESIAN_POINT('Ctrl Pts',(1.5,7.84987502200417,-1.54566629555733));
#42909=CARTESIAN_POINT('Ctrl Pts',(0.,7.82189958009612,-1.68153084833392));
#42910=CARTESIAN_POINT('Ctrl Pts',(1.5,7.82189958009612,-1.68153084833392));
#42911=CARTESIAN_POINT('Ctrl Pts',(0.,7.79157402704011,-1.81687953471755));
#42912=CARTESIAN_POINT('Ctrl Pts',(1.5,7.79157402704011,-1.81687953471755));
#42913=CARTESIAN_POINT('Ctrl Pts',(0.,7.7589073889474,-1.95167303870642));
#42914=CARTESIAN_POINT('Ctrl Pts',(1.5,7.7589073889474,-1.95167303870642));
#42915=CARTESIAN_POINT('Ctrl Pts',(0.,7.72390922932679,-2.08587471600204));
#42916=CARTESIAN_POINT('Ctrl Pts',(1.5,7.72390922932679,-2.08587471600204));
#42917=CARTESIAN_POINT('Ctrl Pts',(0.,7.68658975768396,-2.21944891808571));
#42918=CARTESIAN_POINT('Ctrl Pts',(1.5,7.68658975768396,-2.21944891808571));
#42919=CARTESIAN_POINT('Ctrl Pts',(0.,7.64695993816252,-2.35235931633769));
#42920=CARTESIAN_POINT('Ctrl Pts',(1.5,7.64695993816252,-2.35235931633769));
#42921=CARTESIAN_POINT('Ctrl Pts',(0.,7.60503159823077,-2.48456722613405));
#42922=CARTESIAN_POINT('Ctrl Pts',(1.5,7.60503159823077,-2.48456722613405));
#42923=CARTESIAN_POINT('Ctrl Pts',(0.,7.56081737636842,-2.61603235046274));
#42924=CARTESIAN_POINT('Ctrl Pts',(1.5,7.56081737636842,-2.61603235046274));
#42925=CARTESIAN_POINT('Ctrl Pts',(0.,7.51433066980093,-2.74671352348261));
#42926=CARTESIAN_POINT('Ctrl Pts',(1.5,7.51433066980093,-2.74671352348261));
#42927=CARTESIAN_POINT('Ctrl Pts',(0.,7.46558558227944,-2.87656945405589));
#42928=CARTESIAN_POINT('Ctrl Pts',(1.5,7.46558558227944,-2.87656945405589));
#42929=CARTESIAN_POINT('Ctrl Pts',(0.,7.41459687190435,-3.00555946928131));
#42930=CARTESIAN_POINT('Ctrl Pts',(1.5,7.41459687190435,-3.00555946928131));
#42931=CARTESIAN_POINT('Ctrl Pts',(0.,7.36137989899016,-3.13364425805735));
#42932=CARTESIAN_POINT('Ctrl Pts',(1.5,7.36137989899016,-3.13364425805735));
#42933=CARTESIAN_POINT('Ctrl Pts',(0.,7.30595064174916,-3.26078556725641));
#42934=CARTESIAN_POINT('Ctrl Pts',(1.5,7.30595064174916,-3.26078556725641));
#42935=CARTESIAN_POINT('Ctrl Pts',(0.,7.24832571201489,-3.38694589794601));
#42936=CARTESIAN_POINT('Ctrl Pts',(1.5,7.24832571201489,-3.38694589794601));
#42937=CARTESIAN_POINT('Ctrl Pts',(0.,7.18852237100625,-3.51208820164554));
#42938=CARTESIAN_POINT('Ctrl Pts',(1.5,7.18852237100625,-3.51208820164554));
#42939=CARTESIAN_POINT('Ctrl Pts',(0.,7.1265585451321,-3.63617557660718));
#42940=CARTESIAN_POINT('Ctrl Pts',(1.5,7.1265585451321,-3.63617557660718));
#42941=CARTESIAN_POINT('Ctrl Pts',(0.,7.0624528418373,-3.75917096410974));
#42942=CARTESIAN_POINT('Ctrl Pts',(1.5,7.0624528418373,-3.75917096410974));
#42943=CARTESIAN_POINT('Ctrl Pts',(0.,6.9962245345929,-3.88103729518562));
#42944=CARTESIAN_POINT('Ctrl Pts',(1.5,6.9962245345929,-3.88103729518562));
#42945=CARTESIAN_POINT('Ctrl Pts',(0.,6.92789354792742,-4.00173763735532));
#42946=CARTESIAN_POINT('Ctrl Pts',(1.5,6.92789354792742,-4.00173763735532));
#42947=CARTESIAN_POINT('Ctrl Pts',(0.,6.8574804424984,-4.12123534137538));
#42948=CARTESIAN_POINT('Ctrl Pts',(1.5,6.8574804424984,-4.12123534137538));
#42949=CARTESIAN_POINT('Ctrl Pts',(0.,6.78500640020348,-4.23949418800576));
#42950=CARTESIAN_POINT('Ctrl Pts',(1.5,6.78500640020348,-4.23949418800576));
#42951=CARTESIAN_POINT('Ctrl Pts',(0.,6.7104932093306,-4.35647853480234));
#42952=CARTESIAN_POINT('Ctrl Pts',(1.5,6.7104932093306,-4.35647853480234));
#42953=CARTESIAN_POINT('Ctrl Pts',(0.,6.63396326141838,-4.47215326806802));
#42954=CARTESIAN_POINT('Ctrl Pts',(1.5,6.63396326141838,-4.47215326806802));
#42955=CARTESIAN_POINT('Ctrl Pts',(0.,6.55543954815452,-4.58648375483326));
#42956=CARTESIAN_POINT('Ctrl Pts',(1.5,6.55543954815452,-4.58648375483326));
#42957=CARTESIAN_POINT('Ctrl Pts',(0.,6.47494565831181,-4.69943579486461));
#42958=CARTESIAN_POINT('Ctrl Pts',(1.5,6.47494565831181,-4.69943579486461));
#42959=CARTESIAN_POINT('Ctrl Pts',(0.,6.39250577472155,-4.81097557269941));
#42960=CARTESIAN_POINT('Ctrl Pts',(1.5,6.39250577472155,-4.81097557269941));
#42961=CARTESIAN_POINT('Ctrl Pts',(0.,6.30814467128388,-4.92106960970514));
#42962=CARTESIAN_POINT('Ctrl Pts',(1.5,6.30814467128388,-4.92106960970514));
#42963=CARTESIAN_POINT('Ctrl Pts',(0.,6.2218877034437,-5.02968479900636));
#42964=CARTESIAN_POINT('Ctrl Pts',(1.5,6.2218877034437,-5.02968479900636));
#42965=CARTESIAN_POINT('Ctrl Pts',(0.,6.13376079870311,-5.13678844043638));
#42966=CARTESIAN_POINT('Ctrl Pts',(1.5,6.13376079870311,-5.13678844043638));
#42967=CARTESIAN_POINT('Ctrl Pts',(0.,6.0437904471692,-5.24234827551529));
#42968=CARTESIAN_POINT('Ctrl Pts',(1.5,6.0437904471692,-5.24234827551529));
#42969=CARTESIAN_POINT('Ctrl Pts',(0.,5.9520036921371,-5.34633252245589));
#42970=CARTESIAN_POINT('Ctrl Pts',(1.5,5.9520036921371,-5.34633252245589));
#42971=CARTESIAN_POINT('Ctrl Pts',(0.,5.85842812070735,-5.44870991119904));
#42972=CARTESIAN_POINT('Ctrl Pts',(1.5,5.85842812070735,-5.44870991119904));
#42973=CARTESIAN_POINT('Ctrl Pts',(0.,5.76309185581909,-5.54944968161907));
#42974=CARTESIAN_POINT('Ctrl Pts',(1.5,5.76309185581909,-5.54944968161907));
#42975=CARTESIAN_POINT('Ctrl Pts',(0.,5.66602354831668,-5.64852158176045));
#42976=CARTESIAN_POINT('Ctrl Pts',(1.5,5.66602354831668,-5.64852158176045));
#42977=CARTESIAN_POINT('Ctrl Pts',(0.,5.56725236904917,-5.74589586610578));
#42978=CARTESIAN_POINT('Ctrl Pts',(1.5,5.56725236904917,-5.74589586610578));
#42979=CARTESIAN_POINT('Ctrl Pts',(0.,5.46680800100265,-5.84154329387539));
#42980=CARTESIAN_POINT('Ctrl Pts',(1.5,5.46680800100265,-5.84154329387539));
#42981=CARTESIAN_POINT('Ctrl Pts',(0.,5.36472063146399,-5.93543512735822));
#42982=CARTESIAN_POINT('Ctrl Pts',(1.5,5.36472063146399,-5.93543512735822));
#42983=CARTESIAN_POINT('Ctrl Pts',(0.,5.26102094228231,-6.02754314483389));
#42984=CARTESIAN_POINT('Ctrl Pts',(1.5,5.26102094228231,-6.02754314483389));
#42985=CARTESIAN_POINT('Ctrl Pts',(0.,5.15574010016132,-6.11783965352703));
#42986=CARTESIAN_POINT('Ctrl Pts',(1.5,5.15574010016132,-6.11783965352703));
#42987=CARTESIAN_POINT('Ctrl Pts',(0.,5.04890974698177,-6.20629750259511));
#42988=CARTESIAN_POINT('Ctrl Pts',(1.5,5.04890974698177,-6.20629750259511));
#42989=CARTESIAN_POINT('Ctrl Pts',(0.,4.94056199015376,-6.29289009614986));
#42990=CARTESIAN_POINT('Ctrl Pts',(1.5,4.94056199015376,-6.29289009614986));
#42991=CARTESIAN_POINT('Ctrl Pts',(0.,4.83072939299784,-6.3775914063135));
#42992=CARTESIAN_POINT('Ctrl Pts',(1.5,4.83072939299784,-6.3775914063135));
#42993=CARTESIAN_POINT('Ctrl Pts',(0.,4.71944496476703,-6.46037597861881));
#42994=CARTESIAN_POINT('Ctrl Pts',(1.5,4.71944496476703,-6.46037597861881));
#42995=CARTESIAN_POINT('Ctrl Pts',(0.,4.60674215069668,-6.54121893744458));
#42996=CARTESIAN_POINT('Ctrl Pts',(1.5,4.60674215069668,-6.54121893744458));
#42997=CARTESIAN_POINT('Ctrl Pts',(0.,4.49265482208138,-6.62009599148724));
#42998=CARTESIAN_POINT('Ctrl Pts',(1.5,4.49265482208138,-6.62009599148724));
#42999=CARTESIAN_POINT('Ctrl Pts',(0.,4.37721726637847,-6.69698343926892));
#43000=CARTESIAN_POINT('Ctrl Pts',(1.5,4.37721726637847,-6.69698343926892));
#43001=CARTESIAN_POINT('Ctrl Pts',(0.,4.26046417733745,-6.7718581746823));
#43002=CARTESIAN_POINT('Ctrl Pts',(1.5,4.26046417733745,-6.7718581746823));
#43003=CARTESIAN_POINT('Ctrl Pts',(0.,4.14243064422915,-6.84469769436137));
#43004=CARTESIAN_POINT('Ctrl Pts',(1.5,4.14243064422915,-6.84469769436137));
#43005=CARTESIAN_POINT('Ctrl Pts',(0.,4.02315214109941,-6.91548010508963));
#43006=CARTESIAN_POINT('Ctrl Pts',(1.5,4.02315214109941,-6.91548010508963));
#43007=CARTESIAN_POINT('Ctrl Pts',(0.,3.90266451604688,-6.98418413124661));
#43008=CARTESIAN_POINT('Ctrl Pts',(1.5,3.90266451604688,-6.98418413124661));
#43009=CARTESIAN_POINT('Ctrl Pts',(0.,3.78100398052421,-7.05078912229274));
#43010=CARTESIAN_POINT('Ctrl Pts',(1.5,3.78100398052421,-7.05078912229274));
#43011=CARTESIAN_POINT('Ctrl Pts',(0.,3.658207098662,-7.11527506029345));
#43012=CARTESIAN_POINT('Ctrl Pts',(1.5,3.658207098662,-7.11527506029345));
#43013=CARTESIAN_POINT('Ctrl Pts',(0.,3.53431077605632,-7.17762256510059));
#43014=CARTESIAN_POINT('Ctrl Pts',(1.5,3.53431077605632,-7.17762256510059));
#43015=CARTESIAN_POINT('Ctrl Pts',(0.,3.40935224857761,-7.23781289957334));
#43016=CARTESIAN_POINT('Ctrl Pts',(1.5,3.40935224857761,-7.23781289957334));
#43017=CARTESIAN_POINT('Ctrl Pts',(0.,3.28336907120022,-7.29582797483959));
#43018=CARTESIAN_POINT('Ctrl Pts',(1.5,3.28336907120022,-7.29582797483959));
#43019=CARTESIAN_POINT('Ctrl Pts',(0.,3.15639910685184,-7.35165035559749));
#43020=CARTESIAN_POINT('Ctrl Pts',(1.5,3.15639910685184,-7.35165035559749));
#43021=CARTESIAN_POINT('Ctrl Pts',(0.,3.02848051528223,-7.40526326545788));
#43022=CARTESIAN_POINT('Ctrl Pts',(1.5,3.02848051528223,-7.40526326545788));
#43023=CARTESIAN_POINT('Ctrl Pts',(0.,2.89965174137715,-7.45665059166467));
#43024=CARTESIAN_POINT('Ctrl Pts',(1.5,2.89965174137715,-7.45665059166467));
#43025=CARTESIAN_POINT('Ctrl Pts',(0.,2.76995150349014,-7.50579688985674));
#43026=CARTESIAN_POINT('Ctrl Pts',(1.5,2.76995150349014,-7.50579688985674));
#43027=CARTESIAN_POINT('Ctrl Pts',(0.,2.63941878179125,-7.55268738887152));
#43028=CARTESIAN_POINT('Ctrl Pts',(1.5,2.63941878179125,-7.55268738887152));
#43029=CARTESIAN_POINT('Ctrl Pts',(0.,2.50809280663222,-7.59730799559061));
#43030=CARTESIAN_POINT('Ctrl Pts',(1.5,2.50809280663222,-7.59730799559061));
#43031=CARTESIAN_POINT('Ctrl Pts',(0.,2.37601304692718,-7.63964529982775));
#43032=CARTESIAN_POINT('Ctrl Pts',(1.5,2.37601304692718,-7.63964529982775));
#43033=CARTESIAN_POINT('Ctrl Pts',(0.,2.24321919813061,-7.67968657779174));
#43034=CARTESIAN_POINT('Ctrl Pts',(1.5,2.24321919813061,-7.67968657779174));
#43035=CARTESIAN_POINT('Ctrl Pts',(0.,2.10975117022955,-7.71741979559249));
#43036=CARTESIAN_POINT('Ctrl Pts',(1.5,2.10975117022955,-7.71741979559249));
#43037=CARTESIAN_POINT('Ctrl Pts',(0.,1.97564907574918,-7.7528336127899));
#43038=CARTESIAN_POINT('Ctrl Pts',(1.5,1.97564907574918,-7.7528336127899));
#43039=CARTESIAN_POINT('Ctrl Pts',(0.,1.84095321777114,-7.78591738598633));
#43040=CARTESIAN_POINT('Ctrl Pts',(1.5,1.84095321777114,-7.78591738598633));
#43041=CARTESIAN_POINT('Ctrl Pts',(0.,1.70570407796376,-7.81666117246218));
#43042=CARTESIAN_POINT('Ctrl Pts',(1.5,1.70570407796376,-7.81666117246218));
#43043=CARTESIAN_POINT('Ctrl Pts',(0.,1.56994230429296,-7.84505573268351));
#43044=CARTESIAN_POINT('Ctrl Pts',(1.5,1.56994230429296,-7.84505573268351));
#43045=CARTESIAN_POINT('Ctrl Pts',(0.,1.43370869874369,-7.87109253285344));
#43046=CARTESIAN_POINT('Ctrl Pts',(1.5,1.43370869874369,-7.87109253285344));
#43047=CARTESIAN_POINT('Ctrl Pts',(0.,1.29704420505069,-7.89476374750745));
#43048=CARTESIAN_POINT('Ctrl Pts',(1.5,1.29704420505069,-7.89476374750745));
#43049=CARTESIAN_POINT('Ctrl Pts',(0.,1.15998989643835,-7.91606226215288));
#43050=CARTESIAN_POINT('Ctrl Pts',(1.5,1.15998989643835,-7.91606226215288));
#43051=CARTESIAN_POINT('Ctrl Pts',(0.,1.02258696336842,-7.93498167595306));
#43052=CARTESIAN_POINT('Ctrl Pts',(1.5,1.02258696336842,-7.93498167595306));
#43053=CARTESIAN_POINT('Ctrl Pts',(0.,0.884876701085412,-7.95151630311911));
#43054=CARTESIAN_POINT('Ctrl Pts',(1.5,0.884876701085412,-7.95151630311911));
#43055=CARTESIAN_POINT('Ctrl Pts',(0.,0.746900497168579,-7.96566117434639));
#43056=CARTESIAN_POINT('Ctrl Pts',(1.5,0.746900497168579,-7.96566117434639));
#43057=CARTESIAN_POINT('Ctrl Pts',(0.,0.608699819089495,-7.97741203829576));
#43058=CARTESIAN_POINT('Ctrl Pts',(1.5,0.608699819089495,-7.97741203829576));
#43059=CARTESIAN_POINT('Ctrl Pts',(0.,0.470316201774848,-7.98676536311966));
#43060=CARTESIAN_POINT('Ctrl Pts',(1.5,0.470316201774848,-7.98676536311966));
#43061=CARTESIAN_POINT('Ctrl Pts',(0.,0.331791235173314,-7.99371833803316));
#43062=CARTESIAN_POINT('Ctrl Pts',(1.5,0.331791235173314,-7.99371833803316));
#43063=CARTESIAN_POINT('Ctrl Pts',(0.,0.193166551724818,-7.99826887364049));
#43064=CARTESIAN_POINT('Ctrl Pts',(1.5,0.193166551724818,-7.99826887364049));
#43065=CARTESIAN_POINT('Ctrl Pts',(0.,0.0544838138324683,-8.00041560230666));
#43066=CARTESIAN_POINT('Ctrl Pts',(1.5,0.0544838138324683,-8.00041560230666));
#43067=CARTESIAN_POINT('Ctrl Pts',(0.,-0.0842152986636308,-8.0001578785741));
#43068=CARTESIAN_POINT('Ctrl Pts',(1.5,-0.0842152986636308,-8.0001578785741));
#43069=CARTESIAN_POINT('Ctrl Pts',(0.,-0.222889101011495,-7.99749577962445));
#43070=CARTESIAN_POINT('Ctrl Pts',(1.5,-0.222889101011495,-7.99749577962445));
#43071=CARTESIAN_POINT('Ctrl Pts',(0.,-0.361495916071951,-7.99243010578557));
#43072=CARTESIAN_POINT('Ctrl Pts',(1.5,-0.361495916071951,-7.99243010578557));
#43073=CARTESIAN_POINT('Ctrl Pts',(0.,-0.499994086829513,-7.98496237976419));
#43074=CARTESIAN_POINT('Ctrl Pts',(1.5,-0.499994086829513,-7.98496237976419));
#43075=CARTESIAN_POINT('Ctrl Pts',(0.,-0.638341988904545,-7.9750948459236));
#43076=CARTESIAN_POINT('Ctrl Pts',(1.5,-0.638341988904545,-7.9750948459236));
#43077=CARTESIAN_POINT('Ctrl Pts',(0.,-0.776498043067469,-7.96283046960652));
#43078=CARTESIAN_POINT('Ctrl Pts',(1.5,-0.776498043067469,-7.96283046960652));
#43079=CARTESIAN_POINT('Ctrl Pts',(0.,-0.914420727755825,-7.94817293650308));
#43080=CARTESIAN_POINT('Ctrl Pts',(1.5,-0.914420727755825,-7.94817293650308));
#43081=CARTESIAN_POINT('Ctrl Pts',(0.,-1.05206859159497,-7.93112665206354));
#43082=CARTESIAN_POINT('Ctrl Pts',(1.5,-1.05206859159497,-7.93112665206354));
#43083=CARTESIAN_POINT('Ctrl Pts',(0.,-1.18940026579597,-7.91169673965436));
#43084=CARTESIAN_POINT('Ctrl Pts',(1.5,-1.18940026579597,-7.91169673965436));
#43085=CARTESIAN_POINT('Ctrl Pts',(0.,-1.3263744765588,-7.88988903875861));
#43086=CARTESIAN_POINT('Ctrl Pts',(1.5,-1.3263744765588,-7.88988903875861));
#43087=CARTESIAN_POINT('Ctrl Pts',(0.,-1.4629500574812,-7.86571010322161));
#43088=CARTESIAN_POINT('Ctrl Pts',(1.5,-1.4629500574812,-7.86571010322161));
#43089=CARTESIAN_POINT('Ctrl Pts',(0.,-1.59908596197461,-7.83916719954087));
#43090=CARTESIAN_POINT('Ctrl Pts',(1.5,-1.59908596197461,-7.83916719954087));
#43091=CARTESIAN_POINT('Ctrl Pts',(0.,-1.73474127568722,-7.81026830520049));
#43092=CARTESIAN_POINT('Ctrl Pts',(1.5,-1.73474127568722,-7.81026830520049));
#43093=CARTESIAN_POINT('Ctrl Pts',(0.,-1.86987522869551,-7.77902210575902));
#43094=CARTESIAN_POINT('Ctrl Pts',(1.5,-1.86987522869551,-7.77902210575902));
#43095=CARTESIAN_POINT('Ctrl Pts',(0.,-2.00444720770498,-7.74543799198167));
#43096=CARTESIAN_POINT('Ctrl Pts',(1.5,-2.00444720770498,-7.74543799198167));
#43097=CARTESIAN_POINT('Ctrl Pts',(0.,-2.13841676826037,-7.70952605701667));
#43098=CARTESIAN_POINT('Ctrl Pts',(1.5,-2.13841676826037,-7.70952605701667));
#43099=CARTESIAN_POINT('Ctrl Pts',(0.,-2.27174364696663,-7.67129709361539));
#43100=CARTESIAN_POINT('Ctrl Pts',(1.5,-2.27174364696663,-7.67129709361539));
#43101=CARTESIAN_POINT('Ctrl Pts',(0.,-2.40438777372114,-7.63076259139598));
#43102=CARTESIAN_POINT('Ctrl Pts',(1.5,-2.40438777372114,-7.63076259139598));
#43103=CARTESIAN_POINT('Ctrl Pts',(0.,-2.53630928360746,-7.58793473288758));
#43104=CARTESIAN_POINT('Ctrl Pts',(1.5,-2.53630928360746,-7.58793473288758));
#43105=CARTESIAN_POINT('Ctrl Pts',(0.,-2.66746852880189,-7.54282638961755));
#43106=CARTESIAN_POINT('Ctrl Pts',(1.5,-2.66746852880189,-7.54282638961755));
#43107=CARTESIAN_POINT('Ctrl Pts',(0.,-2.79782609049359,-7.49545111824191));
#43108=CARTESIAN_POINT('Ctrl Pts',(1.5,-2.79782609049359,-7.49545111824191));
#43109=CARTESIAN_POINT('Ctrl Pts',(0.,-2.92734279081898,-7.4458231567185));
#43110=CARTESIAN_POINT('Ctrl Pts',(1.5,-2.92734279081898,-7.4458231567185));
#43111=CARTESIAN_POINT('Ctrl Pts',(0.,-3.05597970481126,-7.39395742052261));
#43112=CARTESIAN_POINT('Ctrl Pts',(1.5,-3.05597970481126,-7.39395742052261));
#43113=CARTESIAN_POINT('Ctrl Pts',(0.,-3.18369817190697,-7.33986949767589));
#43114=CARTESIAN_POINT('Ctrl Pts',(1.5,-3.18369817190697,-7.33986949767589));
#43115=CARTESIAN_POINT('Ctrl Pts',(0.,-3.31045980746918,-7.28357564381743));
#43116=CARTESIAN_POINT('Ctrl Pts',(1.5,-3.31045980746918,-7.28357564381743));
#43117=CARTESIAN_POINT('Ctrl Pts',(0.,-3.43622651432776,-7.2250927773164));
#43118=CARTESIAN_POINT('Ctrl Pts',(1.5,-3.43622651432776,-7.2250927773164));
#43119=CARTESIAN_POINT('Ctrl Pts',(0.,-3.56096049433766,-7.16443847442603));
#43120=CARTESIAN_POINT('Ctrl Pts',(1.5,-3.56096049433766,-7.16443847442603));
#43121=CARTESIAN_POINT('Ctrl Pts',(0.,-3.6846242599558,-7.10163096447882));
#43122=CARTESIAN_POINT('Ctrl Pts',(1.5,-3.6846242599558,-7.10163096447882));
#43123=CARTESIAN_POINT('Ctrl Pts',(0.,-3.80718064527425,-7.03668912393815));
#43124=CARTESIAN_POINT('Ctrl Pts',(1.5,-3.80718064527425,-7.03668912393815));
#43125=CARTESIAN_POINT('Ctrl Pts',(0.,-3.92859281707327,-6.96963247049021));
#43126=CARTESIAN_POINT('Ctrl Pts',(1.5,-3.92859281707327,-6.96963247049021));
#43127=CARTESIAN_POINT('Ctrl Pts',(0.,-4.04882428589532,-6.90048115717619));
#43128=CARTESIAN_POINT('Ctrl Pts',(1.5,-4.04882428589532,-6.90048115717619));
#43129=CARTESIAN_POINT('Ctrl Pts',(0.,-4.16783891714033,-6.82925596656376));
#43130=CARTESIAN_POINT('Ctrl Pts',(1.5,-4.16783891714033,-6.82925596656376));
#43131=CARTESIAN_POINT('Ctrl Pts',(0.,-4.28560094218327,-6.75597830495819));
#43132=CARTESIAN_POINT('Ctrl Pts',(1.5,-4.28560094218327,-6.75597830495819));
#43133=CARTESIAN_POINT('Ctrl Pts',(0.,-4.40207496885083,-6.6806701955211));
#43134=CARTESIAN_POINT('Ctrl Pts',(1.5,-4.40207496885083,-6.6806701955211));
#43135=CARTESIAN_POINT('Ctrl Pts',(0.,-4.51722599192152,-6.60335427142775));
#43136=CARTESIAN_POINT('Ctrl Pts',(1.5,-4.51722599192152,-6.60335427142775));
#43137=CARTESIAN_POINT('Ctrl Pts',(0.,-4.63101940365,-6.52405376906231));
#43138=CARTESIAN_POINT('Ctrl Pts',(1.5,-4.63101940365,-6.52405376906231));
#43139=CARTESIAN_POINT('Ctrl Pts',(0.,-4.74342100431622,-6.44279252125083));
#43140=CARTESIAN_POINT('Ctrl Pts',(1.5,-4.74342100431622,-6.44279252125083));
#43141=CARTESIAN_POINT('Ctrl Pts',(0.,-4.85439701280005,-6.35959495053137));
#43142=CARTESIAN_POINT('Ctrl Pts',(1.5,-4.85439701280005,-6.35959495053137));
#43143=CARTESIAN_POINT('Ctrl Pts',(0.,-4.96391407642278,-6.27448606139168));
#43144=CARTESIAN_POINT('Ctrl Pts',(1.5,-4.96391407642278,-6.27448606139168));
#43145=CARTESIAN_POINT('Ctrl Pts',(0.,-5.07193928081559,-6.18749143254318));
#43146=CARTESIAN_POINT('Ctrl Pts',(1.5,-5.07193928081559,-6.18749143254318));
#43147=CARTESIAN_POINT('Ctrl Pts',(0.,-5.17844015981525,-6.0986372092306));
#43148=CARTESIAN_POINT('Ctrl Pts',(1.5,-5.17844015981525,-6.0986372092306));
#43149=CARTESIAN_POINT('Ctrl Pts',(0.,-5.28338470538775,-6.00795009557728));
#43150=CARTESIAN_POINT('Ctrl Pts',(1.5,-5.28338470538775,-6.00795009557728));
#43151=CARTESIAN_POINT('Ctrl Pts',(0.,-5.38674137758061,-5.91545734696511));
#43152=CARTESIAN_POINT('Ctrl Pts',(1.5,-5.38674137758061,-5.91545734696511));
#43153=CARTESIAN_POINT('Ctrl Pts',(0.,-5.48847911365542,-5.82118676144916));
#43154=CARTESIAN_POINT('Ctrl Pts',(1.5,-5.48847911365542,-5.82118676144916));
#43155=CARTESIAN_POINT('Ctrl Pts',(0.,-5.58856733725029,-5.72516667120635));
#43156=CARTESIAN_POINT('Ctrl Pts',(1.5,-5.58856733725029,-5.72516667120635));
#43157=CARTESIAN_POINT('Ctrl Pts',(0.,-5.68697596757266,-5.6274259340173));
#43158=CARTESIAN_POINT('Ctrl Pts',(1.5,-5.68697596757266,-5.6274259340173));
#43159=CARTESIAN_POINT('Ctrl Pts',(0.,-5.783675428623,-5.52799392478112));
#43160=CARTESIAN_POINT('Ctrl Pts',(1.5,-5.783675428623,-5.52799392478112));
#43161=CARTESIAN_POINT('Ctrl Pts',(0.,-5.87863665845019,-5.42690052706247));
#43162=CARTESIAN_POINT('Ctrl Pts',(1.5,-5.87863665845019,-5.42690052706247));
#43163=CARTESIAN_POINT('Ctrl Pts',(0.,-5.97183111750645,-5.32417612374785));
#43164=CARTESIAN_POINT('Ctrl Pts',(1.5,-5.97183111750645,-5.32417612374785));
#43165=CARTESIAN_POINT('Ctrl Pts',(0.,-6.06323079703504,-5.21985158773308));
#43166=CARTESIAN_POINT('Ctrl Pts',(1.5,-6.06323079703504,-5.21985158773308));
#43167=CARTESIAN_POINT('Ctrl Pts',(0.,-6.15280822749109,-5.11395827264137));
#43168=CARTESIAN_POINT('Ctrl Pts',(1.5,-6.15280822749109,-5.11395827264137));
#43169=CARTESIAN_POINT('Ctrl Pts',(0.,-6.2405364869961,-5.0065280035714));
#43170=CARTESIAN_POINT('Ctrl Pts',(1.5,-6.2405364869961,-5.0065280035714));
#43171=CARTESIAN_POINT('Ctrl Pts',(0.,-6.32638920982662,-4.89759306787482));
#43172=CARTESIAN_POINT('Ctrl Pts',(1.5,-6.32638920982662,-4.89759306787482));
#43173=CARTESIAN_POINT('Ctrl Pts',(0.,-6.41034059392906,-4.78718620512425));
#43174=CARTESIAN_POINT('Ctrl Pts',(1.5,-6.41034059392906,-4.78718620512425));
#43175=CARTESIAN_POINT('Ctrl Pts',(0.,-6.49236540846972,-4.67534059710961));
#43176=CARTESIAN_POINT('Ctrl Pts',(1.5,-6.49236540846972,-4.67534059710961));
#43177=CARTESIAN_POINT('Ctrl Pts',(0.,-6.57243900142041,-4.56208985786201));
#43178=CARTESIAN_POINT('Ctrl Pts',(1.5,-6.57243900142041,-4.56208985786201));
#43179=CARTESIAN_POINT('Ctrl Pts',(0.,-6.65053730718027,-4.44746802370464));
#43180=CARTESIAN_POINT('Ctrl Pts',(1.5,-6.65053730718027,-4.44746802370464));
#43181=CARTESIAN_POINT('Ctrl Pts',(0.,-6.72663685423419,-4.33150954333007));
#43182=CARTESIAN_POINT('Ctrl Pts',(1.5,-6.72663685423419,-4.33150954333007));
#43183=CARTESIAN_POINT('Ctrl Pts',(0.,-6.80071477177081,-4.21424926715533));
#43184=CARTESIAN_POINT('Ctrl Pts',(1.5,-6.80071477177081,-4.21424926715533));
#43185=CARTESIAN_POINT('Ctrl Pts',(0.,-6.87274879633804,-4.09572243670215));
#43186=CARTESIAN_POINT('Ctrl Pts',(1.5,-6.87274879633804,-4.09572243670215));
#43187=CARTESIAN_POINT('Ctrl Pts',(0.,-6.94271727853662,-3.97596467400157));
#43188=CARTESIAN_POINT('Ctrl Pts',(1.5,-6.94271727853662,-3.97596467400157));
#43189=CARTESIAN_POINT('Ctrl Pts',(0.,-7.01059918975196,-3.85501197102232));
#43190=CARTESIAN_POINT('Ctrl Pts',(1.5,-7.01059918975196,-3.85501197102232));
#43191=CARTESIAN_POINT('Ctrl Pts',(0.,-7.07637412892475,-3.73290067912243));
#43192=CARTESIAN_POINT('Ctrl Pts',(1.5,-7.07637412892475,-3.73290067912243));
#43193=CARTESIAN_POINT('Ctrl Pts',(0.,-7.14002232822272,-3.60966749787132));
#43194=CARTESIAN_POINT('Ctrl Pts',(1.5,-7.14002232822272,-3.60966749787132));
#43195=CARTESIAN_POINT('Ctrl Pts',(0.,-7.20152465875188,-3.48534946389366));
#43196=CARTESIAN_POINT('Ctrl Pts',(1.5,-7.20152465875188,-3.48534946389366));
#43197=CARTESIAN_POINT('Ctrl Pts',(0.,-7.26086263630753,-3.3599839397343));
#43198=CARTESIAN_POINT('Ctrl Pts',(1.5,-7.26086263630753,-3.3599839397343));
#43199=CARTESIAN_POINT('Ctrl Pts',(0.,-7.31801842716562,-3.23360860274355));
#43200=CARTESIAN_POINT('Ctrl Pts',(1.5,-7.31801842716562,-3.23360860274355));
#43201=CARTESIAN_POINT('Ctrl Pts',(0.,-7.37297485391472,-3.1062614339821));
#43202=CARTESIAN_POINT('Ctrl Pts',(1.5,-7.37297485391472,-3.1062614339821));
#43203=CARTESIAN_POINT('Ctrl Pts',(0.,-7.42571540013862,-2.97798070659427));
#43204=CARTESIAN_POINT('Ctrl Pts',(1.5,-7.42571540013862,-2.97798070659427));
#43205=CARTESIAN_POINT('Ctrl Pts',(0.,-7.47622421514032,-2.84880497419933));
#43206=CARTESIAN_POINT('Ctrl Pts',(1.5,-7.47622421514032,-2.84880497419933));
#43207=CARTESIAN_POINT('Ctrl Pts',(0.,-7.52448611870752,-2.71877305930032));
#43208=CARTESIAN_POINT('Ctrl Pts',(1.5,-7.52448611870752,-2.71877305930032));
#43209=CARTESIAN_POINT('Ctrl Pts',(0.,-7.57048660592005,-2.58792404170972));
#43210=CARTESIAN_POINT('Ctrl Pts',(1.5,-7.57048660592005,-2.58792404170972));
#43211=CARTESIAN_POINT('Ctrl Pts',(0.,-7.61421185199946,-2.45629724699105));
#43212=CARTESIAN_POINT('Ctrl Pts',(1.5,-7.61421185199946,-2.45629724699105));
#43213=CARTESIAN_POINT('Ctrl Pts',(0.,-7.65564871596749,-2.32393223447027));
#43214=CARTESIAN_POINT('Ctrl Pts',(1.5,-7.65564871596749,-2.32393223447027));
#43215=CARTESIAN_POINT('Ctrl Pts',(0.,-7.69478474434726,-2.19086878526178));
#43216=CARTESIAN_POINT('Ctrl Pts',(1.5,-7.69478474434726,-2.19086878526178));
#43217=CARTESIAN_POINT('Ctrl Pts',(0.,-7.73160817490736,-2.05714689030825));
#43218=CARTESIAN_POINT('Ctrl Pts',(1.5,-7.73160817490736,-2.05714689030825));
#43219=CARTESIAN_POINT('Ctrl Pts',(0.,-7.76610794044926,-1.92280673843347));
#43220=CARTESIAN_POINT('Ctrl Pts',(1.5,-7.76610794044926,-1.92280673843347));
#43221=CARTESIAN_POINT('Ctrl Pts',(0.,-7.79827367263786,-1.78788870440769));
#43222=CARTESIAN_POINT('Ctrl Pts',(1.5,-7.79827367263786,-1.78788870440769));
#43223=CARTESIAN_POINT('Ctrl Pts',(0.,-7.82809570460851,-1.65243333668723));
#43224=CARTESIAN_POINT('Ctrl Pts',(1.5,-7.82809570460851,-1.65243333668723));
#43225=CARTESIAN_POINT('Ctrl Pts',(0.,-7.8555650736176,-1.516481345165));
#43226=CARTESIAN_POINT('Ctrl Pts',(1.5,-7.8555650736176,-1.516481345165));
#43227=CARTESIAN_POINT('Ctrl Pts',(0.,-7.8806735237373,-1.38007358893105));
#43228=CARTESIAN_POINT('Ctrl Pts',(1.5,-7.8806735237373,-1.38007358893105));
#43229=CARTESIAN_POINT('Ctrl Pts',(0.,-7.90341350859433,-1.24325106404244));
#43230=CARTESIAN_POINT('Ctrl Pts',(1.5,-7.90341350859433,-1.24325106404244));
#43231=CARTESIAN_POINT('Ctrl Pts',(0.,-7.92377819415291,-1.1060548913017));
#43232=CARTESIAN_POINT('Ctrl Pts',(1.5,-7.92377819415291,-1.1060548913017));
#43233=CARTESIAN_POINT('Ctrl Pts',(0.,-7.94176146025056,-0.968526303816797));
#43234=CARTESIAN_POINT('Ctrl Pts',(1.5,-7.94176146025056,-0.968526303816797));
#43235=CARTESIAN_POINT('Ctrl Pts',(0.,-7.9573579021783,-0.830706634568147));
#43236=CARTESIAN_POINT('Ctrl Pts',(1.5,-7.9573579021783,-0.830706634568147));
#43237=CARTESIAN_POINT('Ctrl Pts',(0.,-7.97056283230563,-0.692637303981898));
#43238=CARTESIAN_POINT('Ctrl Pts',(1.5,-7.97056283230563,-0.692637303981898));
#43239=CARTESIAN_POINT('Ctrl Pts',(0.,-7.98137228175028,-0.55435980750864));
#43240=CARTESIAN_POINT('Ctrl Pts',(1.5,-7.98137228175028,-0.55435980750864));
#43241=CARTESIAN_POINT('Ctrl Pts',(0.,-7.98978300209272,-0.415915703206775));
#43242=CARTESIAN_POINT('Ctrl Pts',(1.5,-7.98978300209272,-0.415915703206775));
#43243=CARTESIAN_POINT('Ctrl Pts',(0.,-7.99579246582898,-0.277346599216242));
#43244=CARTESIAN_POINT('Ctrl Pts',(1.5,-7.99579246582898,-0.277346599216242));
#43245=CARTESIAN_POINT('Ctrl Pts',(0.,-7.99939886686876,-0.138694141235355));
#43246=CARTESIAN_POINT('Ctrl Pts',(1.5,-7.99939886686876,-0.138694141235355));
#43247=CARTESIAN_POINT('Ctrl Pts',(0.,-8.00060112107831,-7.07794283252849E-14));
#43248=CARTESIAN_POINT('Ctrl Pts',(1.5,-8.00060112107831,-7.07794283252849E-14));
#43249=CARTESIAN_POINT('Ctrl Pts',(0.,-7.9993988668687,0.138694141235229));
#43250=CARTESIAN_POINT('Ctrl Pts',(1.5,-7.9993988668687,0.138694141235229));
#43251=CARTESIAN_POINT('Ctrl Pts',(0.,-7.99579246582889,0.277346599216146));
#43252=CARTESIAN_POINT('Ctrl Pts',(1.5,-7.99579246582889,0.277346599216146));
#43253=CARTESIAN_POINT('Ctrl Pts',(0.,-7.98978300209264,0.415915703206705));
#43254=CARTESIAN_POINT('Ctrl Pts',(1.5,-7.98978300209264,0.415915703206705));
#43255=CARTESIAN_POINT('Ctrl Pts',(0.,-7.98137228175027,0.554359807508556));
#43256=CARTESIAN_POINT('Ctrl Pts',(1.5,-7.98137228175027,0.554359807508556));
#43257=CARTESIAN_POINT('Ctrl Pts',(0.,-7.97056283230564,0.692637303981767));
#43258=CARTESIAN_POINT('Ctrl Pts',(1.5,-7.97056283230564,0.692637303981767));
#43259=CARTESIAN_POINT('Ctrl Pts',(0.,-7.95735790217834,0.830706634567969));
#43260=CARTESIAN_POINT('Ctrl Pts',(1.5,-7.95735790217834,0.830706634567969));
#43261=CARTESIAN_POINT('Ctrl Pts',(0.,-7.94176146025064,0.968526303816614));
#43262=CARTESIAN_POINT('Ctrl Pts',(1.5,-7.94176146025064,0.968526303816614));
#43263=CARTESIAN_POINT('Ctrl Pts',(0.,-7.92377819415303,1.10605489130155));
#43264=CARTESIAN_POINT('Ctrl Pts',(1.5,-7.92377819415303,1.10605489130155));
#43265=CARTESIAN_POINT('Ctrl Pts',(0.,-7.90341350859442,1.24325106404233));
#43266=CARTESIAN_POINT('Ctrl Pts',(1.5,-7.90341350859442,1.24325106404233));
#43267=CARTESIAN_POINT('Ctrl Pts',(0.,-7.88067352373733,1.38007358893094));
#43268=CARTESIAN_POINT('Ctrl Pts',(1.5,-7.88067352373733,1.38007358893094));
#43269=CARTESIAN_POINT('Ctrl Pts',(0.,-7.85556507361753,1.51648134516485));
#43270=CARTESIAN_POINT('Ctrl Pts',(1.5,-7.85556507361753,1.51648134516485));
#43271=CARTESIAN_POINT('Ctrl Pts',(0.,-7.8280957046084,1.65243333668702));
#43272=CARTESIAN_POINT('Ctrl Pts',(1.5,-7.8280957046084,1.65243333668702));
#43273=CARTESIAN_POINT('Ctrl Pts',(0.,-7.79827367263774,1.78788870440746));
#43274=CARTESIAN_POINT('Ctrl Pts',(1.5,-7.79827367263774,1.78788870440746));
#43275=CARTESIAN_POINT('Ctrl Pts',(0.,-7.76610794044919,1.92280673843328));
#43276=CARTESIAN_POINT('Ctrl Pts',(1.5,-7.76610794044919,1.92280673843328));
#43277=CARTESIAN_POINT('Ctrl Pts',(0.,-7.73160817490739,2.05714689030813));
#43278=CARTESIAN_POINT('Ctrl Pts',(1.5,-7.73160817490739,2.05714689030813));
#43279=CARTESIAN_POINT('Ctrl Pts',(0.,-7.69478474434738,2.19086878526173));
#43280=CARTESIAN_POINT('Ctrl Pts',(1.5,-7.69478474434738,2.19086878526173));
#43281=CARTESIAN_POINT('Ctrl Pts',(0.,-7.65564871596768,2.32393223447026));
#43282=CARTESIAN_POINT('Ctrl Pts',(1.5,-7.65564871596768,2.32393223447026));
#43283=CARTESIAN_POINT('Ctrl Pts',(0.,-7.61421185199964,2.45629724699104));
#43284=CARTESIAN_POINT('Ctrl Pts',(1.5,-7.61421185199964,2.45629724699104));
#43285=CARTESIAN_POINT('Ctrl Pts',(0.,-7.57048660592016,2.58792404170968));
#43286=CARTESIAN_POINT('Ctrl Pts',(1.5,-7.57048660592016,2.58792404170968));
#43287=CARTESIAN_POINT('Ctrl Pts',(0.,-7.52448611870755,2.71877305930021));
#43288=CARTESIAN_POINT('Ctrl Pts',(1.5,-7.52448611870755,2.71877305930021));
#43289=CARTESIAN_POINT('Ctrl Pts',(0.,-7.47622421514032,2.84880497419911));
#43290=CARTESIAN_POINT('Ctrl Pts',(1.5,-7.47622421514032,2.84880497419911));
#43291=CARTESIAN_POINT('Ctrl Pts',(0.,-7.42571540013867,2.97798070659398));
#43292=CARTESIAN_POINT('Ctrl Pts',(1.5,-7.42571540013867,2.97798070659398));
#43293=CARTESIAN_POINT('Ctrl Pts',(0.,-7.37297485391485,3.10626143398182));
#43294=CARTESIAN_POINT('Ctrl Pts',(1.5,-7.37297485391485,3.10626143398182));
#43295=CARTESIAN_POINT('Ctrl Pts',(0.,-7.31801842716578,3.23360860274336));
#43296=CARTESIAN_POINT('Ctrl Pts',(1.5,-7.31801842716578,3.23360860274336));
#43297=CARTESIAN_POINT('Ctrl Pts',(0.,-7.2608626363076,3.35998393973421));
#43298=CARTESIAN_POINT('Ctrl Pts',(1.5,-7.2608626363076,3.35998393973421));
#43299=CARTESIAN_POINT('Ctrl Pts',(0.,-7.20152465875178,3.48534946389357));
#43300=CARTESIAN_POINT('Ctrl Pts',(1.5,-7.20152465875178,3.48534946389357));
#43301=CARTESIAN_POINT('Ctrl Pts',(0.,-7.14002232822245,3.60966749787115));
#43302=CARTESIAN_POINT('Ctrl Pts',(1.5,-7.14002232822245,3.60966749787115));
#43303=CARTESIAN_POINT('Ctrl Pts',(0.,-7.07637412892443,3.7329006791222));
#43304=CARTESIAN_POINT('Ctrl Pts',(1.5,-7.07637412892443,3.7329006791222));
#43305=CARTESIAN_POINT('Ctrl Pts',(0.,-7.01059918975178,3.8550119710221));
#43306=CARTESIAN_POINT('Ctrl Pts',(1.5,-7.01059918975178,3.8550119710221));
#43307=CARTESIAN_POINT('Ctrl Pts',(0.,-6.94271727853668,3.97596467400145));
#43308=CARTESIAN_POINT('Ctrl Pts',(1.5,-6.94271727853668,3.97596467400145));
#43309=CARTESIAN_POINT('Ctrl Pts',(0.,-6.87274879633835,4.09572243670218));
#43310=CARTESIAN_POINT('Ctrl Pts',(1.5,-6.87274879633835,4.09572243670218));
#43311=CARTESIAN_POINT('Ctrl Pts',(0.,-6.80071477177124,4.21424926715544));
#43312=CARTESIAN_POINT('Ctrl Pts',(1.5,-6.80071477177124,4.21424926715544));
#43313=CARTESIAN_POINT('Ctrl Pts',(0.,-6.7266368542346,4.33150954333015));
#43314=CARTESIAN_POINT('Ctrl Pts',(1.5,-6.7266368542346,4.33150954333015));
#43315=CARTESIAN_POINT('Ctrl Pts',(0.,-6.65053730718051,4.44746802370462));
#43316=CARTESIAN_POINT('Ctrl Pts',(1.5,-6.65053730718051,4.44746802370462));
#43317=CARTESIAN_POINT('Ctrl Pts',(0.,-6.57243900142046,4.56208985786189));
#43318=CARTESIAN_POINT('Ctrl Pts',(1.5,-6.57243900142046,4.56208985786189));
#43319=CARTESIAN_POINT('Ctrl Pts',(0.,-6.49236540846965,4.67534059710945));
#43320=CARTESIAN_POINT('Ctrl Pts',(1.5,-6.49236540846965,4.67534059710945));
#43321=CARTESIAN_POINT('Ctrl Pts',(0.,-6.41034059392897,4.78718620512409));
#43322=CARTESIAN_POINT('Ctrl Pts',(1.5,-6.41034059392897,4.78718620512409));
#43323=CARTESIAN_POINT('Ctrl Pts',(0.,-6.32638920982654,4.89759306787468));
#43324=CARTESIAN_POINT('Ctrl Pts',(1.5,-6.32638920982654,4.89759306787468));
#43325=CARTESIAN_POINT('Ctrl Pts',(0.,-6.2405364869961,5.0065280035713));
#43326=CARTESIAN_POINT('Ctrl Pts',(1.5,-6.2405364869961,5.0065280035713));
#43327=CARTESIAN_POINT('Ctrl Pts',(0.,-6.15280822749117,5.11395827264129));
#43328=CARTESIAN_POINT('Ctrl Pts',(1.5,-6.15280822749117,5.11395827264129));
#43329=CARTESIAN_POINT('Ctrl Pts',(0.,-6.0632307970352,5.21985158773299));
#43330=CARTESIAN_POINT('Ctrl Pts',(1.5,-6.0632307970352,5.21985158773299));
#43331=CARTESIAN_POINT('Ctrl Pts',(0.,-5.97183111750664,5.32417612374773));
#43332=CARTESIAN_POINT('Ctrl Pts',(1.5,-5.97183111750664,5.32417612374773));
#43333=CARTESIAN_POINT('Ctrl Pts',(0.,-5.87863665845037,5.42690052706231));
#43334=CARTESIAN_POINT('Ctrl Pts',(1.5,-5.87863665845037,5.42690052706231));
#43335=CARTESIAN_POINT('Ctrl Pts',(0.,-5.78367542862314,5.52799392478097));
#43336=CARTESIAN_POINT('Ctrl Pts',(1.5,-5.78367542862314,5.52799392478097));
#43337=CARTESIAN_POINT('Ctrl Pts',(0.,-5.68697596757273,5.62742593401721));
#43338=CARTESIAN_POINT('Ctrl Pts',(1.5,-5.68697596757273,5.62742593401721));
#43339=CARTESIAN_POINT('Ctrl Pts',(0.,-5.58856733725033,5.72516667120635));
#43340=CARTESIAN_POINT('Ctrl Pts',(1.5,-5.58856733725033,5.72516667120635));
#43341=CARTESIAN_POINT('Ctrl Pts',(0.,-5.48847911365546,5.82118676144923));
#43342=CARTESIAN_POINT('Ctrl Pts',(1.5,-5.48847911365546,5.82118676144923));
#43343=CARTESIAN_POINT('Ctrl Pts',(0.,-5.38674137758068,5.91545734696517));
#43344=CARTESIAN_POINT('Ctrl Pts',(1.5,-5.38674137758068,5.91545734696517));
#43345=CARTESIAN_POINT('Ctrl Pts',(0.,-5.28338470538786,6.0079500955773));
#43346=CARTESIAN_POINT('Ctrl Pts',(1.5,-5.28338470538786,6.0079500955773));
#43347=CARTESIAN_POINT('Ctrl Pts',(0.,-5.17844015981534,6.09863720923052));
#43348=CARTESIAN_POINT('Ctrl Pts',(1.5,-5.17844015981534,6.09863720923052));
#43349=CARTESIAN_POINT('Ctrl Pts',(0.,-5.07193928081565,6.18749143254302));
#43350=CARTESIAN_POINT('Ctrl Pts',(1.5,-5.07193928081565,6.18749143254302));
#43351=CARTESIAN_POINT('Ctrl Pts',(0.,-4.96391407642283,6.27448606139153));
#43352=CARTESIAN_POINT('Ctrl Pts',(1.5,-4.96391407642283,6.27448606139153));
#43353=CARTESIAN_POINT('Ctrl Pts',(0.,-4.85439701280011,6.35959495053125));
#43354=CARTESIAN_POINT('Ctrl Pts',(1.5,-4.85439701280011,6.35959495053125));
#43355=CARTESIAN_POINT('Ctrl Pts',(0.,-4.74342100431631,6.44279252125077));
#43356=CARTESIAN_POINT('Ctrl Pts',(1.5,-4.74342100431631,6.44279252125077));
#43357=CARTESIAN_POINT('Ctrl Pts',(0.,-4.63101940365009,6.52405376906226));
#43358=CARTESIAN_POINT('Ctrl Pts',(1.5,-4.63101940365009,6.52405376906226));
#43359=CARTESIAN_POINT('Ctrl Pts',(0.,-4.51722599192163,6.60335427142766));
#43360=CARTESIAN_POINT('Ctrl Pts',(1.5,-4.51722599192163,6.60335427142766));
#43361=CARTESIAN_POINT('Ctrl Pts',(0.,-4.40207496885094,6.68067019552094));
#43362=CARTESIAN_POINT('Ctrl Pts',(1.5,-4.40207496885094,6.68067019552094));
#43363=CARTESIAN_POINT('Ctrl Pts',(0.,-4.28560094218339,6.75597830495801));
#43364=CARTESIAN_POINT('Ctrl Pts',(1.5,-4.28560094218339,6.75597830495801));
#43365=CARTESIAN_POINT('Ctrl Pts',(0.,-4.16783891714045,6.82925596656362));
#43366=CARTESIAN_POINT('Ctrl Pts',(1.5,-4.16783891714045,6.82925596656362));
#43367=CARTESIAN_POINT('Ctrl Pts',(0.,-4.04882428589543,6.90048115717614));
#43368=CARTESIAN_POINT('Ctrl Pts',(1.5,-4.04882428589543,6.90048115717614));
#43369=CARTESIAN_POINT('Ctrl Pts',(0.,-3.92859281707335,6.96963247049021));
#43370=CARTESIAN_POINT('Ctrl Pts',(1.5,-3.92859281707335,6.96963247049021));
#43371=CARTESIAN_POINT('Ctrl Pts',(0.,-3.80718064527426,7.03668912393813));
#43372=CARTESIAN_POINT('Ctrl Pts',(1.5,-3.80718064527426,7.03668912393813));
#43373=CARTESIAN_POINT('Ctrl Pts',(0.,-3.68462425995581,7.10163096447878));
#43374=CARTESIAN_POINT('Ctrl Pts',(1.5,-3.68462425995581,7.10163096447878));
#43375=CARTESIAN_POINT('Ctrl Pts',(0.,-3.56096049433769,7.16443847442598));
#43376=CARTESIAN_POINT('Ctrl Pts',(1.5,-3.56096049433769,7.16443847442598));
#43377=CARTESIAN_POINT('Ctrl Pts',(0.,-3.43622651432787,7.22509277731633));
#43378=CARTESIAN_POINT('Ctrl Pts',(1.5,-3.43622651432787,7.22509277731633));
#43379=CARTESIAN_POINT('Ctrl Pts',(0.,-3.31045980746936,7.28357564381742));
#43380=CARTESIAN_POINT('Ctrl Pts',(1.5,-3.31045980746936,7.28357564381742));
#43381=CARTESIAN_POINT('Ctrl Pts',(0.,-3.18369817190718,7.33986949767594));
#43382=CARTESIAN_POINT('Ctrl Pts',(1.5,-3.18369817190718,7.33986949767594));
#43383=CARTESIAN_POINT('Ctrl Pts',(0.,-3.05597970481146,7.39395742052271));
#43384=CARTESIAN_POINT('Ctrl Pts',(1.5,-3.05597970481146,7.39395742052271));
#43385=CARTESIAN_POINT('Ctrl Pts',(0.,-2.92734279081915,7.44582315671858));
#43386=CARTESIAN_POINT('Ctrl Pts',(1.5,-2.92734279081915,7.44582315671858));
#43387=CARTESIAN_POINT('Ctrl Pts',(0.,-2.7978260904937,7.49545111824188));
#43388=CARTESIAN_POINT('Ctrl Pts',(1.5,-2.7978260904937,7.49545111824188));
#43389=CARTESIAN_POINT('Ctrl Pts',(0.,-2.66746852880196,7.54282638961738));
#43390=CARTESIAN_POINT('Ctrl Pts',(1.5,-2.66746852880196,7.54282638961738));
#43391=CARTESIAN_POINT('Ctrl Pts',(0.,-2.53630928360749,7.58793473288732));
#43392=CARTESIAN_POINT('Ctrl Pts',(1.5,-2.53630928360749,7.58793473288732));
#43393=CARTESIAN_POINT('Ctrl Pts',(0.,-2.40438777372116,7.63076259139572));
#43394=CARTESIAN_POINT('Ctrl Pts',(1.5,-2.40438777372116,7.63076259139572));
#43395=CARTESIAN_POINT('Ctrl Pts',(0.,-2.27174364696667,7.6712970936152));
#43396=CARTESIAN_POINT('Ctrl Pts',(1.5,-2.27174364696667,7.6712970936152));
#43397=CARTESIAN_POINT('Ctrl Pts',(0.,-2.13841676826048,7.70952605701664));
#43398=CARTESIAN_POINT('Ctrl Pts',(1.5,-2.13841676826048,7.70952605701664));
#43399=CARTESIAN_POINT('Ctrl Pts',(0.,-2.00444720770517,7.7454379919818));
#43400=CARTESIAN_POINT('Ctrl Pts',(1.5,-2.00444720770517,7.7454379919818));
#43401=CARTESIAN_POINT('Ctrl Pts',(0.,-1.86987522869577,7.77902210575933));
#43402=CARTESIAN_POINT('Ctrl Pts',(1.5,-1.86987522869577,7.77902210575933));
#43403=CARTESIAN_POINT('Ctrl Pts',(0.,-1.73474127568748,7.81026830520089));
#43404=CARTESIAN_POINT('Ctrl Pts',(1.5,-1.73474127568748,7.81026830520089));
#43405=CARTESIAN_POINT('Ctrl Pts',(0.,-1.59908596197483,7.83916719954116));
#43406=CARTESIAN_POINT('Ctrl Pts',(1.5,-1.59908596197483,7.83916719954116));
#43407=CARTESIAN_POINT('Ctrl Pts',(0.,-1.46295005748132,7.86571010322159));
#43408=CARTESIAN_POINT('Ctrl Pts',(1.5,-1.46295005748132,7.86571010322159));
#43409=CARTESIAN_POINT('Ctrl Pts',(0.,-1.32637447655881,7.88988903875827));
#43410=CARTESIAN_POINT('Ctrl Pts',(1.5,-1.32637447655881,7.88988903875827));
#43411=CARTESIAN_POINT('Ctrl Pts',(0.,-1.18940026579592,7.91169673965388));
#43412=CARTESIAN_POINT('Ctrl Pts',(1.5,-1.18940026579592,7.91169673965388));
#43413=CARTESIAN_POINT('Ctrl Pts',(0.,-1.0520685915949,7.93112665206312));
#43414=CARTESIAN_POINT('Ctrl Pts',(1.5,-1.0520685915949,7.93112665206312));
#43415=CARTESIAN_POINT('Ctrl Pts',(0.,-0.914420727755818,7.94817293650282));
#43416=CARTESIAN_POINT('Ctrl Pts',(1.5,-0.914420727755818,7.94817293650282));
#43417=CARTESIAN_POINT('Ctrl Pts',(0.,-0.776498043067579,7.96283046960651));
#43418=CARTESIAN_POINT('Ctrl Pts',(1.5,-0.776498043067579,7.96283046960651));
#43419=CARTESIAN_POINT('Ctrl Pts',(0.,-0.6383419889048,7.97509484592382));
#43420=CARTESIAN_POINT('Ctrl Pts',(1.5,-0.6383419889048,7.97509484592382));
#43421=CARTESIAN_POINT('Ctrl Pts',(0.,-0.49999408682987,7.98496237976457));
#43422=CARTESIAN_POINT('Ctrl Pts',(1.5,-0.49999408682987,7.98496237976457));
#43423=CARTESIAN_POINT('Ctrl Pts',(0.,-0.361495916072309,7.99243010578594));
#43424=CARTESIAN_POINT('Ctrl Pts',(1.5,-0.361495916072309,7.99243010578594));
#43425=CARTESIAN_POINT('Ctrl Pts',(0.,-0.222889101011755,7.99749577962464));
#43426=CARTESIAN_POINT('Ctrl Pts',(1.5,-0.222889101011755,7.99749577962464));
#43427=CARTESIAN_POINT('Ctrl Pts',(0.,-0.0842152986637398,8.00015787857408));
#43428=CARTESIAN_POINT('Ctrl Pts',(1.5,-0.0842152986637398,8.00015787857408));
#43429=CARTESIAN_POINT('Ctrl Pts',(0.,0.0544838138324916,8.0004156023065));
#43430=CARTESIAN_POINT('Ctrl Pts',(1.5,0.0544838138324916,8.0004156023065));
#43431=CARTESIAN_POINT('Ctrl Pts',(0.,0.19316655172488,7.99826887364025));
#43432=CARTESIAN_POINT('Ctrl Pts',(1.5,0.19316655172488,7.99826887364025));
#43433=CARTESIAN_POINT('Ctrl Pts',(0.,0.331791235173336,7.99371833803291));
#43434=CARTESIAN_POINT('Ctrl Pts',(1.5,0.331791235173336,7.99371833803291));
#43435=CARTESIAN_POINT('Ctrl Pts',(0.,0.470316201774787,7.98676536311949));
#43436=CARTESIAN_POINT('Ctrl Pts',(1.5,0.470316201774787,7.98676536311949));
#43437=CARTESIAN_POINT('Ctrl Pts',(0.,0.608699819089367,7.97741203829577));
#43438=CARTESIAN_POINT('Ctrl Pts',(1.5,0.608699819089367,7.97741203829577));
#43439=CARTESIAN_POINT('Ctrl Pts',(0.,0.746900497168441,7.96566117434659));
#43440=CARTESIAN_POINT('Ctrl Pts',(1.5,0.746900497168441,7.96566117434659));
#43441=CARTESIAN_POINT('Ctrl Pts',(0.,0.884876701085331,7.95151630311944));
#43442=CARTESIAN_POINT('Ctrl Pts',(1.5,0.884876701085331,7.95151630311944));
#43443=CARTESIAN_POINT('Ctrl Pts',(0.,1.02258696336839,7.9349816759534));
#43444=CARTESIAN_POINT('Ctrl Pts',(1.5,1.02258696336839,7.9349816759534));
#43445=CARTESIAN_POINT('Ctrl Pts',(0.,1.15998989643833,7.9160622621531));
#43446=CARTESIAN_POINT('Ctrl Pts',(1.5,1.15998989643833,7.9160622621531));
#43447=CARTESIAN_POINT('Ctrl Pts',(0.,1.2970442050506,7.89476374750747));
#43448=CARTESIAN_POINT('Ctrl Pts',(1.5,1.2970442050506,7.89476374750747));
#43449=CARTESIAN_POINT('Ctrl Pts',(0.,1.43370869874345,7.87109253285326));
#43450=CARTESIAN_POINT('Ctrl Pts',(1.5,1.43370869874345,7.87109253285326));
#43451=CARTESIAN_POINT('Ctrl Pts',(0.,1.56994230429259,7.84505573268319));
#43452=CARTESIAN_POINT('Ctrl Pts',(1.5,1.56994230429259,7.84505573268319));
#43453=CARTESIAN_POINT('Ctrl Pts',(0.,1.70570407796333,7.81666117246187));
#43454=CARTESIAN_POINT('Ctrl Pts',(1.5,1.70570407796333,7.81666117246187));
#43455=CARTESIAN_POINT('Ctrl Pts',(0.,1.84095321777081,7.78591738598617));
#43456=CARTESIAN_POINT('Ctrl Pts',(1.5,1.84095321777081,7.78591738598617));
#43457=CARTESIAN_POINT('Ctrl Pts',(0.,1.97564907574906,7.75283361278995));
#43458=CARTESIAN_POINT('Ctrl Pts',(1.5,1.97564907574906,7.75283361278995));
#43459=CARTESIAN_POINT('Ctrl Pts',(0.,2.10975117022968,7.71741979559267));
#43460=CARTESIAN_POINT('Ctrl Pts',(1.5,2.10975117022968,7.71741979559267));
#43461=CARTESIAN_POINT('Ctrl Pts',(0.,2.24321919813091,7.67968657779199));
#43462=CARTESIAN_POINT('Ctrl Pts',(1.5,2.24321919813091,7.67968657779199));
#43463=CARTESIAN_POINT('Ctrl Pts',(0.,2.37601304692748,7.63964529982795));
#43464=CARTESIAN_POINT('Ctrl Pts',(1.5,2.37601304692748,7.63964529982795));
#43465=CARTESIAN_POINT('Ctrl Pts',(0.,2.50809280663236,7.59730799559073));
#43466=CARTESIAN_POINT('Ctrl Pts',(1.5,2.50809280663236,7.59730799559073));
#43467=CARTESIAN_POINT('Ctrl Pts',(0.,2.63941878179114,7.55268738887154));
#43468=CARTESIAN_POINT('Ctrl Pts',(1.5,2.63941878179114,7.55268738887154));
#43469=CARTESIAN_POINT('Ctrl Pts',(0.,2.76995150348982,7.50579688985671));
#43470=CARTESIAN_POINT('Ctrl Pts',(1.5,2.76995150348982,7.50579688985671));
#43471=CARTESIAN_POINT('Ctrl Pts',(0.,2.89965174137675,7.45665059166464));
#43472=CARTESIAN_POINT('Ctrl Pts',(1.5,2.89965174137675,7.45665059166464));
#43473=CARTESIAN_POINT('Ctrl Pts',(0.,3.02848051528187,7.40526326545791));
#43474=CARTESIAN_POINT('Ctrl Pts',(1.5,3.02848051528187,7.40526326545791));
#43475=CARTESIAN_POINT('Ctrl Pts',(0.,3.15639910685162,7.35165035559758));
#43476=CARTESIAN_POINT('Ctrl Pts',(1.5,3.15639910685162,7.35165035559758));
#43477=CARTESIAN_POINT('Ctrl Pts',(0.,3.28336907120013,7.29582797483965));
#43478=CARTESIAN_POINT('Ctrl Pts',(1.5,3.28336907120013,7.29582797483965));
#43479=CARTESIAN_POINT('Ctrl Pts',(0.,3.4093522485776,7.23781289957331));
#43480=CARTESIAN_POINT('Ctrl Pts',(1.5,3.4093522485776,7.23781289957331));
#43481=CARTESIAN_POINT('Ctrl Pts',(0.,3.5343107760563,7.17762256510045));
#43482=CARTESIAN_POINT('Ctrl Pts',(1.5,3.5343107760563,7.17762256510045));
#43483=CARTESIAN_POINT('Ctrl Pts',(0.,3.65820709866192,7.1152750602933));
#43484=CARTESIAN_POINT('Ctrl Pts',(1.5,3.65820709866192,7.1152750602933));
#43485=CARTESIAN_POINT('Ctrl Pts',(0.,3.78100398052407,7.05078912229265));
#43486=CARTESIAN_POINT('Ctrl Pts',(1.5,3.78100398052407,7.05078912229265));
#43487=CARTESIAN_POINT('Ctrl Pts',(0.,3.90266451604675,6.98418413124666));
#43488=CARTESIAN_POINT('Ctrl Pts',(1.5,3.90266451604675,6.98418413124666));
#43489=CARTESIAN_POINT('Ctrl Pts',(0.,4.02315214109941,6.91548010508983));
#43490=CARTESIAN_POINT('Ctrl Pts',(1.5,4.02315214109941,6.91548010508983));
#43491=CARTESIAN_POINT('Ctrl Pts',(0.,4.14243064422928,6.84469769436163));
#43492=CARTESIAN_POINT('Ctrl Pts',(1.5,4.14243064422928,6.84469769436163));
#43493=CARTESIAN_POINT('Ctrl Pts',(0.,4.26046417733762,6.77185817468256));
#43494=CARTESIAN_POINT('Ctrl Pts',(1.5,4.26046417733762,6.77185817468256));
#43495=CARTESIAN_POINT('Ctrl Pts',(0.,4.37721726637856,6.69698343926911));
#43496=CARTESIAN_POINT('Ctrl Pts',(1.5,4.37721726637856,6.69698343926911));
#43497=CARTESIAN_POINT('Ctrl Pts',(0.,4.4926548220813,6.62009599148732));
#43498=CARTESIAN_POINT('Ctrl Pts',(1.5,4.4926548220813,6.62009599148732));
#43499=CARTESIAN_POINT('Ctrl Pts',(0.,4.60674215069637,6.54121893744448));
#43500=CARTESIAN_POINT('Ctrl Pts',(1.5,4.60674215069637,6.54121893744448));
#43501=CARTESIAN_POINT('Ctrl Pts',(0.,4.71944496476657,6.46037597861856));
#43502=CARTESIAN_POINT('Ctrl Pts',(1.5,4.71944496476657,6.46037597861856));
#43503=CARTESIAN_POINT('Ctrl Pts',(0.,4.83072939299739,6.37759140631321));
#43504=CARTESIAN_POINT('Ctrl Pts',(1.5,4.83072939299739,6.37759140631321));
#43505=CARTESIAN_POINT('Ctrl Pts',(0.,4.9405619901535,6.29289009614967));
#43506=CARTESIAN_POINT('Ctrl Pts',(1.5,4.9405619901535,6.29289009614967));
#43507=CARTESIAN_POINT('Ctrl Pts',(0.,5.04890974698171,6.20629750259518));
#43508=CARTESIAN_POINT('Ctrl Pts',(1.5,5.04890974698171,6.20629750259518));
#43509=CARTESIAN_POINT('Ctrl Pts',(0.,5.15574010016135,6.11783965352734));
#43510=CARTESIAN_POINT('Ctrl Pts',(1.5,5.15574010016135,6.11783965352734));
#43511=CARTESIAN_POINT('Ctrl Pts',(0.,5.26102094228238,6.02754314483433));
#43512=CARTESIAN_POINT('Ctrl Pts',(1.5,5.26102094228238,6.02754314483433));
#43513=CARTESIAN_POINT('Ctrl Pts',(0.,5.36472063146403,5.93543512735866));
#43514=CARTESIAN_POINT('Ctrl Pts',(1.5,5.36472063146403,5.93543512735866));
#43515=CARTESIAN_POINT('Ctrl Pts',(0.,5.46680800100264,5.84154329387568));
#43516=CARTESIAN_POINT('Ctrl Pts',(1.5,5.46680800100264,5.84154329387568));
#43517=CARTESIAN_POINT('Ctrl Pts',(0.,5.56725236904908,5.74589586610586));
#43518=CARTESIAN_POINT('Ctrl Pts',(1.5,5.56725236904908,5.74589586610586));
#43519=CARTESIAN_POINT('Ctrl Pts',(0.,5.66602354831653,5.64852158176032));
#43520=CARTESIAN_POINT('Ctrl Pts',(1.5,5.66602354831653,5.64852158176032));
#43521=CARTESIAN_POINT('Ctrl Pts',(0.,5.76309185581898,5.54944968161887));
#43522=CARTESIAN_POINT('Ctrl Pts',(1.5,5.76309185581898,5.54944968161887));
#43523=CARTESIAN_POINT('Ctrl Pts',(0.,5.85842812070729,5.44870991119888));
#43524=CARTESIAN_POINT('Ctrl Pts',(1.5,5.85842812070729,5.44870991119888));
#43525=CARTESIAN_POINT('Ctrl Pts',(0.,5.95200369213706,5.34633252245584));
#43526=CARTESIAN_POINT('Ctrl Pts',(1.5,5.95200369213706,5.34633252245584));
#43527=CARTESIAN_POINT('Ctrl Pts',(0.,6.04379044716914,5.24234827551538));
#43528=CARTESIAN_POINT('Ctrl Pts',(1.5,6.04379044716914,5.24234827551538));
#43529=CARTESIAN_POINT('Ctrl Pts',(0.,6.13376079870296,5.13678844043658));
#43530=CARTESIAN_POINT('Ctrl Pts',(1.5,6.13376079870296,5.13678844043658));
#43531=CARTESIAN_POINT('Ctrl Pts',(0.,6.22188770344349,5.02968479900663));
#43532=CARTESIAN_POINT('Ctrl Pts',(1.5,6.22188770344349,5.02968479900663));
#43533=CARTESIAN_POINT('Ctrl Pts',(0.,6.30814467128367,4.92106960970541));
#43534=CARTESIAN_POINT('Ctrl Pts',(1.5,6.30814467128367,4.92106960970541));
#43535=CARTESIAN_POINT('Ctrl Pts',(0.,6.39250577472143,4.81097557269961));
#43536=CARTESIAN_POINT('Ctrl Pts',(1.5,6.39250577472143,4.81097557269961));
#43537=CARTESIAN_POINT('Ctrl Pts',(0.,6.47494565831174,4.6994357948647));
#43538=CARTESIAN_POINT('Ctrl Pts',(1.5,6.47494565831174,4.6994357948647));
#43539=CARTESIAN_POINT('Ctrl Pts',(0.,6.55543954815451,4.58648375483325));
#43540=CARTESIAN_POINT('Ctrl Pts',(1.5,6.55543954815451,4.58648375483325));
#43541=CARTESIAN_POINT('Ctrl Pts',(0.,6.63396326141842,4.47215326806801));
#43542=CARTESIAN_POINT('Ctrl Pts',(1.5,6.63396326141842,4.47215326806801));
#43543=CARTESIAN_POINT('Ctrl Pts',(0.,6.71049320933066,4.3564785348024));
#43544=CARTESIAN_POINT('Ctrl Pts',(1.5,6.71049320933066,4.3564785348024));
#43545=CARTESIAN_POINT('Ctrl Pts',(0.,6.7850064002035,4.23949418800588));
#43546=CARTESIAN_POINT('Ctrl Pts',(1.5,6.7850064002035,4.23949418800588));
#43547=CARTESIAN_POINT('Ctrl Pts',(0.,6.85748044249833,4.1212353413755));
#43548=CARTESIAN_POINT('Ctrl Pts',(1.5,6.85748044249833,4.1212353413755));
#43549=CARTESIAN_POINT('Ctrl Pts',(0.,6.92789354792729,4.00173763735536));
#43550=CARTESIAN_POINT('Ctrl Pts',(1.5,6.92789354792729,4.00173763735536));
#43551=CARTESIAN_POINT('Ctrl Pts',(0.,6.99622453459269,3.88103729518557));
#43552=CARTESIAN_POINT('Ctrl Pts',(1.5,6.99622453459269,3.88103729518557));
#43553=CARTESIAN_POINT('Ctrl Pts',(0.,7.06245284183707,3.75917096410964));
#43554=CARTESIAN_POINT('Ctrl Pts',(1.5,7.06245284183707,3.75917096410964));
#43555=CARTESIAN_POINT('Ctrl Pts',(0.,7.12655854513193,3.63617557660714));
#43556=CARTESIAN_POINT('Ctrl Pts',(1.5,7.12655854513193,3.63617557660714));
#43557=CARTESIAN_POINT('Ctrl Pts',(0.,7.18852237100618,3.51208820164565));
#43558=CARTESIAN_POINT('Ctrl Pts',(1.5,7.18852237100618,3.51208820164565));
#43559=CARTESIAN_POINT('Ctrl Pts',(0.,7.24832571201498,3.38694589794629));
#43560=CARTESIAN_POINT('Ctrl Pts',(1.5,7.24832571201498,3.38694589794629));
#43561=CARTESIAN_POINT('Ctrl Pts',(0.,7.30595064174937,3.26078556725682));
#43562=CARTESIAN_POINT('Ctrl Pts',(1.5,7.30595064174937,3.26078556725682));
#43563=CARTESIAN_POINT('Ctrl Pts',(0.,7.36137989899042,3.1336442580578));
#43564=CARTESIAN_POINT('Ctrl Pts',(1.5,7.36137989899042,3.1336442580578));
#43565=CARTESIAN_POINT('Ctrl Pts',(0.,7.41459687190452,3.00555946928163));
#43566=CARTESIAN_POINT('Ctrl Pts',(1.5,7.41459687190452,3.00555946928163));
#43567=CARTESIAN_POINT('Ctrl Pts',(0.,7.4655855822794,2.87656945405601));
#43568=CARTESIAN_POINT('Ctrl Pts',(1.5,7.4655855822794,2.87656945405601));
#43569=CARTESIAN_POINT('Ctrl Pts',(0.,7.51433066980066,2.74671352348252));
#43570=CARTESIAN_POINT('Ctrl Pts',(1.5,7.51433066980066,2.74671352348252));
#43571=CARTESIAN_POINT('Ctrl Pts',(0.,7.56081737636802,2.61603235046252));
#43572=CARTESIAN_POINT('Ctrl Pts',(1.5,7.56081737636802,2.61603235046252));
#43573=CARTESIAN_POINT('Ctrl Pts',(0.,7.60503159823037,2.48456722613382));
#43574=CARTESIAN_POINT('Ctrl Pts',(1.5,7.60503159823037,2.48456722613382));
#43575=CARTESIAN_POINT('Ctrl Pts',(0.,7.64695993816224,2.35235931633758));
#43576=CARTESIAN_POINT('Ctrl Pts',(1.5,7.64695993816224,2.35235931633758));
#43577=CARTESIAN_POINT('Ctrl Pts',(0.,7.68658975768392,2.21944891808583));
#43578=CARTESIAN_POINT('Ctrl Pts',(1.5,7.68658975768392,2.21944891808583));
#43579=CARTESIAN_POINT('Ctrl Pts',(0.,7.72390922932699,2.0858747160024));
#43580=CARTESIAN_POINT('Ctrl Pts',(1.5,7.72390922932699,2.0858747160024));
#43581=CARTESIAN_POINT('Ctrl Pts',(0.,7.7589073889478,1.95167303870691));
#43582=CARTESIAN_POINT('Ctrl Pts',(1.5,7.7589073889478,1.95167303870691));
#43583=CARTESIAN_POINT('Ctrl Pts',(0.,7.79157402704055,1.81687953471803));
#43584=CARTESIAN_POINT('Ctrl Pts',(1.5,7.79157402704055,1.81687953471803));
#43585=CARTESIAN_POINT('Ctrl Pts',(0.,7.8218995800964,1.68153084833423));
#43586=CARTESIAN_POINT('Ctrl Pts',(1.5,7.8218995800964,1.68153084833423));
#43587=CARTESIAN_POINT('Ctrl Pts',(0.,7.84987502200416,1.54566629555745));
#43588=CARTESIAN_POINT('Ctrl Pts',(1.5,7.84987502200416,1.54566629555745));
#43589=CARTESIAN_POINT('Ctrl Pts',(0.,7.87549175548865,1.40932954012019));
#43590=CARTESIAN_POINT('Ctrl Pts',(1.5,7.87549175548865,1.40932954012019));
#43591=CARTESIAN_POINT('Ctrl Pts',(0.,7.89874150358258,1.27257026968328));
#43592=CARTESIAN_POINT('Ctrl Pts',(1.5,7.89874150358258,1.27257026968328));
#43593=CARTESIAN_POINT('Ctrl Pts',(0.,7.91961655999428,1.13544052228966));
#43594=CARTESIAN_POINT('Ctrl Pts',(1.5,7.91961655999428,1.13544052228966));
#43595=CARTESIAN_POINT('Ctrl Pts',(0.,7.93811003951429,0.99799101291279));
#43596=CARTESIAN_POINT('Ctrl Pts',(1.5,7.93811003951429,0.99799101291279));
#43597=CARTESIAN_POINT('Ctrl Pts',(0.,7.95421612847067,0.860267459956574));
#43598=CARTESIAN_POINT('Ctrl Pts',(1.5,7.95421612847067,0.860267459956574));
#43599=CARTESIAN_POINT('Ctrl Pts',(0.,7.96793033524234,0.722306911570933));
#43600=CARTESIAN_POINT('Ctrl Pts',(1.5,7.96793033524234,0.722306911570933));
#43601=CARTESIAN_POINT('Ctrl Pts',(0.,7.97924974084015,0.584134071639387));
#43602=CARTESIAN_POINT('Ctrl Pts',(1.5,7.97924974084015,0.584134071639387));
#43603=CARTESIAN_POINT('Ctrl Pts',(0.,7.988172666211,0.445763767776282));
#43604=CARTESIAN_POINT('Ctrl Pts',(1.5,7.988172666211,0.445763767776282));
#43605=CARTESIAN_POINT('Ctrl Pts',(0.,7.99339320492744,0.334915488715433));
#43606=CARTESIAN_POINT('Ctrl Pts',(1.5,7.99339320492744,0.334915488715433));
#43607=CARTESIAN_POINT('Ctrl Pts',(0.,7.9962297569157,0.251694874137988));
#43608=CARTESIAN_POINT('Ctrl Pts',(1.5,7.9962297569157,0.251694874137988));
#43609=CARTESIAN_POINT('Ctrl Pts',(0.,7.99764130779673,0.196176951432127));
#43610=CARTESIAN_POINT('Ctrl Pts',(1.5,7.99764130779673,0.196176951432127));
#43611=CARTESIAN_POINT('Ctrl Pts',(0.,7.99822721229278,0.168408611832292));
#43612=CARTESIAN_POINT('Ctrl Pts',(1.5,7.99822721229278,0.168408611832292));
#43613=CARTESIAN_POINT('',(0.15,7.99822721229278,0.168408611832292));
#43614=CARTESIAN_POINT('Ctrl Pts',(0.15,7.99822721229278,0.168408611832292));
#43615=CARTESIAN_POINT('Ctrl Pts',(0.15,7.9668162212544,1.6571001514885));
#43616=CARTESIAN_POINT('Ctrl Pts',(0.15,7.05454066693418,4.60748407596604));
#43617=CARTESIAN_POINT('Ctrl Pts',(0.15,3.54676252795573,7.6458195669611));
#43618=CARTESIAN_POINT('Ctrl Pts',(0.15,-1.03566271747928,8.36163178448781));
#43619=CARTESIAN_POINT('Ctrl Pts',(0.15,-5.30396918600683,6.54797121169431));
#43620=CARTESIAN_POINT('Ctrl Pts',(0.15,-7.96648062384354,2.74828140568407));
#43621=CARTESIAN_POINT('Ctrl Pts',(0.15,-8.19387712094983,-1.54631831555544));
#43622=CARTESIAN_POINT('Ctrl Pts',(0.15,-6.51467119594908,-5.07412386813192));
#43623=CARTESIAN_POINT('Ctrl Pts',(0.15,-3.76134237152816,-7.35225187872476));
#43624=CARTESIAN_POINT('Ctrl Pts',(0.15,-0.301346652009213,-8.25272087673402));
#43625=CARTESIAN_POINT('Ctrl Pts',(0.15,3.21364811100624,-7.60713764510347));
#43626=CARTESIAN_POINT('Ctrl Pts',(0.15,6.12799056084021,-5.53596483741694));
#43627=CARTESIAN_POINT('Ctrl Pts',(0.15,7.42100104272284,-3.25862403370716));
#43628=CARTESIAN_POINT('Ctrl Pts',(0.15,7.90104362420642,-1.41473238843176));
#43629=CARTESIAN_POINT('Ctrl Pts',(0.15,7.98748469629358,-0.677499195126446));
#43630=CARTESIAN_POINT('Ctrl Pts',(0.15,7.99822707315249,-0.168415205726119));
#43631=CARTESIAN_POINT('',(0.,7.99822721229278,0.168408611832292));
#43632=CARTESIAN_POINT('Ctrl Pts',(0.15,7.99822735142219,-0.168402017937099));
#43633=CARTESIAN_POINT('Ctrl Pts',(0.15,7.98748572261181,-0.677490441897062));
#43634=CARTESIAN_POINT('Ctrl Pts',(0.15,7.90104473181587,-1.41472813399292));
#43635=CARTESIAN_POINT('Ctrl Pts',(0.15,7.42100104272284,-3.25862403370716));
#43636=CARTESIAN_POINT('Ctrl Pts',(0.15,6.12799056084021,-5.53596483741694));
#43637=CARTESIAN_POINT('Ctrl Pts',(0.15,3.21364811100624,-7.60713764510347));
#43638=CARTESIAN_POINT('Ctrl Pts',(0.15,-0.301346652009213,-8.25272087673402));
#43639=CARTESIAN_POINT('Ctrl Pts',(0.15,-3.76134237152816,-7.35225187872476));
#43640=CARTESIAN_POINT('Ctrl Pts',(0.15,-6.51467119594908,-5.07412386813192));
#43641=CARTESIAN_POINT('Ctrl Pts',(0.15,-8.19387712094983,-1.54631831555544));
#43642=CARTESIAN_POINT('Ctrl Pts',(0.15,-7.96648062384354,2.74828140568407));
#43643=CARTESIAN_POINT('Ctrl Pts',(0.15,-5.30396918600683,6.54797121169431));
#43644=CARTESIAN_POINT('Ctrl Pts',(0.15,-1.03566271747928,8.36163178448781));
#43645=CARTESIAN_POINT('Ctrl Pts',(0.15,3.54676252795573,7.6458195669611));
#43646=CARTESIAN_POINT('Ctrl Pts',(0.15,7.05454066693418,4.60748407596604));
#43647=CARTESIAN_POINT('Ctrl Pts',(0.15,7.9668162212544,1.6571001514885));
#43648=CARTESIAN_POINT('Ctrl Pts',(0.15,7.99822721229278,0.168408611832292));
#43649=CARTESIAN_POINT('Ctrl Pts',(0.1,8.04821622517087,-0.169456769727133));
#43650=CARTESIAN_POINT('Ctrl Pts',(0.1,8.03741002472644,-0.681720507360159));
#43651=CARTESIAN_POINT('Ctrl Pts',(0.1,7.95042407944463,-1.42356971720002));
#43652=CARTESIAN_POINT('Ctrl Pts',(0.1,7.46738625004804,-3.2789905004189));
#43653=CARTESIAN_POINT('Ctrl Pts',(0.1,6.16628997740278,-5.57056470636502));
#43654=CARTESIAN_POINT('Ctrl Pts',(0.1,3.23373517685434,-7.65468305150081));
#43655=CARTESIAN_POINT('Ctrl Pts',(0.1,-0.303229672299122,-8.30429995047224));
#43656=CARTESIAN_POINT('Ctrl Pts',(0.1,-3.7848514261649,-7.39820381482444));
#43657=CARTESIAN_POINT('Ctrl Pts',(0.1,-6.55538636377591,-5.10583648537583));
#43658=CARTESIAN_POINT('Ctrl Pts',(0.1,-8.24508930199638,-1.55598312295372));
#43659=CARTESIAN_POINT('Ctrl Pts',(0.1,-8.01627176717492,2.76545880984833));
#43660=CARTESIAN_POINT('Ctrl Pts',(0.1,-5.33711785417695,6.58889573792462));
#43661=CARTESIAN_POINT('Ctrl Pts',(0.1,-1.04213746891484,8.41389837754811));
#43662=CARTESIAN_POINT('Ctrl Pts',(0.1,3.56893478939425,7.69359494724594));
#43663=CARTESIAN_POINT('Ctrl Pts',(0.1,7.09862217307051,4.63628718819819));
#43664=CARTESIAN_POINT('Ctrl Pts',(0.1,8.01662992354949,1.6674436985376));
#43665=CARTESIAN_POINT('Ctrl Pts',(0.1,8.04821608604147,0.169463363621706));
#43666=CARTESIAN_POINT('Ctrl Pts',(0.05,8.09820509891955,-0.170511521517167));
#43667=CARTESIAN_POINT('Ctrl Pts',(0.0499999999999999,8.08752804174321,
-0.676424631804066));
#43668=CARTESIAN_POINT('Ctrl Pts',(0.05,7.99982927879915,-1.43151013980792));
#43669=CARTESIAN_POINT('Ctrl Pts',(0.0499999999999999,7.51385392106967,
-3.2948434841773));
#43670=CARTESIAN_POINT('Ctrl Pts',(0.0500000000000001,6.20457757618847,
-5.60581111430041));
#43671=CARTESIAN_POINT('Ctrl Pts',(0.0499999999999999,3.25384581479248,
-7.70084002943972));
#43672=CARTESIAN_POINT('Ctrl Pts',(0.05,-0.305119682800658,-8.35615970982999));
#43673=CARTESIAN_POINT('Ctrl Pts',(0.05,-3.80835338172119,-7.44390937025256));
#43674=CARTESIAN_POINT('Ctrl Pts',(0.05,-6.59610752261337,-5.13761912738161));
#43675=CARTESIAN_POINT('Ctrl Pts',(0.05,-8.29629911008737,-1.56559713102122));
#43676=CARTESIAN_POINT('Ctrl Pts',(0.05,-8.06606138615749,2.78261373021506));
#43677=CARTESIAN_POINT('Ctrl Pts',(0.05,-5.37026983572066,6.62982849821033));
#43678=CARTESIAN_POINT('Ctrl Pts',(0.05,-1.04860644953161,8.46614583459751));
#43679=CARTESIAN_POINT('Ctrl Pts',(0.0499999999999999,3.59109175735748,
7.741390063858));
#43680=CARTESIAN_POINT('Ctrl Pts',(0.0500000000000001,7.14273392056364,
4.66508468971586));
#43681=CARTESIAN_POINT('Ctrl Pts',(0.0499999999999999,8.06638259247629,
1.67771968477482));
#43682=CARTESIAN_POINT('Ctrl Pts',(0.05,8.09820495979016,0.170518115411121));
#43683=CARTESIAN_POINT('Ctrl Pts',(0.,8.14819397266823,-0.171566273307201));
#43684=CARTESIAN_POINT('Ctrl Pts',(0.,8.13745234385785,-0.680654697267163));
#43685=CARTESIAN_POINT('Ctrl Pts',(0.,8.04920862642792,-1.44035172301502));
#43686=CARTESIAN_POINT('Ctrl Pts',(0.,7.56023912839487,-3.31520995088904));
#43687=CARTESIAN_POINT('Ctrl Pts',(0.,6.24287699275104,-5.64041098324849));
#43688=CARTESIAN_POINT('Ctrl Pts',(0.,3.27393288064058,-7.74838543583707));
#43689=CARTESIAN_POINT('Ctrl Pts',(0.,-0.307002703090567,-8.40773878356821));
#43690=CARTESIAN_POINT('Ctrl Pts',(0.,-3.83186243635793,-7.48986130635224));
#43691=CARTESIAN_POINT('Ctrl Pts',(0.,-6.6368226904402,-5.16933174462552));
#43692=CARTESIAN_POINT('Ctrl Pts',(0.,-8.34751129113392,-1.5752619384195));
#43693=CARTESIAN_POINT('Ctrl Pts',(0.,-8.11585252948887,2.79979113437932));
#43694=CARTESIAN_POINT('Ctrl Pts',(0.,-5.40341850389078,6.67075302444065));
#43695=CARTESIAN_POINT('Ctrl Pts',(0.,-1.05508120096718,8.51841242765781));
#43696=CARTESIAN_POINT('Ctrl Pts',(0.,3.61326401879599,7.78916544414284));
#43697=CARTESIAN_POINT('Ctrl Pts',(0.,7.18681542669997,4.693887801948));
#43698=CARTESIAN_POINT('Ctrl Pts',(0.,8.11619629477138,1.68806323182392));
#43699=CARTESIAN_POINT('Ctrl Pts',(0.,8.14819383353886,0.171572867200535));
#43700=CARTESIAN_POINT('',(0.,8.14819390295858,0.171569570250815));
#43701=CARTESIAN_POINT('Ctrl Pts',(0.,8.14819383353886,0.171572867200535));
#43702=CARTESIAN_POINT('Ctrl Pts',(0.05,8.09820495979016,0.170518115411121));
#43703=CARTESIAN_POINT('Ctrl Pts',(0.1,8.04821608604147,0.169463363621706));
#43704=CARTESIAN_POINT('Ctrl Pts',(0.15,7.99822721229278,0.168408611832292));
#43705=CARTESIAN_POINT('Ctrl Pts',(0.,8.14819397266823,-0.171566273307201));
#43706=CARTESIAN_POINT('Ctrl Pts',(0.,8.13745234385785,-0.680654697267163));
#43707=CARTESIAN_POINT('Ctrl Pts',(0.,8.04920862642792,-1.44035172301502));
#43708=CARTESIAN_POINT('Ctrl Pts',(0.,7.56023912839487,-3.31520995088904));
#43709=CARTESIAN_POINT('Ctrl Pts',(0.,6.24287699275104,-5.64041098324849));
#43710=CARTESIAN_POINT('Ctrl Pts',(0.,3.27393288064058,-7.74838543583707));
#43711=CARTESIAN_POINT('Ctrl Pts',(0.,-0.307002703090567,-8.40773878356821));
#43712=CARTESIAN_POINT('Ctrl Pts',(0.,-3.83186243635793,-7.48986130635224));
#43713=CARTESIAN_POINT('Ctrl Pts',(0.,-6.6368226904402,-5.16933174462552));
#43714=CARTESIAN_POINT('Ctrl Pts',(0.,-8.34751129113392,-1.5752619384195));
#43715=CARTESIAN_POINT('Ctrl Pts',(0.,-8.11585252948887,2.79979113437932));
#43716=CARTESIAN_POINT('Ctrl Pts',(0.,-5.40341850389078,6.67075302444065));
#43717=CARTESIAN_POINT('Ctrl Pts',(0.,-1.05508120096718,8.51841242765781));
#43718=CARTESIAN_POINT('Ctrl Pts',(0.,3.61326401879599,7.78916544414284));
#43719=CARTESIAN_POINT('Ctrl Pts',(0.,7.18681542669997,4.693887801948));
#43720=CARTESIAN_POINT('Ctrl Pts',(0.,8.11619629477138,1.68806323182392));
#43721=CARTESIAN_POINT('Ctrl Pts',(0.,8.14819383353886,0.171572867200535));
#43722=CARTESIAN_POINT('Origin',(0.,7.99822721229278,0.168408611832292));
#43723=CARTESIAN_POINT('',(1.5,7.99822721229278,0.168408611832292));
#43724=CARTESIAN_POINT('',(0.,7.99822721229278,0.168408611832292));
#43725=CARTESIAN_POINT('Origin',(1.5,-0.00140950834140008,9.76996261670138E-14));
#43726=CARTESIAN_POINT('Origin',(0.,-0.00140950834140008,9.76996261670138E-14));
#43727=CARTESIAN_POINT('',(0.,0.,0.));
#43728=CARTESIAN_POINT('Origin',(0.1,0.,0.));
#43729=CARTESIAN_POINT('',(0.2,-8.5,-1.04094977927525E-15));
#43730=CARTESIAN_POINT('Origin',(0.2,0.,0.));
#43731=CARTESIAN_POINT('',(-3.98986399474666E-16,-8.3,-1.0164568432923E-15));
#43732=CARTESIAN_POINT('',(0.1,-8.4,-1.02870331128378E-15));
#43733=CARTESIAN_POINT('Origin',(0.,0.,0.));
#43734=CARTESIAN_POINT('Origin',(1.75,0.,0.));
#43735=CARTESIAN_POINT('',(3.3,-8.5,-1.04094977927525E-15));
#43736=CARTESIAN_POINT('Origin',(3.3,0.,0.));
#43737=CARTESIAN_POINT('',(1.75,-8.5,-1.04094977927525E-15));
#43738=CARTESIAN_POINT('Origin',(3.4,0.,0.));
#43739=CARTESIAN_POINT('',(3.5,-8.2,-1.00421037530083E-15));
#43740=CARTESIAN_POINT('Origin',(3.5,0.,0.));
#43741=CARTESIAN_POINT('',(3.4,-8.35,-1.02258007728804E-15));
#43742=CARTESIAN_POINT('Origin',(3.5,3.81,0.));
#43743=CARTESIAN_POINT('',(3.5,-3.81,-4.66590430475142E-16));
#43744=CARTESIAN_POINT('Origin',(3.5,0.,0.));
#43745=CARTESIAN_POINT('Origin',(3.35,0.,0.));
#43746=CARTESIAN_POINT('',(3.2,-3.505,-4.29238703101147E-16));
#43747=CARTESIAN_POINT('',(3.35,-3.6575,-4.47914566788144E-16));
#43748=CARTESIAN_POINT('Origin',(3.2,0.,0.));
#43749=CARTESIAN_POINT('Origin',(1.75,0.,0.));
#43750=CARTESIAN_POINT('',(0.3,-3.505,-4.29238703101147E-16));
#43751=CARTESIAN_POINT('',(1.75,-3.505,-4.29238703101147E-16));
#43752=CARTESIAN_POINT('Origin',(0.3,0.,0.));
#43753=CARTESIAN_POINT('Origin',(0.15,0.,0.));
#43754=CARTESIAN_POINT('',(1.21430643318376E-16,-3.81,-4.66590430475142E-16));
#43755=CARTESIAN_POINT('',(0.15,-3.6575,-4.47914566788144E-16));
#43756=CARTESIAN_POINT('Origin',(0.,0.,0.));
#43757=CARTESIAN_POINT('Origin',(0.,8.3,0.));
#43758=CARTESIAN_POINT('',(0.,0.,0.));
#43759=CARTESIAN_POINT('Origin',(3.9,2.5,14.9));
#43760=CARTESIAN_POINT('',(4.,5.,14.8));
#43761=CARTESIAN_POINT('',(3.8,5.,15.));
#43762=CARTESIAN_POINT('',(2.58798079768202,5.,16.212019202318));
#43763=CARTESIAN_POINT('',(3.8,-5.,15.));
#43764=CARTESIAN_POINT('',(3.8,2.5,15.));
#43765=CARTESIAN_POINT('',(4.,-5.,14.8));
#43766=CARTESIAN_POINT('',(2.9,-5.,15.9));
#43767=CARTESIAN_POINT('',(4.,2.5,14.8));
#43768=CARTESIAN_POINT('Origin',(0.,5.,15.));
#43769=CARTESIAN_POINT('',(0.2,5.,15.));
#43770=CARTESIAN_POINT('',(0.,5.,15.));
#43771=CARTESIAN_POINT('',(0.2,-5.,15.));
#43772=CARTESIAN_POINT('',(0.2,2.5,15.));
#43773=CARTESIAN_POINT('',(0.,-5.,15.));
#43774=CARTESIAN_POINT('',(0.8,-1.46957615897682E-16,15.));
#43775=CARTESIAN_POINT('Origin',(2.,0.,15.));
#43776=CARTESIAN_POINT('Origin',(0.1,2.5,14.9));
#43777=CARTESIAN_POINT('',(0.,5.,14.8));
#43778=CARTESIAN_POINT('',(0.41201920231798,5.,15.212019202318));
#43779=CARTESIAN_POINT('',(0.,-5.,14.8));
#43780=CARTESIAN_POINT('',(0.,2.5,14.8));
#43781=CARTESIAN_POINT('',(0.1,-5.,14.9));
#43782=CARTESIAN_POINT('Origin',(0.,0.,-0.375961595364038));
#43783=CARTESIAN_POINT('',(0.,-5.,16.0387031894726));
#43784=CARTESIAN_POINT('',(0.,-5.,15.));
#43785=CARTESIAN_POINT('',(0.,5.,16.0387031894726));
#43786=CARTESIAN_POINT('',(0.,5.,21.));
#43787=CARTESIAN_POINT('Origin',(0.,0.,0.));
#43788=CARTESIAN_POINT('',(0.,-2.13088543051639E-15,-10.65));
#43789=CARTESIAN_POINT('Origin',(0.,-2.47990976827339E-15,-13.5));
#43790=CARTESIAN_POINT('',(0.,-11.6913429510899,-3.9));
#43791=CARTESIAN_POINT('Origin',(0.,-11.6913429510899,-6.75));
#43792=CARTESIAN_POINT('',(0.,-7.16418377501202E-16,5.85));
#43793=CARTESIAN_POINT('Origin',(0.,0.,0.));
#43794=CARTESIAN_POINT('',(0.,5.00154026730478,-5.17924656243829));
#43795=CARTESIAN_POINT('',(0.,4.43276262234474,-5.6736774259684));
#43796=CARTESIAN_POINT('',(0.,4.76627016532424,-5.38376374189465));
#43797=CARTESIAN_POINT('',(0.,6.52601163845198,-8.35291398823125));
#43798=CARTESIAN_POINT('',(0.,2.30757979347878,-2.95356744728099));
#43799=CARTESIAN_POINT('',(0.,7.36337872686537,-7.6250018835897));
#43800=CARTESIAN_POINT('',(0.,6.64227771981479,-8.2518454256447));
#43801=CARTESIAN_POINT('',(0.,8.12007109706117,-6.81354866267731));
#43802=CARTESIAN_POINT('',(0.,7.45879037646094,-7.52268541599157));
#43803=CARTESIAN_POINT('',(0.,8.78779826908344,-5.92744477678991));
#43804=CARTESIAN_POINT('',(0.,8.19665351987491,-6.7119203550552));
#43805=CARTESIAN_POINT('',(0.,9.35924448430463,-4.97639856553044));
#43806=CARTESIAN_POINT('',(0.,8.84767122648022,-5.82779944224681));
#43807=CARTESIAN_POINT('',(0.,9.82814885840795,-3.97082989020866));
#43808=CARTESIAN_POINT('',(0.,9.40446975509177,-4.8794126593455));
#43809=CARTESIAN_POINT('',(0.,10.1893739769462,-2.92175597166019));
#43810=CARTESIAN_POINT('',(0.,9.8605888704256,-3.87661725443506));
#43811=CARTESIAN_POINT('',(0.,6.9210842107559,-1.98458896188239));
#43812=CARTESIAN_POINT('',(0.,5.1444943114719,-1.475160005877));
#43813=CARTESIAN_POINT('',(0.,6.67572375288087,-2.69716747259456));
#43814=CARTESIAN_POINT('',(0.,6.80187782867024,-2.33078943342394));
#43815=CARTESIAN_POINT('',(0.,6.35722266858427,-3.38019525205841));
#43816=CARTESIAN_POINT('',(0.,6.52409765906803,-3.02233068010603));
#43817=CARTESIAN_POINT('',(0.,5.9690705223963,-4.02618890498938));
#43818=CARTESIAN_POINT('',(0.,6.17719603562876,-3.67980988356293));
#43819=CARTESIAN_POINT('',(0.,5.51551999045664,-4.62807078974308));
#43820=CARTESIAN_POINT('',(0.,5.76533351921956,-4.29655704002753));
#43821=CARTESIAN_POINT('',(0.,5.2932636167153,-4.86641157054685));
#43822=CARTESIAN_POINT('',(0.,-6.98612922918717,-1.74183764831761));
#43823=CARTESIAN_POINT('',(0.,-7.12993009493931,-1.00204632691247));
#43824=CARTESIAN_POINT('',(0.,-6.98687002250157,-1.73802659709701));
#43825=CARTESIAN_POINT('',(0.,-10.4968415286606,-1.47523487017669));
#43826=CARTESIAN_POINT('',(0.,-3.59087231247837,-0.504664192105417));
#43827=CARTESIAN_POINT('',(0.,-10.2851346985256,-2.56437209335648));
#43828=CARTESIAN_POINT('',(0.,-10.4087053980032,-1.92865595510232));
#43829=CARTESIAN_POINT('',(0.,-9.96074178033063,-3.62541351925209));
#43830=CARTESIAN_POINT('',(0.,-10.1514777049506,-3.00154442077003));
#43831=CARTESIAN_POINT('',(0.,-9.52721689077117,-4.64673415596422));
#43832=CARTESIAN_POINT('',(0.,-9.78474952320472,-4.04002529456882));
#43833=CARTESIAN_POINT('',(0.,-8.98930981925811,-5.61714420087197));
#43834=CARTESIAN_POINT('',(0.,-9.3130317440988,-5.03313438903098));
#43835=CARTESIAN_POINT('',(0.,-8.35291398823125,-6.52601163845198));
#43836=CARTESIAN_POINT('',(0.,-8.74188877728577,-5.97049806879083));
#43837=CARTESIAN_POINT('',(0.,-7.6250018835897,-7.36337872686537));
#43838=CARTESIAN_POINT('',(0.,-8.07786027133033,-6.84242474466351));
#43839=CARTESIAN_POINT('',(0.,-5.17924656243829,-5.00154026730478));
#43840=CARTESIAN_POINT('',(0.,-3.90643408422442,-3.77239954465928));
#43841=CARTESIAN_POINT('',(0.,-5.6736774259684,-4.43276262234474));
#43842=CARTESIAN_POINT('',(0.,-5.20977858758028,-4.96641719017296));
#43843=CARTESIAN_POINT('',(0.,-6.10594629232627,-3.81541870247908));
#43844=CARTESIAN_POINT('',(0.,-5.69342255834225,-4.40456365090217));
#43845=CARTESIAN_POINT('',(0.,-6.471317133354,-3.15627225688136));
#43846=CARTESIAN_POINT('',(0.,-6.1175806237891,-3.79442981291947));
#43847=CARTESIAN_POINT('',(0.,-6.76578686965854,-2.46254503194481));
#43848=CARTESIAN_POINT('',(0.,-6.4773235326941,-3.14212206678592));
#43849=CARTESIAN_POINT('',(0.,-6.76831369551442,-2.45428015697765));
#43850=CARTESIAN_POINT('',(0.,-5.00154026730478,5.17924656243829));
#43851=CARTESIAN_POINT('',(0.,-4.43276262234474,5.6736774259684));
#43852=CARTESIAN_POINT('',(0.,-4.95242154680531,5.22194481474698));
#43853=CARTESIAN_POINT('',(0.,-6.52601163845198,8.35291398823125));
#43854=CARTESIAN_POINT('',(0.,-2.12518282886596,2.7201099786874));
#43855=CARTESIAN_POINT('',(0.,-7.36337872686537,7.6250018835897));
#43856=CARTESIAN_POINT('',(0.,-6.82842910129586,8.09002649849703));
#43857=CARTESIAN_POINT('',(0.,-8.12007109706117,6.81354866267732));
#43858=CARTESIAN_POINT('',(0.,-7.64631326236769,7.32159174073164));
#43859=CARTESIAN_POINT('',(0.,-8.78779826908344,5.92744477678992));
#43860=CARTESIAN_POINT('',(0.,-8.37735226025856,6.47212502735574));
#43861=CARTESIAN_POINT('',(0.,-9.35924448430463,4.97639856553044));
#43862=CARTESIAN_POINT('',(0.,-9.01364841929725,5.55156700570328));
#43863=CARTESIAN_POINT('',(0.,-9.82814885840794,3.97082989020867));
#43864=CARTESIAN_POINT('',(0.,-9.54847140056915,4.57060013405449));
#43865=CARTESIAN_POINT('',(0.,-10.1893739769462,2.92175597166019));
#43866=CARTESIAN_POINT('',(0.,-9.9763214056594,3.54050556670805));
#43867=CARTESIAN_POINT('',(0.,-6.9210842107559,1.98458896188239));
#43868=CARTESIAN_POINT('',(0.,-5.04487966547428,1.44659596578319));
#43869=CARTESIAN_POINT('',(0.,-6.67572375288087,2.69716747259457));
#43870=CARTESIAN_POINT('',(0.,-6.91761036390404,1.99467774569693));
#43871=CARTESIAN_POINT('',(0.,-6.35722266858427,3.38019525205841));
#43872=CARTESIAN_POINT('',(0.,-6.66809930454541,2.71351815481502));
#43873=CARTESIAN_POINT('',(0.,-5.9690705223963,4.02618890498938));
#43874=CARTESIAN_POINT('',(0.,-6.3431732284458,3.40357744701939));
#43875=CARTESIAN_POINT('',(0.,-5.51551999045664,4.62807078974308));
#43876=CARTESIAN_POINT('',(0.,-5.94603225960321,4.05676171232808));
#43877=CARTESIAN_POINT('',(0.,-5.48078650262205,4.66531789528692));
#43878=CARTESIAN_POINT('',(0.,1.98458896188239,6.9210842107559));
#43879=CARTESIAN_POINT('',(0.,2.69716747259457,6.67572375288087));
#43880=CARTESIAN_POINT('',(0.,2.22059985717734,6.83981914246863));
#43881=CARTESIAN_POINT('',(0.,3.97082989020867,9.82814885840795));
#43882=CARTESIAN_POINT('',(0.,1.2832925189996,3.17626044286338));
#43883=CARTESIAN_POINT('',(0.,2.92175597166019,10.1893739769462));
#43884=CARTESIAN_POINT('',(0.,3.76642767818846,9.89853018422399));
#43885=CARTESIAN_POINT('',(0.,1.84067068326946,10.4389621819294));
#43886=CARTESIAN_POINT('',(0.,2.69268732848961,10.2422586402386));
#43887=CARTESIAN_POINT('',(0.,0.739418621687727,10.5741789327541));
#43888=CARTESIAN_POINT('',(0.,1.5880960033298,10.469974453101));
#43889=CARTESIAN_POINT('',(0.,-0.36993466504651,10.5935427664024));
#43890=CARTESIAN_POINT('',(0.,0.465360517618589,10.5789626347548));
#43891=CARTESIAN_POINT('',(0.,-1.4752348701767,10.4968415286606));
#43892=CARTESIAN_POINT('',(0.,-0.662580977805997,10.5679395316133));
#43893=CARTESIAN_POINT('',(0.,-2.56437209335648,10.2851346985256));
#43894=CARTESIAN_POINT('',(0.,-1.78272859909527,10.4370708025755));
#43895=CARTESIAN_POINT('',(0.,-1.74183764831761,6.98612922918717));
#43896=CARTESIAN_POINT('',(0.,-1.23806022724748,4.96558835401325));
#43897=CARTESIAN_POINT('',(0.,-1.00204632691247,7.12993009493931));
#43898=CARTESIAN_POINT('',(0.,-1.59209924108996,7.01523542707388));
#43899=CARTESIAN_POINT('',(0.,-0.251276376258007,7.19561395453749));
#43900=CARTESIAN_POINT('',(0.,-0.830675100725787,7.14492313448518));
#43901=CARTESIAN_POINT('',(0.,0.502246610957702,7.18246116187073));
#43902=CARTESIAN_POINT('',(0.,-0.0596154118396585,7.19226849995936));
#43903=CARTESIAN_POINT('',(0.,1.2502668792019,7.0906158216879));
#43904=CARTESIAN_POINT('',(0.,0.711990013474533,7.15670791029043));
#43905=CARTESIAN_POINT('',(0.,1.47505007879912,7.03872053100147));
#43906=CARTESIAN_POINT('',(0.,6.98612922918717,1.74183764831761));
#43907=CARTESIAN_POINT('',(0.,7.12993009493931,1.00204632691247));
#43908=CARTESIAN_POINT('',(0.,7.05728886874884,1.37575303883564));
#43909=CARTESIAN_POINT('',(0.,10.4968415286606,1.47523487017669));
#43910=CARTESIAN_POINT('',(0.,3.53905778246093,0.497382134807054));
#43911=CARTESIAN_POINT('',(0.,10.2851346985256,2.56437209335648));
#43912=CARTESIAN_POINT('',(0.,10.4791242442505,1.56638239684096));
#43913=CARTESIAN_POINT('',(0.,9.96074178033063,3.62541351925209));
#43914=CARTESIAN_POINT('',(0.,10.2565952330031,2.65772047889074));
#43915=CARTESIAN_POINT('',(0.,9.52721689077117,4.64673415596422));
#43916=CARTESIAN_POINT('',(0.,9.91997159267681,3.72146206229143));
#43917=CARTESIAN_POINT('',(0.,8.98930981925811,5.61714420087197));
#43918=CARTESIAN_POINT('',(0.,9.472448501687,4.74553894535134));
#43919=CARTESIAN_POINT('',(0.,8.35291398823125,6.52601163845198));
#43920=CARTESIAN_POINT('',(0.,8.91853294571702,5.71822405174313));
#43921=CARTESIAN_POINT('',(0.,7.6250018835897,7.36337872686537));
#43922=CARTESIAN_POINT('',(0.,8.2640116528114,6.62828207644714));
#43923=CARTESIAN_POINT('',(0.,5.17924656243829,5.00154026730478));
#43924=CARTESIAN_POINT('',(0.,3.71856779936528,3.59097918220609));
#43925=CARTESIAN_POINT('',(0.,5.6736774259684,4.43276262234474));
#43926=CARTESIAN_POINT('',(0.,5.39592996906135,4.75227452195658));
#43927=CARTESIAN_POINT('',(0.,6.10594629232627,3.81541870247908));
#43928=CARTESIAN_POINT('',(0.,5.87006672677349,4.15228963385447));
#43929=CARTESIAN_POINT('',(0.,6.471317133354,3.15627225688136));
#43930=CARTESIAN_POINT('',(0.,6.2769973813773,3.50683436923982));
#43931=CARTESIAN_POINT('',(0.,6.76578686965854,2.46254503194481));
#43932=CARTESIAN_POINT('',(0.,6.61254560216618,2.82355883450853));
#43933=CARTESIAN_POINT('',(0.,6.87343122356698,2.11045621509837));
#43934=CARTESIAN_POINT('',(0.,-1.9845889618824,-6.92108421075589));
#43935=CARTESIAN_POINT('',(0.,-2.69716747259457,-6.67572375288087));
#43936=CARTESIAN_POINT('',(0.,-2.10486732194354,-6.87966905010565));
#43937=CARTESIAN_POINT('',(0.,-3.97082989020867,-9.82814885840794));
#43938=CARTESIAN_POINT('',(0.,-1.41387495359497,-3.49946331001749));
#43939=CARTESIAN_POINT('',(0.,-2.9217559716602,-10.1893739769462));
#43940=CARTESIAN_POINT('',(0.,-3.65069514295465,-9.93838009186101));
#43941=CARTESIAN_POINT('',(0.,-1.84067068326946,-10.4389621819294));
#43942=CARTESIAN_POINT('',(0.,-2.61028197063542,-10.2612834161454));
#43943=CARTESIAN_POINT('',(0.,-0.739418621687731,-10.5741789327541));
#43944=CARTESIAN_POINT('',(0.,-1.54261933241824,-10.4755582861702));
#43945=CARTESIAN_POINT('',(0.,0.369934665046504,-10.5935427664024));
#43946=CARTESIAN_POINT('',(0.,-0.458800082389754,-10.5790771475776));
#43947=CARTESIAN_POINT('',(0.,1.47523487017669,-10.4968415286606));
#43948=CARTESIAN_POINT('',(0.,0.629938454852123,-10.5707953823206));
#43949=CARTESIAN_POINT('',(0.,2.56437209335647,-10.2851346985256));
#43950=CARTESIAN_POINT('',(0.,1.712309752848,-10.4507588396782));
#43951=CARTESIAN_POINT('',(0.,1.74183764831761,-6.98612922918718));
#43952=CARTESIAN_POINT('',(0.,1.326311866109,-5.31954634451231));
#43953=CARTESIAN_POINT('',(0.,1.00204632691247,-7.12993009493931));
#43954=CARTESIAN_POINT('',(0.,1.52168039484269,-7.02892346417654));
#43955=CARTESIAN_POINT('',(0.,0.251276376258003,-7.19561395453749));
#43956=CARTESIAN_POINT('',(0.,0.798032577771921,-7.14777898519253));
#43957=CARTESIAN_POINT('',(0.,-0.502246610957704,-7.18246116187073));
#43958=CARTESIAN_POINT('',(0.,0.0661758470684938,-7.19238301278224));
#43959=CARTESIAN_POINT('',(0.,-1.2502668792019,-7.0906158216879));
#43960=CARTESIAN_POINT('',(0.,-0.666513342562969,-7.16229174335963));
#43961=CARTESIAN_POINT('',(0.,-1.39264472094493,-7.05774530690832));
#43962=CARTESIAN_POINT('',(0.,11.6913429510899,-3.90000000000001));
#43963=CARTESIAN_POINT('Origin',(0.,11.6913429510899,-6.75000000000001));
#43964=CARTESIAN_POINT('Origin',(0.1,0.,0.));
#43965=CARTESIAN_POINT('',(0.0089490830417863,5.,16.0480768092719));
#43966=CARTESIAN_POINT('Ctrl Pts',(5.20417042793042E-17,5.,16.0387031894726));
#43967=CARTESIAN_POINT('Ctrl Pts',(0.00447323435791146,5.,16.0433887514115));
#43968=CARTESIAN_POINT('Ctrl Pts',(0.0089490830417863,5.,16.0480768092719));
#43969=CARTESIAN_POINT('',(0.2,5.19080451686515,16.1881298631958));
#43970=CARTESIAN_POINT('Ctrl Pts',(0.00894908304178668,5.,16.0480768092719));
#43971=CARTESIAN_POINT('Ctrl Pts',(0.07251246250349,5.06367493004374,16.0948150550825));
#43972=CARTESIAN_POINT('Ctrl Pts',(0.136203613263926,5.12728130687429,16.1415029819226));
#43973=CARTESIAN_POINT('Ctrl Pts',(0.2,5.19080451686515,16.1881298631958));
#43974=CARTESIAN_POINT('',(0.2,-5.19080451686515,16.1881298631958));
#43975=CARTESIAN_POINT('Origin',(0.2,0.,0.));
#43976=CARTESIAN_POINT('',(0.0089490830417863,-5.,16.0480768092719));
#43977=CARTESIAN_POINT('Ctrl Pts',(0.2,-5.19080451686515,16.1881298631958));
#43978=CARTESIAN_POINT('Ctrl Pts',(0.136203613263926,-5.12728130687429,
16.1415029819226));
#43979=CARTESIAN_POINT('Ctrl Pts',(0.07251246250349,-5.06367493004374,16.0948150550825));
#43980=CARTESIAN_POINT('Ctrl Pts',(0.00894908304178668,-5.,16.0480768092719));
#43981=CARTESIAN_POINT('Ctrl Pts',(0.0089490830417863,-5.,16.0480768092719));
#43982=CARTESIAN_POINT('Ctrl Pts',(0.00447323435791139,-5.,16.0433887514115));
#43983=CARTESIAN_POINT('Ctrl Pts',(5.20417042793042E-17,-5.,16.0387031894726));
#43984=CARTESIAN_POINT('Origin',(0.,5.09540225843257,16.1181033362339));
#43985=CARTESIAN_POINT('',(3.8,5.19080451686515,16.1881298631958));
#43986=CARTESIAN_POINT('',(0.,5.19080451686515,16.1881298631958));
#43987=CARTESIAN_POINT('',(3.99105091695821,5.,16.0480768092719));
#43988=CARTESIAN_POINT('',(0.,5.,16.0480768092719));
#43989=CARTESIAN_POINT('Ctrl Pts',(3.99105091695821,5.,16.0480768092719));
#43990=CARTESIAN_POINT('Ctrl Pts',(3.92748753749667,5.06367493004358,16.0948150550824));
#43991=CARTESIAN_POINT('Ctrl Pts',(3.8637963867364,5.12728130687397,16.1415029819224));
#43992=CARTESIAN_POINT('Ctrl Pts',(3.8,5.19080451686515,16.1881298631958));
#43993=CARTESIAN_POINT('Origin',(3.9,0.,0.));
#43994=CARTESIAN_POINT('',(3.8,-5.19080451686515,16.1881298631958));
#43995=CARTESIAN_POINT('Origin',(3.8,0.,0.));
#43996=CARTESIAN_POINT('',(4.,5.,16.0387031894726));
#43997=CARTESIAN_POINT('Ctrl Pts',(3.99105091695821,5.,16.0480768092719));
#43998=CARTESIAN_POINT('Ctrl Pts',(3.99552676564209,5.,16.0433887514115));
#43999=CARTESIAN_POINT('Ctrl Pts',(4.,5.,16.0387031894726));
#44000=CARTESIAN_POINT('',(4.,-5.,16.0387031894726));
#44001=CARTESIAN_POINT('Origin',(4.,0.,0.));
#44002=CARTESIAN_POINT('',(3.99105091695821,-5.,16.0480768092719));
#44003=CARTESIAN_POINT('Ctrl Pts',(4.,-5.,16.0387031894726));
#44004=CARTESIAN_POINT('Ctrl Pts',(3.99552676564209,-5.,16.0433887514115));
#44005=CARTESIAN_POINT('Ctrl Pts',(3.99105091695821,-5.,16.0480768092719));
#44006=CARTESIAN_POINT('Ctrl Pts',(3.8,-5.19080451686515,16.1881298631958));
#44007=CARTESIAN_POINT('Ctrl Pts',(3.8637963867364,-5.12728130687397,16.1415029819224));
#44008=CARTESIAN_POINT('Ctrl Pts',(3.92748753749667,-5.06367493004358,16.0948150550824));
#44009=CARTESIAN_POINT('Ctrl Pts',(3.99105091695821,-5.,16.0480768092719));
#44010=CARTESIAN_POINT('Origin',(0.,-5.09540225843257,16.1181033362339));
#44011=CARTESIAN_POINT('',(0.,-5.,16.0480768092719));
#44012=CARTESIAN_POINT('',(0.,-5.19080451686515,16.1881298631958));
#44013=CARTESIAN_POINT('Origin',(0.,-5.,15.));
#44014=CARTESIAN_POINT('',(4.,-5.,15.));
#44015=CARTESIAN_POINT('Origin',(4.,0.,-0.375961595364038));
#44016=CARTESIAN_POINT('',(4.,5.,21.));
#44017=CARTESIAN_POINT('',(4.,-2.82893410603039E-15,-10.65));
#44018=CARTESIAN_POINT('Origin',(4.,-2.47990976827339E-15,-13.5));
#44019=CARTESIAN_POINT('',(4.,-11.6913429510899,-3.9));
#44020=CARTESIAN_POINT('Origin',(4.,-11.6913429510899,-6.75));
#44021=CARTESIAN_POINT('',(4.,-7.16418377501202E-16,5.85));
#44022=CARTESIAN_POINT('Origin',(4.,0.,0.));
#44023=CARTESIAN_POINT('',(4.,7.36337872686537,-7.6250018835897));
#44024=CARTESIAN_POINT('',(4.,6.52601163845198,-8.35291398823125));
#44025=CARTESIAN_POINT('',(4.,7.06096126402149,-7.88788937332392));
#44026=CARTESIAN_POINT('',(4.,4.43276262234474,-5.6736774259684));
#44027=CARTESIAN_POINT('',(4.,3.3542043015324,-4.29318572841242));
#44028=CARTESIAN_POINT('',(4.,5.00154026730478,-5.17924656243829));
#44029=CARTESIAN_POINT('',(4.,4.48188134284422,-5.6309791736597));
#44030=CARTESIAN_POINT('',(4.,5.51551999045664,-4.62807078974308));
#44031=CARTESIAN_POINT('',(4.,5.03627375513937,-5.14199945689445));
#44032=CARTESIAN_POINT('',(4.,5.9690705223963,-4.02618890498938));
#44033=CARTESIAN_POINT('',(4.,5.53855825324973,-4.59749798240438));
#44034=CARTESIAN_POINT('',(4.,6.35722266858427,-3.38019525205841));
#44035=CARTESIAN_POINT('',(4.,5.98311996253477,-4.00280671002841));
#44036=CARTESIAN_POINT('',(4.,6.67572375288087,-2.69716747259456));
#44037=CARTESIAN_POINT('',(4.,6.36484711691973,-3.36384456983795));
#44038=CARTESIAN_POINT('',(4.,6.9210842107559,-1.98458896188239));
#44039=CARTESIAN_POINT('',(4.,6.67919759973273,-2.68707868878003));
#44040=CARTESIAN_POINT('',(4.,10.1893739769462,-2.92175597166019));
#44041=CARTESIAN_POINT('',(4.,3.51034942837676,-1.00657650098811));
#44042=CARTESIAN_POINT('',(4.,9.82814885840795,-3.97082989020866));
#44043=CARTESIAN_POINT('',(4.,10.0412014296947,-3.35208029516082));
#44044=CARTESIAN_POINT('',(4.,9.35924448430463,-4.97639856553044));
#44045=CARTESIAN_POINT('',(4.,9.63892194214343,-4.37662832168461));
#44046=CARTESIAN_POINT('',(4.,8.78779826908344,-5.92744477678991));
#44047=CARTESIAN_POINT('',(4.,9.13339433409081,-5.35227633661707));
#44048=CARTESIAN_POINT('',(4.,8.12007109706117,-6.81354866267731));
#44049=CARTESIAN_POINT('',(4.,8.53051710588605,-6.2688684121115));
#44050=CARTESIAN_POINT('',(4.,7.83713656155884,-7.11695880553538));
#44051=CARTESIAN_POINT('',(4.,-10.2851346985256,-2.56437209335648));
#44052=CARTESIAN_POINT('',(4.,-10.4968415286606,-1.47523487017669));
#44053=CARTESIAN_POINT('',(4.,-10.3028519829357,-2.47322456669221));
#44054=CARTESIAN_POINT('',(4.,-7.12993009493931,-1.00204632691247));
#44055=CARTESIAN_POINT('',(4.,-5.27432802933904,-0.741258463737529));
#44056=CARTESIAN_POINT('',(4.,-6.98612922918717,-1.74183764831761));
#44057=CARTESIAN_POINT('',(4.,-7.05877045537764,-1.36813093639444));
#44058=CARTESIAN_POINT('',(4.,-6.76578686965854,-2.46254503194481));
#44059=CARTESIAN_POINT('',(4.,-6.87848487527874,-2.09392646516405));
#44060=CARTESIAN_POINT('',(4.,-6.471317133354,-3.15627225688136));
#44061=CARTESIAN_POINT('',(4.,-6.62455840084636,-2.79525845431765));
#44062=CARTESIAN_POINT('',(4.,-6.10594629232627,-3.81541870247908));
#44063=CARTESIAN_POINT('',(4.,-6.30026604430297,-3.46485659012061));
#44064=CARTESIAN_POINT('',(4.,-5.6736774259684,-4.43276262234474));
#44065=CARTESIAN_POINT('',(4.,-5.90955699152118,-4.09589169096934));
#44066=CARTESIAN_POINT('',(4.,-5.17924656243829,-5.00154026730478));
#44067=CARTESIAN_POINT('',(4.,-5.45699401934533,-4.68202836769294));
#44068=CARTESIAN_POINT('',(4.,-7.6250018835897,-7.36337872686537));
#44069=CARTESIAN_POINT('',(4.,-2.68355642364871,-2.59148031487898));
#44070=CARTESIAN_POINT('',(4.,-8.35291398823125,-6.52601163845198));
#44071=CARTESIAN_POINT('',(4.,-7.71390421900955,-7.26110828887021));
#44072=CARTESIAN_POINT('',(4.,-8.98930981925811,-5.61714420087197));
#44073=CARTESIAN_POINT('',(4.,-8.42369086177234,-6.42493178758083));
#44074=CARTESIAN_POINT('',(4.,-9.52721689077117,-4.64673415596422));
#44075=CARTESIAN_POINT('',(4.,-9.04407820834228,-5.51833941148486));
#44076=CARTESIAN_POINT('',(4.,-9.96074178033063,-3.62541351925209));
#44077=CARTESIAN_POINT('',(4.,-9.56798707842499,-4.55068561292488));
#44078=CARTESIAN_POINT('',(4.,-9.98928124585308,-3.53206513371783));
#44079=CARTESIAN_POINT('',(4.,-7.36337872686537,7.6250018835897));
#44080=CARTESIAN_POINT('',(4.,-6.52601163845198,8.35291398823125));
#44081=CARTESIAN_POINT('',(4.,-7.24711264550256,7.72607044617626));
#44082=CARTESIAN_POINT('',(4.,-4.43276262234474,5.6736774259684));
#44083=CARTESIAN_POINT('',(4.,-3.17180733691958,4.05972825981883));
#44084=CARTESIAN_POINT('',(4.,-5.00154026730478,5.17924656243829));
#44085=CARTESIAN_POINT('',(4.,-4.66803272432529,5.46916024651204));
#44086=CARTESIAN_POINT('',(4.,-5.51551999045664,4.62807078974308));
#44087=CARTESIAN_POINT('',(4.,-5.22379664104612,4.94090578163452));
#44088=CARTESIAN_POINT('',(4.,-5.9690705223963,4.02618890498938));
#44089=CARTESIAN_POINT('',(4.,-5.71925699363338,4.35770265470493));
#44090=CARTESIAN_POINT('',(4.,-6.35722266858427,3.38019525205841));
#44091=CARTESIAN_POINT('',(4.,-6.14909715535181,3.72657427348487));
#44092=CARTESIAN_POINT('',(4.,-6.67572375288087,2.69716747259457));
#44093=CARTESIAN_POINT('',(4.,-6.50884876239711,3.05503204454694));
#44094=CARTESIAN_POINT('',(4.,-6.9210842107559,1.98458896188239));
#44095=CARTESIAN_POINT('',(4.,-6.79493013496653,2.35096700105301));
#44096=CARTESIAN_POINT('',(4.,-10.1893739769462,2.92175597166019));
#44097=CARTESIAN_POINT('',(4.,-3.41073478237913,0.97801246089429));
#44098=CARTESIAN_POINT('',(4.,-9.82814885840794,3.97082989020867));
#44099=CARTESIAN_POINT('',(4.,-10.1569339649285,3.01596860743381));
#44100=CARTESIAN_POINT('',(4.,-9.35924448430463,4.97639856553044));
#44101=CARTESIAN_POINT('',(4.,-9.78292358762081,4.06781579639361));
#44102=CARTESIAN_POINT('',(4.,-8.78779826908344,5.92744477678992));
#44103=CARTESIAN_POINT('',(4.,-9.29937152690785,5.07604390007354));
#44104=CARTESIAN_POINT('',(4.,-8.12007109706117,6.81354866267732));
#44105=CARTESIAN_POINT('',(4.,-8.7112158462697,6.02907308441204));
#44106=CARTESIAN_POINT('',(4.,-8.02465944746559,6.91586513027545));
#44107=CARTESIAN_POINT('',(4.,2.92175597166019,10.1893739769462));
#44108=CARTESIAN_POINT('',(4.,3.97082989020867,9.82814885840795));
#44109=CARTESIAN_POINT('',(4.,3.24189071891422,10.0791427434931));
#44110=CARTESIAN_POINT('',(4.,2.69716747259457,6.67572375288087));
#44111=CARTESIAN_POINT('',(4.,1.92012372780665,4.75247299562692));
#44112=CARTESIAN_POINT('',(4.,1.98458896188239,6.9210842107559));
#44113=CARTESIAN_POINT('',(4.,2.57688911253343,6.71713891353112));
#44114=CARTESIAN_POINT('',(4.,1.2502668792019,7.0906158216879));
#44115=CARTESIAN_POINT('',(4.,1.84221112013937,6.95395472553547));
#44116=CARTESIAN_POINT('',(4.,0.502246610957702,7.18246116187073));
#44117=CARTESIAN_POINT('',(4.,1.08600014759663,7.11078524019901));
#44118=CARTESIAN_POINT('',(4.,-0.251276376258007,7.19561395453749));
#44119=CARTESIAN_POINT('',(4.,0.317146081768196,7.18569210362599));
#44120=CARTESIAN_POINT('',(4.,-1.00204632691247,7.12993009493931));
#44121=CARTESIAN_POINT('',(4.,-0.455290125398554,7.17776506428427));
#44122=CARTESIAN_POINT('',(4.,-1.74183764831761,6.98612922918717));
#44123=CARTESIAN_POINT('',(4.,-1.22220358038739,7.08713585994994));
#44124=CARTESIAN_POINT('',(4.,-2.56437209335648,10.2851346985256));
#44125=CARTESIAN_POINT('',(4.,-0.826793004728047,3.31608561934406));
#44126=CARTESIAN_POINT('',(4.,-1.4752348701767,10.4968415286606));
#44127=CARTESIAN_POINT('',(4.,-2.32729721068516,10.331217387508));
#44128=CARTESIAN_POINT('',(4.,-0.36993466504651,10.5935427664024));
#44129=CARTESIAN_POINT('',(4.,-1.21523108037109,10.5195889127424));
#44130=CARTESIAN_POINT('',(4.,0.739418621687727,10.5741789327541));
#44131=CARTESIAN_POINT('',(4.,-0.0893161257485295,10.5886445515789));
#44132=CARTESIAN_POINT('',(4.,1.84067068326946,10.4389621819294));
#44133=CARTESIAN_POINT('',(4.,1.03746997253894,10.5375828285134));
#44134=CARTESIAN_POINT('',(4.,2.15214468429424,10.3670527427302));
#44135=CARTESIAN_POINT('',(4.,10.2851346985256,2.56437209335648));
#44136=CARTESIAN_POINT('',(4.,10.4968415286606,1.47523487017669));
#44137=CARTESIAN_POINT('',(4.,10.373270829183,2.11095100843085));
#44138=CARTESIAN_POINT('',(4.,7.12993009493931,1.00204632691247));
#44139=CARTESIAN_POINT('',(4.,5.2225134993216,0.733976406439165));
#44140=CARTESIAN_POINT('',(4.,6.98612922918717,1.74183764831761));
#44141=CARTESIAN_POINT('',(4.,7.12918930162491,1.00585737813307));
#44142=CARTESIAN_POINT('',(4.,6.76578686965854,2.46254503194481));
#44143=CARTESIAN_POINT('',(4.,6.98360240333129,1.75010252328477));
#44144=CARTESIAN_POINT('',(4.,6.471317133354,3.15627225688136));
#44145=CARTESIAN_POINT('',(4.,6.75978047031845,2.47669522204026));
#44146=CARTESIAN_POINT('',(4.,6.10594629232627,3.81541870247908));
#44147=CARTESIAN_POINT('',(4.,6.45968280189117,3.17726114644097));
#44148=CARTESIAN_POINT('',(4.,5.6736774259684,4.43276262234474));
#44149=CARTESIAN_POINT('',(4.,6.08620115995242,3.84361767392164));
#44150=CARTESIAN_POINT('',(4.,5.17924656243829,5.00154026730478));
#44151=CARTESIAN_POINT('',(4.,5.64314540082641,4.46788569947656));
#44152=CARTESIAN_POINT('',(4.,7.6250018835897,7.36337872686537));
#44153=CARTESIAN_POINT('',(4.,2.49569013878957,2.4100599524258));
#44154=CARTESIAN_POINT('',(4.,8.35291398823125,6.52601163845198));
#44155=CARTESIAN_POINT('',(4.,7.90005560049063,7.04696562065383));
#44156=CARTESIAN_POINT('',(4.,8.98930981925811,5.61714420087197));
#44157=CARTESIAN_POINT('',(4.,8.60033503020359,6.17265777053313));
#44158=CARTESIAN_POINT('',(4.,9.52721689077117,4.64673415596422));
#44159=CARTESIAN_POINT('',(4.,9.20349496593048,5.23074396780521));
#44160=CARTESIAN_POINT('',(4.,9.96074178033063,3.62541351925209));
#44161=CARTESIAN_POINT('',(4.,9.70320914789708,4.23212238064749));
#44162=CARTESIAN_POINT('',(4.,10.0943987739056,3.18824119183854));
#44163=CARTESIAN_POINT('',(4.,-2.9217559716602,-10.1893739769462));
#44164=CARTESIAN_POINT('',(4.,-3.97082989020867,-9.82814885840794));
#44165=CARTESIAN_POINT('',(4.,-3.12615818368041,-10.1189926511301));
#44166=CARTESIAN_POINT('',(4.,-2.69716747259457,-6.67572375288087));
#44167=CARTESIAN_POINT('',(4.,-2.05070616240202,-5.07567586278102));
#44168=CARTESIAN_POINT('',(4.,-1.9845889618824,-6.92108421075589));
#44169=CARTESIAN_POINT('',(4.,-2.46115657729962,-6.75698882116814));
#44170=CARTESIAN_POINT('',(4.,-1.2502668792019,-7.0906158216879));
#44171=CARTESIAN_POINT('',(4.,-1.75980576228518,-6.97297950144232));
#44172=CARTESIAN_POINT('',(4.,-0.502246610957704,-7.18246116187073));
#44173=CARTESIAN_POINT('',(4.,-1.04052347668507,-7.11636907326821));
#44174=CARTESIAN_POINT('',(4.,0.251276376258003,-7.19561395453749));
#44175=CARTESIAN_POINT('',(4.,-0.31058564653936,-7.18580661644886));
#44176=CARTESIAN_POINT('',(4.,1.00204632691247,-7.12993009493931));
#44177=CARTESIAN_POINT('',(4.,0.422647602444687,-7.18062091499162));
#44178=CARTESIAN_POINT('',(4.,1.74183764831761,-6.98612922918718));
#44179=CARTESIAN_POINT('',(4.,1.15178473414012,-7.10082389705261));
#44180=CARTESIAN_POINT('',(4.,2.56437209335647,-10.2851346985256));
#44181=CARTESIAN_POINT('',(4.,0.915044643589561,-3.67004360984312));
#44182=CARTESIAN_POINT('',(4.,1.47523487017669,-10.4968415286606));
#44183=CARTESIAN_POINT('',(4.,2.25687836443789,-10.3449054246107));
#44184=CARTESIAN_POINT('',(4.,0.369934665046504,-10.5935427664024));
#44185=CARTESIAN_POINT('',(4.,1.18258855741722,-10.5224447634498));
#44186=CARTESIAN_POINT('',(4.,-0.739418621687731,-10.5741789327541));
#44187=CARTESIAN_POINT('',(4.,0.0958765609773636,-10.5887590644018));
#44188=CARTESIAN_POINT('',(4.,-1.84067068326946,-10.4389621819294));
#44189=CARTESIAN_POINT('',(4.,-0.991993301627379,-10.5431666615826));
#44190=CARTESIAN_POINT('',(4.,-2.06973932644006,-10.386077518637));
#44191=CARTESIAN_POINT('',(4.,11.6913429510899,-3.90000000000001));
#44192=CARTESIAN_POINT('Origin',(4.,11.6913429510899,-6.75000000000001));
#44193=CARTESIAN_POINT('Origin',(0.,0.,0.));
#44194=CARTESIAN_POINT('Origin',(0.1,-2.47990976827339E-15,-13.5));
#44195=CARTESIAN_POINT('',(0.2,-2.80444117004744E-15,-10.85));
#44196=CARTESIAN_POINT('',(0.1,-2.14313189850787E-15,-10.75));
#44197=CARTESIAN_POINT('Origin',(0.2,-2.47990976827339E-15,-13.5));
#44198=CARTESIAN_POINT('Origin',(0.,-2.47990976827339E-15,-13.5));
#44199=CARTESIAN_POINT('',(3.8,-2.15537836649934E-15,-10.85));
#44200=CARTESIAN_POINT('',(0.,-2.80444117004744E-15,-10.85));
#44201=CARTESIAN_POINT('Origin',(3.8,-2.47990976827339E-15,-13.5));
#44202=CARTESIAN_POINT('Origin',(3.9,-2.47990976827339E-15,-13.5));
#44203=CARTESIAN_POINT('',(3.9,-2.81668763803891E-15,-10.75));
#44204=CARTESIAN_POINT('Origin',(0.1,11.6913429510899,-6.75000000000001));
#44205=CARTESIAN_POINT('',(0.2,11.6913429510899,-4.10000000000001));
#44206=CARTESIAN_POINT('',(0.1,11.6913429510899,-4.00000000000001));
#44207=CARTESIAN_POINT('Origin',(0.2,11.6913429510899,-6.75000000000001));
#44208=CARTESIAN_POINT('Origin',(0.,11.6913429510899,-6.75000000000001));
#44209=CARTESIAN_POINT('',(3.8,11.6913429510899,-4.10000000000001));
#44210=CARTESIAN_POINT('',(0.,11.6913429510899,-4.10000000000001));
#44211=CARTESIAN_POINT('Origin',(3.8,11.6913429510899,-6.75000000000001));
#44212=CARTESIAN_POINT('Origin',(3.9,11.6913429510899,-6.75000000000001));
#44213=CARTESIAN_POINT('',(3.9,11.6913429510899,-4.00000000000001));
#44214=CARTESIAN_POINT('Origin',(0.1,-11.6913429510899,-6.75));
#44215=CARTESIAN_POINT('',(0.2,-11.6913429510899,-4.1));
#44216=CARTESIAN_POINT('',(0.1,-11.6913429510899,-4.));
#44217=CARTESIAN_POINT('Origin',(0.2,-11.6913429510899,-6.75));
#44218=CARTESIAN_POINT('Origin',(0.,-11.6913429510899,-6.75));
#44219=CARTESIAN_POINT('',(3.8,-11.6913429510899,-4.1));
#44220=CARTESIAN_POINT('',(0.,-11.6913429510899,-4.1));
#44221=CARTESIAN_POINT('Origin',(3.8,-11.6913429510899,-6.75));
#44222=CARTESIAN_POINT('Origin',(3.9,-11.6913429510899,-6.75));
#44223=CARTESIAN_POINT('',(3.9,-11.6913429510899,-4.));
#44224=CARTESIAN_POINT('Origin',(2.,0.,14.9));
#44225=CARTESIAN_POINT('',(1.,1.22464679914735E-16,14.8));
#44226=CARTESIAN_POINT('',(0.9,-1.34711147906209E-16,14.9));
#44227=CARTESIAN_POINT('Origin',(2.,0.,14.8));
#44228=CARTESIAN_POINT('Origin',(2.,0.,21.));
#44229=CARTESIAN_POINT('',(1.,1.47968513756208E-16,5.85));
#44230=CARTESIAN_POINT('',(1.,1.22464679914735E-16,21.));
#44231=CARTESIAN_POINT('',(2.,1.,5.76389625166866));
#44232=CARTESIAN_POINT('Ctrl Pts',(2.,1.,5.76389625166866));
#44233=CARTESIAN_POINT('Ctrl Pts',(1.87416996601027,1.,5.76389625166866));
#44234=CARTESIAN_POINT('Ctrl Pts',(1.74012546214185,0.974802142157817,5.76844303881019));
#44235=CARTESIAN_POINT('Ctrl Pts',(1.49382158240198,0.872672585527757,5.78477457060768));
#44236=CARTESIAN_POINT('Ctrl Pts',(1.38154050485319,0.795754067226289,5.79631351124354));
#44237=CARTESIAN_POINT('Ctrl Pts',(1.20424855638596,0.61846211875906,5.81790159694625));
#44238=CARTESIAN_POINT('Ctrl Pts',(1.127327980397,0.506179916337122,5.82936652378142));
#44239=CARTESIAN_POINT('Ctrl Pts',(1.02519693018325,0.259872166731316,5.84552808842072));
#44240=CARTESIAN_POINT('Ctrl Pts',(1.,0.125826309913858,5.85));
#44241=CARTESIAN_POINT('Ctrl Pts',(1.,1.04083408558608E-16,5.85));
#44242=CARTESIAN_POINT('',(3.,-4.44945362549441E-16,5.85));
#44243=CARTESIAN_POINT('Ctrl Pts',(3.,-1.73472347597681E-16,5.85));
#44244=CARTESIAN_POINT('Ctrl Pts',(3.,0.125826309913858,5.85));
#44245=CARTESIAN_POINT('Ctrl Pts',(2.97480306981675,0.259872166731315,5.84552808842072));
#44246=CARTESIAN_POINT('Ctrl Pts',(2.872672019603,0.50617991633712,5.82936652378142));
#44247=CARTESIAN_POINT('Ctrl Pts',(2.79575144361404,0.61846211875906,5.81790159694625));
#44248=CARTESIAN_POINT('Ctrl Pts',(2.61845949514681,0.795754067226288,5.79631351124354));
#44249=CARTESIAN_POINT('Ctrl Pts',(2.50617841759802,0.872672585527758,5.78477457060768));
#44250=CARTESIAN_POINT('Ctrl Pts',(2.25987453785815,0.974802142157818,5.76844303881019));
#44251=CARTESIAN_POINT('Ctrl Pts',(2.12583003398973,1.,5.76389625166866));
#44252=CARTESIAN_POINT('Ctrl Pts',(2.,1.,5.76389625166866));
#44253=CARTESIAN_POINT('Ctrl Pts',(1.,1.73472347597681E-16,5.85));
#44254=CARTESIAN_POINT('Ctrl Pts',(1.,-0.125826309913858,5.85));
#44255=CARTESIAN_POINT('Ctrl Pts',(1.02519693018325,-0.259872166731316,
5.84552808842072));
#44256=CARTESIAN_POINT('Ctrl Pts',(1.127327980397,-0.506179916337121,5.82936652378142));
#44257=CARTESIAN_POINT('Ctrl Pts',(1.20424855638596,-0.61846211875906,5.81790159694625));
#44258=CARTESIAN_POINT('Ctrl Pts',(1.38154050485319,-0.795754067226289,
5.79631351124354));
#44259=CARTESIAN_POINT('Ctrl Pts',(1.49382158240198,-0.872672585527757,
5.78477457060768));
#44260=CARTESIAN_POINT('Ctrl Pts',(1.74012546214185,-0.974802142157818,
5.76844303881019));
#44261=CARTESIAN_POINT('Ctrl Pts',(1.87416996601027,-1.,5.76389625166866));
#44262=CARTESIAN_POINT('Ctrl Pts',(2.12583003398973,-1.,5.76389625166866));
#44263=CARTESIAN_POINT('Ctrl Pts',(2.25987453785815,-0.974802142157817,
5.76844303881019));
#44264=CARTESIAN_POINT('Ctrl Pts',(2.50617841759802,-0.872672585527757,
5.78477457060768));
#44265=CARTESIAN_POINT('Ctrl Pts',(2.61845949514681,-0.795754067226289,
5.79631351124354));
#44266=CARTESIAN_POINT('Ctrl Pts',(2.79575144361404,-0.61846211875906,5.81790159694625));
#44267=CARTESIAN_POINT('Ctrl Pts',(2.872672019603,-0.506179916337122,5.82936652378142));
#44268=CARTESIAN_POINT('Ctrl Pts',(2.97480306981675,-0.259872166731316,
5.84552808842072));
#44269=CARTESIAN_POINT('Ctrl Pts',(3.,-0.125826309913858,5.85));
#44270=CARTESIAN_POINT('Ctrl Pts',(3.,-2.77555756156289E-16,5.85));
#44271=CARTESIAN_POINT('Origin',(4.,-2.9217559716602,-10.1893739769462));
#44272=CARTESIAN_POINT('',(3.85,-2.9217559716602,-10.1893739769462));
#44273=CARTESIAN_POINT('',(4.,-2.9217559716602,-10.1893739769462));
#44274=CARTESIAN_POINT('',(3.85,-3.97082989020867,-9.82814885840794));
#44275=CARTESIAN_POINT('',(3.85,-3.97082989020867,-9.82814885840794));
#44276=CARTESIAN_POINT('',(4.,-3.97082989020867,-9.82814885840794));
#44277=CARTESIAN_POINT('Origin',(4.,-1.84067068326946,-10.4389621819294));
#44278=CARTESIAN_POINT('',(3.85,-1.84067068326946,-10.4389621819294));
#44279=CARTESIAN_POINT('',(4.,-1.84067068326946,-10.4389621819294));
#44280=CARTESIAN_POINT('',(3.85,-2.9217559716602,-10.1893739769462));
#44281=CARTESIAN_POINT('Origin',(4.,-0.739418621687731,-10.5741789327541));
#44282=CARTESIAN_POINT('',(3.85,-0.739418621687731,-10.5741789327541));
#44283=CARTESIAN_POINT('',(4.,-0.739418621687731,-10.5741789327541));
#44284=CARTESIAN_POINT('',(3.85,-1.84067068326946,-10.4389621819294));
#44285=CARTESIAN_POINT('Origin',(4.,0.369934665046504,-10.5935427664024));
#44286=CARTESIAN_POINT('',(3.85,0.369934665046504,-10.5935427664024));
#44287=CARTESIAN_POINT('',(4.,0.369934665046504,-10.5935427664024));
#44288=CARTESIAN_POINT('',(3.85,-0.739418621687731,-10.5741789327541));
#44289=CARTESIAN_POINT('Origin',(4.,1.47523487017669,-10.4968415286606));
#44290=CARTESIAN_POINT('',(3.85,1.47523487017669,-10.4968415286606));
#44291=CARTESIAN_POINT('',(4.,1.47523487017669,-10.4968415286606));
#44292=CARTESIAN_POINT('',(3.85,0.369934665046504,-10.5935427664024));
#44293=CARTESIAN_POINT('Origin',(4.,2.56437209335647,-10.2851346985256));
#44294=CARTESIAN_POINT('',(3.85,2.56437209335647,-10.2851346985256));
#44295=CARTESIAN_POINT('',(4.,2.56437209335647,-10.2851346985256));
#44296=CARTESIAN_POINT('',(3.85,1.47523487017669,-10.4968415286606));
#44297=CARTESIAN_POINT('Origin',(4.,1.74183764831761,-6.98612922918718));
#44298=CARTESIAN_POINT('',(3.85,1.74183764831761,-6.98612922918718));
#44299=CARTESIAN_POINT('',(4.,1.74183764831761,-6.98612922918718));
#44300=CARTESIAN_POINT('',(3.85,2.56437209335647,-10.2851346985256));
#44301=CARTESIAN_POINT('Origin',(4.,1.00204632691247,-7.12993009493931));
#44302=CARTESIAN_POINT('',(3.85,1.00204632691247,-7.12993009493931));
#44303=CARTESIAN_POINT('',(4.,1.00204632691247,-7.12993009493931));
#44304=CARTESIAN_POINT('',(3.85,1.74183764831761,-6.98612922918718));
#44305=CARTESIAN_POINT('Origin',(4.,0.251276376258003,-7.19561395453749));
#44306=CARTESIAN_POINT('',(3.85,0.251276376258003,-7.19561395453749));
#44307=CARTESIAN_POINT('',(4.,0.251276376258003,-7.19561395453749));
#44308=CARTESIAN_POINT('',(3.85,1.00204632691247,-7.12993009493931));
#44309=CARTESIAN_POINT('Origin',(4.,-0.502246610957704,-7.18246116187073));
#44310=CARTESIAN_POINT('',(3.85,-0.502246610957704,-7.18246116187073));
#44311=CARTESIAN_POINT('',(4.,-0.502246610957704,-7.18246116187073));
#44312=CARTESIAN_POINT('',(3.85,0.251276376258003,-7.19561395453749));
#44313=CARTESIAN_POINT('Origin',(4.,-1.2502668792019,-7.0906158216879));
#44314=CARTESIAN_POINT('',(3.85,-1.2502668792019,-7.0906158216879));
#44315=CARTESIAN_POINT('',(4.,-1.2502668792019,-7.0906158216879));
#44316=CARTESIAN_POINT('',(3.85,-0.502246610957704,-7.18246116187073));
#44317=CARTESIAN_POINT('Origin',(4.,-1.9845889618824,-6.92108421075589));
#44318=CARTESIAN_POINT('',(3.85,-1.9845889618824,-6.92108421075589));
#44319=CARTESIAN_POINT('',(4.,-1.9845889618824,-6.92108421075589));
#44320=CARTESIAN_POINT('',(3.85,-1.2502668792019,-7.0906158216879));
#44321=CARTESIAN_POINT('Origin',(4.,-2.69716747259457,-6.67572375288087));
#44322=CARTESIAN_POINT('',(3.85,-2.69716747259457,-6.67572375288087));
#44323=CARTESIAN_POINT('',(4.,-2.69716747259457,-6.67572375288087));
#44324=CARTESIAN_POINT('',(3.85,-1.9845889618824,-6.92108421075589));
#44325=CARTESIAN_POINT('Origin',(4.,-3.97082989020867,-9.82814885840794));
#44326=CARTESIAN_POINT('',(3.85,-2.69716747259457,-6.67572375288087));
#44327=CARTESIAN_POINT('Origin',(3.85,-0.703228898426098,-8.63463325964164));
#44328=CARTESIAN_POINT('Origin',(4.,10.2851346985256,2.56437209335648));
#44329=CARTESIAN_POINT('',(3.85,10.2851346985256,2.56437209335648));
#44330=CARTESIAN_POINT('',(4.,10.2851346985256,2.56437209335648));
#44331=CARTESIAN_POINT('',(3.85,10.4968415286606,1.47523487017669));
#44332=CARTESIAN_POINT('',(3.85,10.4968415286606,1.47523487017669));
#44333=CARTESIAN_POINT('',(4.,10.4968415286606,1.47523487017669));
#44334=CARTESIAN_POINT('Origin',(4.,9.96074178033063,3.62541351925209));
#44335=CARTESIAN_POINT('',(3.85,9.96074178033063,3.62541351925209));
#44336=CARTESIAN_POINT('',(4.,9.96074178033063,3.62541351925209));
#44337=CARTESIAN_POINT('',(3.85,10.2851346985256,2.56437209335648));
#44338=CARTESIAN_POINT('Origin',(4.,9.52721689077117,4.64673415596422));
#44339=CARTESIAN_POINT('',(3.85,9.52721689077117,4.64673415596422));
#44340=CARTESIAN_POINT('',(4.,9.52721689077117,4.64673415596422));
#44341=CARTESIAN_POINT('',(3.85,9.96074178033063,3.62541351925209));
#44342=CARTESIAN_POINT('Origin',(4.,8.98930981925811,5.61714420087197));
#44343=CARTESIAN_POINT('',(3.85,8.98930981925811,5.61714420087197));
#44344=CARTESIAN_POINT('',(4.,8.98930981925811,5.61714420087197));
#44345=CARTESIAN_POINT('',(3.85,9.52721689077117,4.64673415596422));
#44346=CARTESIAN_POINT('Origin',(4.,8.35291398823125,6.52601163845198));
#44347=CARTESIAN_POINT('',(3.85,8.35291398823125,6.52601163845198));
#44348=CARTESIAN_POINT('',(4.,8.35291398823125,6.52601163845198));
#44349=CARTESIAN_POINT('',(3.85,8.98930981925811,5.61714420087197));
#44350=CARTESIAN_POINT('Origin',(4.,7.6250018835897,7.36337872686537));
#44351=CARTESIAN_POINT('',(3.85,7.6250018835897,7.36337872686537));
#44352=CARTESIAN_POINT('',(4.,7.6250018835897,7.36337872686537));
#44353=CARTESIAN_POINT('',(3.85,8.35291398823125,6.52601163845198));
#44354=CARTESIAN_POINT('Origin',(4.,5.17924656243829,5.00154026730478));
#44355=CARTESIAN_POINT('',(3.85,5.17924656243829,5.00154026730478));
#44356=CARTESIAN_POINT('',(4.,5.17924656243829,5.00154026730478));
#44357=CARTESIAN_POINT('',(3.85,7.6250018835897,7.36337872686537));
#44358=CARTESIAN_POINT('Origin',(4.,5.6736774259684,4.43276262234474));
#44359=CARTESIAN_POINT('',(3.85,5.6736774259684,4.43276262234474));
#44360=CARTESIAN_POINT('',(4.,5.6736774259684,4.43276262234474));
#44361=CARTESIAN_POINT('',(3.85,5.17924656243829,5.00154026730478));
#44362=CARTESIAN_POINT('Origin',(4.,6.10594629232627,3.81541870247908));
#44363=CARTESIAN_POINT('',(3.85,6.10594629232627,3.81541870247908));
#44364=CARTESIAN_POINT('',(4.,6.10594629232627,3.81541870247908));
#44365=CARTESIAN_POINT('',(3.85,5.6736774259684,4.43276262234474));
#44366=CARTESIAN_POINT('Origin',(4.,6.471317133354,3.15627225688136));
#44367=CARTESIAN_POINT('',(3.85,6.471317133354,3.15627225688136));
#44368=CARTESIAN_POINT('',(4.,6.471317133354,3.15627225688136));
#44369=CARTESIAN_POINT('',(3.85,6.10594629232627,3.81541870247908));
#44370=CARTESIAN_POINT('Origin',(4.,6.76578686965854,2.46254503194481));
#44371=CARTESIAN_POINT('',(3.85,6.76578686965854,2.46254503194481));
#44372=CARTESIAN_POINT('',(4.,6.76578686965854,2.46254503194481));
#44373=CARTESIAN_POINT('',(3.85,6.471317133354,3.15627225688136));
#44374=CARTESIAN_POINT('Origin',(4.,6.98612922918717,1.74183764831761));
#44375=CARTESIAN_POINT('',(3.85,6.98612922918717,1.74183764831761));
#44376=CARTESIAN_POINT('',(4.,6.98612922918717,1.74183764831761));
#44377=CARTESIAN_POINT('',(3.85,6.76578686965854,2.46254503194481));
#44378=CARTESIAN_POINT('Origin',(4.,7.12993009493931,1.00204632691247));
#44379=CARTESIAN_POINT('',(3.85,7.12993009493931,1.00204632691247));
#44380=CARTESIAN_POINT('',(4.,7.12993009493931,1.00204632691247));
#44381=CARTESIAN_POINT('',(3.85,6.98612922918717,1.74183764831761));
#44382=CARTESIAN_POINT('Origin',(4.,10.4968415286606,1.47523487017669));
#44383=CARTESIAN_POINT('',(3.85,7.12993009493931,1.00204632691247));
#44384=CARTESIAN_POINT('Origin',(3.85,7.83804404554947,4.18271252688892));
#44385=CARTESIAN_POINT('Origin',(4.,2.92175597166019,10.1893739769462));
#44386=CARTESIAN_POINT('',(3.85,2.92175597166019,10.1893739769462));
#44387=CARTESIAN_POINT('',(4.,2.92175597166019,10.1893739769462));
#44388=CARTESIAN_POINT('',(3.85,3.97082989020867,9.82814885840795));
#44389=CARTESIAN_POINT('',(3.85,3.97082989020867,9.82814885840795));
#44390=CARTESIAN_POINT('',(4.,3.97082989020867,9.82814885840795));
#44391=CARTESIAN_POINT('Origin',(4.,1.84067068326946,10.4389621819294));
#44392=CARTESIAN_POINT('',(3.85,1.84067068326946,10.4389621819294));
#44393=CARTESIAN_POINT('',(4.,1.84067068326946,10.4389621819294));
#44394=CARTESIAN_POINT('',(3.85,2.92175597166019,10.1893739769462));
#44395=CARTESIAN_POINT('Origin',(4.,0.739418621687727,10.5741789327541));
#44396=CARTESIAN_POINT('',(3.85,0.739418621687727,10.5741789327541));
#44397=CARTESIAN_POINT('',(4.,0.739418621687727,10.5741789327541));
#44398=CARTESIAN_POINT('',(3.85,1.84067068326946,10.4389621819294));
#44399=CARTESIAN_POINT('Origin',(4.,-0.36993466504651,10.5935427664024));
#44400=CARTESIAN_POINT('',(3.85,-0.36993466504651,10.5935427664024));
#44401=CARTESIAN_POINT('',(4.,-0.36993466504651,10.5935427664024));
#44402=CARTESIAN_POINT('',(3.85,0.739418621687727,10.5741789327541));
#44403=CARTESIAN_POINT('Origin',(4.,-1.4752348701767,10.4968415286606));
#44404=CARTESIAN_POINT('',(3.85,-1.47523487017669,10.4968415286606));
#44405=CARTESIAN_POINT('',(4.,-1.4752348701767,10.4968415286606));
#44406=CARTESIAN_POINT('',(3.85,-0.36993466504651,10.5935427664024));
#44407=CARTESIAN_POINT('Origin',(4.,-2.56437209335648,10.2851346985256));
#44408=CARTESIAN_POINT('',(3.85,-2.56437209335648,10.2851346985256));
#44409=CARTESIAN_POINT('',(4.,-2.56437209335648,10.2851346985256));
#44410=CARTESIAN_POINT('',(3.85,-1.4752348701767,10.4968415286606));
#44411=CARTESIAN_POINT('Origin',(4.,-1.74183764831761,6.98612922918717));
#44412=CARTESIAN_POINT('',(3.85,-1.74183764831761,6.98612922918717));
#44413=CARTESIAN_POINT('',(4.,-1.74183764831761,6.98612922918717));
#44414=CARTESIAN_POINT('',(3.85,-2.56437209335648,10.2851346985256));
#44415=CARTESIAN_POINT('Origin',(4.,-1.00204632691247,7.12993009493931));
#44416=CARTESIAN_POINT('',(3.85,-1.00204632691247,7.12993009493931));
#44417=CARTESIAN_POINT('',(4.,-1.00204632691247,7.12993009493931));
#44418=CARTESIAN_POINT('',(3.85,-1.74183764831761,6.98612922918717));
#44419=CARTESIAN_POINT('Origin',(4.,-0.251276376258007,7.19561395453749));
#44420=CARTESIAN_POINT('',(3.85,-0.251276376258007,7.19561395453749));
#44421=CARTESIAN_POINT('',(4.,-0.251276376258007,7.19561395453749));
#44422=CARTESIAN_POINT('',(3.85,-1.00204632691247,7.12993009493931));
#44423=CARTESIAN_POINT('Origin',(4.,0.502246610957702,7.18246116187073));
#44424=CARTESIAN_POINT('',(3.85,0.502246610957702,7.18246116187073));
#44425=CARTESIAN_POINT('',(4.,0.502246610957702,7.18246116187073));
#44426=CARTESIAN_POINT('',(3.85,-0.251276376258007,7.19561395453749));
#44427=CARTESIAN_POINT('Origin',(4.,1.2502668792019,7.0906158216879));
#44428=CARTESIAN_POINT('',(3.85,1.2502668792019,7.0906158216879));
#44429=CARTESIAN_POINT('',(4.,1.2502668792019,7.0906158216879));
#44430=CARTESIAN_POINT('',(3.85,0.502246610957702,7.18246116187073));
#44431=CARTESIAN_POINT('Origin',(4.,1.98458896188239,6.9210842107559));
#44432=CARTESIAN_POINT('',(3.85,1.98458896188239,6.9210842107559));
#44433=CARTESIAN_POINT('',(4.,1.98458896188239,6.9210842107559));
#44434=CARTESIAN_POINT('',(3.85,1.2502668792019,7.0906158216879));
#44435=CARTESIAN_POINT('Origin',(4.,2.69716747259457,6.67572375288087));
#44436=CARTESIAN_POINT('',(3.85,2.69716747259457,6.67572375288087));
#44437=CARTESIAN_POINT('',(4.,2.69716747259457,6.67572375288087));
#44438=CARTESIAN_POINT('',(3.85,1.98458896188239,6.9210842107559));
#44439=CARTESIAN_POINT('Origin',(4.,3.97082989020867,9.82814885840795));
#44440=CARTESIAN_POINT('',(3.85,2.69716747259457,6.67572375288087));
#44441=CARTESIAN_POINT('Origin',(3.85,0.703228898426094,8.63463325964164));
#44442=CARTESIAN_POINT('Origin',(4.,-7.36337872686537,7.6250018835897));
#44443=CARTESIAN_POINT('',(3.85,-7.36337872686537,7.6250018835897));
#44444=CARTESIAN_POINT('',(4.,-7.36337872686537,7.6250018835897));
#44445=CARTESIAN_POINT('',(3.85,-6.52601163845198,8.35291398823125));
#44446=CARTESIAN_POINT('',(3.85,-6.52601163845198,8.35291398823125));
#44447=CARTESIAN_POINT('',(4.,-6.52601163845198,8.35291398823125));
#44448=CARTESIAN_POINT('Origin',(4.,-8.12007109706117,6.81354866267732));
#44449=CARTESIAN_POINT('',(3.85,-8.12007109706117,6.81354866267732));
#44450=CARTESIAN_POINT('',(4.,-8.12007109706117,6.81354866267732));
#44451=CARTESIAN_POINT('',(3.85,-7.36337872686537,7.6250018835897));
#44452=CARTESIAN_POINT('Origin',(4.,-8.78779826908344,5.92744477678992));
#44453=CARTESIAN_POINT('',(3.85,-8.78779826908344,5.92744477678992));
#44454=CARTESIAN_POINT('',(4.,-8.78779826908344,5.92744477678992));
#44455=CARTESIAN_POINT('',(3.85,-8.12007109706117,6.81354866267732));
#44456=CARTESIAN_POINT('Origin',(4.,-9.35924448430463,4.97639856553044));
#44457=CARTESIAN_POINT('',(3.85,-9.35924448430463,4.97639856553044));
#44458=CARTESIAN_POINT('',(4.,-9.35924448430463,4.97639856553044));
#44459=CARTESIAN_POINT('',(3.85,-8.78779826908344,5.92744477678992));
#44460=CARTESIAN_POINT('Origin',(4.,-9.82814885840794,3.97082989020867));
#44461=CARTESIAN_POINT('',(3.85,-9.82814885840794,3.97082989020867));
#44462=CARTESIAN_POINT('',(4.,-9.82814885840794,3.97082989020867));
#44463=CARTESIAN_POINT('',(3.85,-9.35924448430463,4.97639856553044));
#44464=CARTESIAN_POINT('Origin',(4.,-10.1893739769462,2.92175597166019));
#44465=CARTESIAN_POINT('',(3.85,-10.1893739769462,2.92175597166019));
#44466=CARTESIAN_POINT('',(4.,-10.1893739769462,2.92175597166019));
#44467=CARTESIAN_POINT('',(3.85,-9.82814885840794,3.97082989020867));
#44468=CARTESIAN_POINT('Origin',(4.,-6.9210842107559,1.98458896188239));
#44469=CARTESIAN_POINT('',(3.85,-6.9210842107559,1.98458896188239));
#44470=CARTESIAN_POINT('',(4.,-6.9210842107559,1.98458896188239));
#44471=CARTESIAN_POINT('',(3.85,-10.1893739769462,2.92175597166019));
#44472=CARTESIAN_POINT('Origin',(4.,-6.67572375288087,2.69716747259457));
#44473=CARTESIAN_POINT('',(3.85,-6.67572375288087,2.69716747259457));
#44474=CARTESIAN_POINT('',(4.,-6.67572375288087,2.69716747259457));
#44475=CARTESIAN_POINT('',(3.85,-6.9210842107559,1.98458896188239));
#44476=CARTESIAN_POINT('Origin',(4.,-6.35722266858427,3.38019525205841));
#44477=CARTESIAN_POINT('',(3.85,-6.35722266858427,3.38019525205841));
#44478=CARTESIAN_POINT('',(4.,-6.35722266858427,3.38019525205841));
#44479=CARTESIAN_POINT('',(3.85,-6.67572375288087,2.69716747259457));
#44480=CARTESIAN_POINT('Origin',(4.,-5.9690705223963,4.02618890498938));
#44481=CARTESIAN_POINT('',(3.85,-5.9690705223963,4.02618890498938));
#44482=CARTESIAN_POINT('',(4.,-5.9690705223963,4.02618890498938));
#44483=CARTESIAN_POINT('',(3.85,-6.35722266858427,3.38019525205841));
#44484=CARTESIAN_POINT('Origin',(4.,-5.51551999045664,4.62807078974308));
#44485=CARTESIAN_POINT('',(3.85,-5.51551999045664,4.62807078974308));
#44486=CARTESIAN_POINT('',(4.,-5.51551999045664,4.62807078974308));
#44487=CARTESIAN_POINT('',(3.85,-5.9690705223963,4.02618890498938));
#44488=CARTESIAN_POINT('Origin',(4.,-5.00154026730478,5.17924656243829));
#44489=CARTESIAN_POINT('',(3.85,-5.00154026730478,5.17924656243829));
#44490=CARTESIAN_POINT('',(4.,-5.00154026730478,5.17924656243829));
#44491=CARTESIAN_POINT('',(3.85,-5.51551999045664,4.62807078974308));
#44492=CARTESIAN_POINT('Origin',(4.,-4.43276262234474,5.6736774259684));
#44493=CARTESIAN_POINT('',(3.85,-4.43276262234474,5.6736774259684));
#44494=CARTESIAN_POINT('',(4.,-4.43276262234474,5.6736774259684));
#44495=CARTESIAN_POINT('',(3.85,-5.00154026730478,5.17924656243829));
#44496=CARTESIAN_POINT('Origin',(4.,-6.52601163845198,8.35291398823125));
#44497=CARTESIAN_POINT('',(3.85,-4.43276262234474,5.6736774259684));
#44498=CARTESIAN_POINT('Origin',(3.85,-7.31106829964546,5.16875147505682));
#44499=CARTESIAN_POINT('Origin',(4.,-10.2851346985256,-2.56437209335648));
#44500=CARTESIAN_POINT('',(3.85,-10.2851346985256,-2.56437209335648));
#44501=CARTESIAN_POINT('',(4.,-10.2851346985256,-2.56437209335648));
#44502=CARTESIAN_POINT('',(3.85,-10.4968415286606,-1.47523487017669));
#44503=CARTESIAN_POINT('',(3.85,-10.4968415286606,-1.47523487017669));
#44504=CARTESIAN_POINT('',(4.,-10.4968415286606,-1.47523487017669));
#44505=CARTESIAN_POINT('Origin',(4.,-9.96074178033063,-3.62541351925209));
#44506=CARTESIAN_POINT('',(3.85,-9.96074178033063,-3.62541351925209));
#44507=CARTESIAN_POINT('',(4.,-9.96074178033063,-3.62541351925209));
#44508=CARTESIAN_POINT('',(3.85,-10.2851346985256,-2.56437209335648));
#44509=CARTESIAN_POINT('Origin',(4.,-9.52721689077117,-4.64673415596422));
#44510=CARTESIAN_POINT('',(3.85,-9.52721689077117,-4.64673415596422));
#44511=CARTESIAN_POINT('',(4.,-9.52721689077117,-4.64673415596422));
#44512=CARTESIAN_POINT('',(3.85,-9.96074178033063,-3.62541351925209));
#44513=CARTESIAN_POINT('Origin',(4.,-8.98930981925811,-5.61714420087197));
#44514=CARTESIAN_POINT('',(3.85,-8.98930981925811,-5.61714420087197));
#44515=CARTESIAN_POINT('',(4.,-8.98930981925811,-5.61714420087197));
#44516=CARTESIAN_POINT('',(3.85,-9.52721689077117,-4.64673415596422));
#44517=CARTESIAN_POINT('Origin',(4.,-8.35291398823125,-6.52601163845198));
#44518=CARTESIAN_POINT('',(3.85,-8.35291398823125,-6.52601163845198));
#44519=CARTESIAN_POINT('',(4.,-8.35291398823125,-6.52601163845198));
#44520=CARTESIAN_POINT('',(3.85,-8.98930981925811,-5.61714420087197));
#44521=CARTESIAN_POINT('Origin',(4.,-7.6250018835897,-7.36337872686537));
#44522=CARTESIAN_POINT('',(3.85,-7.6250018835897,-7.36337872686537));
#44523=CARTESIAN_POINT('',(4.,-7.6250018835897,-7.36337872686537));
#44524=CARTESIAN_POINT('',(3.85,-8.35291398823125,-6.52601163845198));
#44525=CARTESIAN_POINT('Origin',(4.,-5.17924656243829,-5.00154026730478));
#44526=CARTESIAN_POINT('',(3.85,-5.17924656243829,-5.00154026730478));
#44527=CARTESIAN_POINT('',(4.,-5.17924656243829,-5.00154026730478));
#44528=CARTESIAN_POINT('',(3.85,-7.6250018835897,-7.36337872686537));
#44529=CARTESIAN_POINT('Origin',(4.,-5.6736774259684,-4.43276262234474));
#44530=CARTESIAN_POINT('',(3.85,-5.6736774259684,-4.43276262234474));
#44531=CARTESIAN_POINT('',(4.,-5.6736774259684,-4.43276262234474));
#44532=CARTESIAN_POINT('',(3.85,-5.17924656243829,-5.00154026730478));
#44533=CARTESIAN_POINT('Origin',(4.,-6.10594629232627,-3.81541870247908));
#44534=CARTESIAN_POINT('',(3.85,-6.10594629232627,-3.81541870247908));
#44535=CARTESIAN_POINT('',(4.,-6.10594629232627,-3.81541870247908));
#44536=CARTESIAN_POINT('',(3.85,-5.6736774259684,-4.43276262234474));
#44537=CARTESIAN_POINT('Origin',(4.,-6.471317133354,-3.15627225688136));
#44538=CARTESIAN_POINT('',(3.85,-6.471317133354,-3.15627225688136));
#44539=CARTESIAN_POINT('',(4.,-6.471317133354,-3.15627225688136));
#44540=CARTESIAN_POINT('',(3.85,-6.10594629232627,-3.81541870247908));
#44541=CARTESIAN_POINT('Origin',(4.,-6.76578686965854,-2.46254503194481));
#44542=CARTESIAN_POINT('',(3.85,-6.76578686965854,-2.46254503194481));
#44543=CARTESIAN_POINT('',(4.,-6.76578686965854,-2.46254503194481));
#44544=CARTESIAN_POINT('',(3.85,-6.471317133354,-3.15627225688136));
#44545=CARTESIAN_POINT('Origin',(4.,-6.98612922918717,-1.74183764831761));
#44546=CARTESIAN_POINT('',(3.85,-6.98612922918717,-1.74183764831761));
#44547=CARTESIAN_POINT('',(4.,-6.98612922918717,-1.74183764831761));
#44548=CARTESIAN_POINT('',(3.85,-6.76578686965854,-2.46254503194481));
#44549=CARTESIAN_POINT('Origin',(4.,-7.12993009493931,-1.00204632691247));
#44550=CARTESIAN_POINT('',(3.85,-7.12993009493931,-1.00204632691247));
#44551=CARTESIAN_POINT('',(4.,-7.12993009493931,-1.00204632691247));
#44552=CARTESIAN_POINT('',(3.85,-6.98612922918717,-1.74183764831761));
#44553=CARTESIAN_POINT('Origin',(4.,-10.4968415286606,-1.47523487017669));
#44554=CARTESIAN_POINT('',(3.85,-7.12993009493931,-1.00204632691247));
#44555=CARTESIAN_POINT('Origin',(3.85,-7.83804404554947,-4.18271252688892));
#44556=CARTESIAN_POINT('Origin',(4.,7.36337872686537,-7.6250018835897));
#44557=CARTESIAN_POINT('',(3.85,7.36337872686537,-7.6250018835897));
#44558=CARTESIAN_POINT('',(4.,7.36337872686537,-7.6250018835897));
#44559=CARTESIAN_POINT('',(3.85,6.52601163845198,-8.35291398823125));
#44560=CARTESIAN_POINT('',(3.85,6.52601163845198,-8.35291398823125));
#44561=CARTESIAN_POINT('',(4.,6.52601163845198,-8.35291398823125));
#44562=CARTESIAN_POINT('Origin',(4.,8.12007109706117,-6.81354866267731));
#44563=CARTESIAN_POINT('',(3.85,8.12007109706117,-6.81354866267731));
#44564=CARTESIAN_POINT('',(4.,8.12007109706117,-6.81354866267731));
#44565=CARTESIAN_POINT('',(3.85,7.36337872686537,-7.6250018835897));
#44566=CARTESIAN_POINT('Origin',(4.,8.78779826908344,-5.92744477678991));
#44567=CARTESIAN_POINT('',(3.85,8.78779826908344,-5.92744477678991));
#44568=CARTESIAN_POINT('',(4.,8.78779826908344,-5.92744477678991));
#44569=CARTESIAN_POINT('',(3.85,8.12007109706117,-6.81354866267731));
#44570=CARTESIAN_POINT('Origin',(4.,9.35924448430463,-4.97639856553044));
#44571=CARTESIAN_POINT('',(3.85,9.35924448430463,-4.97639856553044));
#44572=CARTESIAN_POINT('',(4.,9.35924448430463,-4.97639856553044));
#44573=CARTESIAN_POINT('',(3.85,8.78779826908344,-5.92744477678991));
#44574=CARTESIAN_POINT('Origin',(4.,9.82814885840795,-3.97082989020866));
#44575=CARTESIAN_POINT('',(3.85,9.82814885840795,-3.97082989020866));
#44576=CARTESIAN_POINT('',(4.,9.82814885840795,-3.97082989020866));
#44577=CARTESIAN_POINT('',(3.85,9.35924448430463,-4.97639856553044));
#44578=CARTESIAN_POINT('Origin',(4.,10.1893739769462,-2.92175597166019));
#44579=CARTESIAN_POINT('',(3.85,10.1893739769462,-2.92175597166019));
#44580=CARTESIAN_POINT('',(4.,10.1893739769462,-2.92175597166019));
#44581=CARTESIAN_POINT('',(3.85,9.82814885840795,-3.97082989020866));
#44582=CARTESIAN_POINT('Origin',(4.,6.9210842107559,-1.98458896188239));
#44583=CARTESIAN_POINT('',(3.85,6.9210842107559,-1.98458896188239));
#44584=CARTESIAN_POINT('',(4.,6.9210842107559,-1.98458896188239));
#44585=CARTESIAN_POINT('',(3.85,10.1893739769462,-2.92175597166019));
#44586=CARTESIAN_POINT('Origin',(4.,6.67572375288087,-2.69716747259456));
#44587=CARTESIAN_POINT('',(3.85,6.67572375288087,-2.69716747259456));
#44588=CARTESIAN_POINT('',(4.,6.67572375288087,-2.69716747259456));
#44589=CARTESIAN_POINT('',(3.85,6.9210842107559,-1.98458896188239));
#44590=CARTESIAN_POINT('Origin',(4.,6.35722266858427,-3.38019525205841));
#44591=CARTESIAN_POINT('',(3.85,6.35722266858427,-3.38019525205841));
#44592=CARTESIAN_POINT('',(4.,6.35722266858427,-3.38019525205841));
#44593=CARTESIAN_POINT('',(3.85,6.67572375288087,-2.69716747259456));
#44594=CARTESIAN_POINT('Origin',(4.,5.9690705223963,-4.02618890498938));
#44595=CARTESIAN_POINT('',(3.85,5.9690705223963,-4.02618890498938));
#44596=CARTESIAN_POINT('',(4.,5.9690705223963,-4.02618890498938));
#44597=CARTESIAN_POINT('',(3.85,6.35722266858427,-3.38019525205841));
#44598=CARTESIAN_POINT('Origin',(4.,5.51551999045664,-4.62807078974308));
#44599=CARTESIAN_POINT('',(3.85,5.51551999045664,-4.62807078974308));
#44600=CARTESIAN_POINT('',(4.,5.51551999045664,-4.62807078974308));
#44601=CARTESIAN_POINT('',(3.85,5.9690705223963,-4.02618890498938));
#44602=CARTESIAN_POINT('Origin',(4.,5.00154026730478,-5.17924656243829));
#44603=CARTESIAN_POINT('',(3.85,5.00154026730478,-5.17924656243829));
#44604=CARTESIAN_POINT('',(4.,5.00154026730478,-5.17924656243829));
#44605=CARTESIAN_POINT('',(3.85,5.51551999045664,-4.62807078974308));
#44606=CARTESIAN_POINT('Origin',(4.,4.43276262234474,-5.6736774259684));
#44607=CARTESIAN_POINT('',(3.85,4.43276262234474,-5.6736774259684));
#44608=CARTESIAN_POINT('',(4.,4.43276262234474,-5.6736774259684));
#44609=CARTESIAN_POINT('',(3.85,5.00154026730478,-5.17924656243829));
#44610=CARTESIAN_POINT('Origin',(4.,6.52601163845198,-8.35291398823125));
#44611=CARTESIAN_POINT('',(3.85,4.43276262234474,-5.6736774259684));
#44612=CARTESIAN_POINT('Origin',(3.85,7.31106829964546,-5.16875147505682));
#44613=CARTESIAN_POINT('Origin',(0.,-1.9845889618824,-6.92108421075589));
#44614=CARTESIAN_POINT('',(0.15,-1.9845889618824,-6.92108421075589));
#44615=CARTESIAN_POINT('',(0.,-1.9845889618824,-6.92108421075589));
#44616=CARTESIAN_POINT('',(0.15,-2.69716747259457,-6.67572375288087));
#44617=CARTESIAN_POINT('',(0.15,-1.9845889618824,-6.92108421075589));
#44618=CARTESIAN_POINT('',(0.,-2.69716747259457,-6.67572375288087));
#44619=CARTESIAN_POINT('Origin',(0.,-1.2502668792019,-7.0906158216879));
#44620=CARTESIAN_POINT('',(0.15,-1.2502668792019,-7.0906158216879));
#44621=CARTESIAN_POINT('',(0.,-1.2502668792019,-7.0906158216879));
#44622=CARTESIAN_POINT('',(0.15,-1.2502668792019,-7.0906158216879));
#44623=CARTESIAN_POINT('Origin',(0.,-0.502246610957704,-7.18246116187073));
#44624=CARTESIAN_POINT('',(0.15,-0.502246610957704,-7.18246116187073));
#44625=CARTESIAN_POINT('',(0.,-0.502246610957704,-7.18246116187073));
#44626=CARTESIAN_POINT('',(0.15,-0.502246610957704,-7.18246116187073));
#44627=CARTESIAN_POINT('Origin',(0.,0.251276376258003,-7.19561395453749));
#44628=CARTESIAN_POINT('',(0.15,0.251276376258003,-7.19561395453749));
#44629=CARTESIAN_POINT('',(0.,0.251276376258003,-7.19561395453749));
#44630=CARTESIAN_POINT('',(0.15,0.251276376258003,-7.19561395453749));
#44631=CARTESIAN_POINT('Origin',(0.,1.00204632691247,-7.12993009493931));
#44632=CARTESIAN_POINT('',(0.15,1.00204632691247,-7.12993009493931));
#44633=CARTESIAN_POINT('',(0.,1.00204632691247,-7.12993009493931));
#44634=CARTESIAN_POINT('',(0.15,1.00204632691247,-7.12993009493931));
#44635=CARTESIAN_POINT('Origin',(0.,1.74183764831761,-6.98612922918718));
#44636=CARTESIAN_POINT('',(0.15,1.74183764831761,-6.98612922918718));
#44637=CARTESIAN_POINT('',(0.,1.74183764831761,-6.98612922918718));
#44638=CARTESIAN_POINT('',(0.15,1.74183764831761,-6.98612922918718));
#44639=CARTESIAN_POINT('Origin',(0.,2.56437209335647,-10.2851346985256));
#44640=CARTESIAN_POINT('',(0.15,2.56437209335647,-10.2851346985256));
#44641=CARTESIAN_POINT('',(0.,2.56437209335647,-10.2851346985256));
#44642=CARTESIAN_POINT('',(0.15,2.56437209335647,-10.2851346985256));
#44643=CARTESIAN_POINT('Origin',(0.,1.47523487017669,-10.4968415286606));
#44644=CARTESIAN_POINT('',(0.15,1.47523487017669,-10.4968415286606));
#44645=CARTESIAN_POINT('',(0.,1.47523487017669,-10.4968415286606));
#44646=CARTESIAN_POINT('',(0.15,1.47523487017669,-10.4968415286606));
#44647=CARTESIAN_POINT('Origin',(0.,0.369934665046504,-10.5935427664024));
#44648=CARTESIAN_POINT('',(0.15,0.369934665046504,-10.5935427664024));
#44649=CARTESIAN_POINT('',(0.,0.369934665046504,-10.5935427664024));
#44650=CARTESIAN_POINT('',(0.15,0.369934665046504,-10.5935427664024));
#44651=CARTESIAN_POINT('Origin',(0.,-0.739418621687731,-10.5741789327541));
#44652=CARTESIAN_POINT('',(0.15,-0.739418621687731,-10.5741789327541));
#44653=CARTESIAN_POINT('',(0.,-0.739418621687731,-10.5741789327541));
#44654=CARTESIAN_POINT('',(0.15,-0.739418621687731,-10.5741789327541));
#44655=CARTESIAN_POINT('Origin',(0.,-1.84067068326946,-10.4389621819294));
#44656=CARTESIAN_POINT('',(0.15,-1.84067068326946,-10.4389621819294));
#44657=CARTESIAN_POINT('',(0.,-1.84067068326946,-10.4389621819294));
#44658=CARTESIAN_POINT('',(0.15,-1.84067068326946,-10.4389621819294));
#44659=CARTESIAN_POINT('Origin',(0.,-2.9217559716602,-10.1893739769462));
#44660=CARTESIAN_POINT('',(0.15,-2.9217559716602,-10.1893739769462));
#44661=CARTESIAN_POINT('',(0.,-2.9217559716602,-10.1893739769462));
#44662=CARTESIAN_POINT('',(0.15,-2.9217559716602,-10.1893739769462));
#44663=CARTESIAN_POINT('Origin',(0.,-3.97082989020867,-9.82814885840794));
#44664=CARTESIAN_POINT('',(0.15,-3.97082989020867,-9.82814885840794));
#44665=CARTESIAN_POINT('',(0.,-3.97082989020867,-9.82814885840794));
#44666=CARTESIAN_POINT('',(0.15,-3.97082989020867,-9.82814885840794));
#44667=CARTESIAN_POINT('Origin',(0.,-2.69716747259457,-6.67572375288087));
#44668=CARTESIAN_POINT('',(0.15,-2.69716747259457,-6.67572375288087));
#44669=CARTESIAN_POINT('Origin',(0.15,-0.703228898426098,-8.63463325964164));
#44670=CARTESIAN_POINT('Origin',(0.,6.98612922918717,1.74183764831761));
#44671=CARTESIAN_POINT('',(0.15,6.98612922918717,1.74183764831761));
#44672=CARTESIAN_POINT('',(0.,6.98612922918717,1.74183764831761));
#44673=CARTESIAN_POINT('',(0.15,7.12993009493931,1.00204632691247));
#44674=CARTESIAN_POINT('',(0.15,6.98612922918717,1.74183764831761));
#44675=CARTESIAN_POINT('',(0.,7.12993009493931,1.00204632691247));
#44676=CARTESIAN_POINT('Origin',(0.,6.76578686965854,2.46254503194481));
#44677=CARTESIAN_POINT('',(0.15,6.76578686965854,2.46254503194481));
#44678=CARTESIAN_POINT('',(0.,6.76578686965854,2.46254503194481));
#44679=CARTESIAN_POINT('',(0.15,6.76578686965854,2.46254503194481));
#44680=CARTESIAN_POINT('Origin',(0.,6.471317133354,3.15627225688136));
#44681=CARTESIAN_POINT('',(0.15,6.471317133354,3.15627225688136));
#44682=CARTESIAN_POINT('',(0.,6.471317133354,3.15627225688136));
#44683=CARTESIAN_POINT('',(0.15,6.471317133354,3.15627225688136));
#44684=CARTESIAN_POINT('Origin',(0.,6.10594629232627,3.81541870247908));
#44685=CARTESIAN_POINT('',(0.15,6.10594629232627,3.81541870247908));
#44686=CARTESIAN_POINT('',(0.,6.10594629232627,3.81541870247908));
#44687=CARTESIAN_POINT('',(0.15,6.10594629232627,3.81541870247908));
#44688=CARTESIAN_POINT('Origin',(0.,5.6736774259684,4.43276262234474));
#44689=CARTESIAN_POINT('',(0.15,5.6736774259684,4.43276262234474));
#44690=CARTESIAN_POINT('',(0.,5.6736774259684,4.43276262234474));
#44691=CARTESIAN_POINT('',(0.15,5.6736774259684,4.43276262234474));
#44692=CARTESIAN_POINT('Origin',(0.,5.17924656243829,5.00154026730478));
#44693=CARTESIAN_POINT('',(0.15,5.17924656243829,5.00154026730478));
#44694=CARTESIAN_POINT('',(0.,5.17924656243829,5.00154026730478));
#44695=CARTESIAN_POINT('',(0.15,5.17924656243829,5.00154026730478));
#44696=CARTESIAN_POINT('Origin',(0.,7.6250018835897,7.36337872686537));
#44697=CARTESIAN_POINT('',(0.15,7.6250018835897,7.36337872686537));
#44698=CARTESIAN_POINT('',(0.,7.6250018835897,7.36337872686537));
#44699=CARTESIAN_POINT('',(0.15,7.6250018835897,7.36337872686537));
#44700=CARTESIAN_POINT('Origin',(0.,8.35291398823125,6.52601163845198));
#44701=CARTESIAN_POINT('',(0.15,8.35291398823125,6.52601163845198));
#44702=CARTESIAN_POINT('',(0.,8.35291398823125,6.52601163845198));
#44703=CARTESIAN_POINT('',(0.15,8.35291398823125,6.52601163845198));
#44704=CARTESIAN_POINT('Origin',(0.,8.98930981925811,5.61714420087197));
#44705=CARTESIAN_POINT('',(0.15,8.98930981925811,5.61714420087197));
#44706=CARTESIAN_POINT('',(0.,8.98930981925811,5.61714420087197));
#44707=CARTESIAN_POINT('',(0.15,8.98930981925811,5.61714420087197));
#44708=CARTESIAN_POINT('Origin',(0.,9.52721689077117,4.64673415596422));
#44709=CARTESIAN_POINT('',(0.15,9.52721689077117,4.64673415596422));
#44710=CARTESIAN_POINT('',(0.,9.52721689077117,4.64673415596422));
#44711=CARTESIAN_POINT('',(0.15,9.52721689077117,4.64673415596422));
#44712=CARTESIAN_POINT('Origin',(0.,9.96074178033063,3.62541351925209));
#44713=CARTESIAN_POINT('',(0.15,9.96074178033063,3.62541351925209));
#44714=CARTESIAN_POINT('',(0.,9.96074178033063,3.62541351925209));
#44715=CARTESIAN_POINT('',(0.15,9.96074178033063,3.62541351925209));
#44716=CARTESIAN_POINT('Origin',(0.,10.2851346985256,2.56437209335648));
#44717=CARTESIAN_POINT('',(0.15,10.2851346985256,2.56437209335648));
#44718=CARTESIAN_POINT('',(0.,10.2851346985256,2.56437209335648));
#44719=CARTESIAN_POINT('',(0.15,10.2851346985256,2.56437209335648));
#44720=CARTESIAN_POINT('Origin',(0.,10.4968415286606,1.47523487017669));
#44721=CARTESIAN_POINT('',(0.15,10.4968415286606,1.47523487017669));
#44722=CARTESIAN_POINT('',(0.,10.4968415286606,1.47523487017669));
#44723=CARTESIAN_POINT('',(0.15,10.4968415286606,1.47523487017669));
#44724=CARTESIAN_POINT('Origin',(0.,7.12993009493931,1.00204632691247));
#44725=CARTESIAN_POINT('',(0.15,7.12993009493931,1.00204632691247));
#44726=CARTESIAN_POINT('Origin',(0.15,7.83804404554947,4.18271252688892));
#44727=CARTESIAN_POINT('Origin',(0.,1.98458896188239,6.9210842107559));
#44728=CARTESIAN_POINT('',(0.15,1.98458896188239,6.9210842107559));
#44729=CARTESIAN_POINT('',(0.,1.98458896188239,6.9210842107559));
#44730=CARTESIAN_POINT('',(0.15,2.69716747259457,6.67572375288087));
#44731=CARTESIAN_POINT('',(0.15,1.98458896188239,6.9210842107559));
#44732=CARTESIAN_POINT('',(0.,2.69716747259457,6.67572375288087));
#44733=CARTESIAN_POINT('Origin',(0.,1.2502668792019,7.0906158216879));
#44734=CARTESIAN_POINT('',(0.15,1.2502668792019,7.0906158216879));
#44735=CARTESIAN_POINT('',(0.,1.2502668792019,7.0906158216879));
#44736=CARTESIAN_POINT('',(0.15,1.2502668792019,7.0906158216879));
#44737=CARTESIAN_POINT('Origin',(0.,0.502246610957702,7.18246116187073));
#44738=CARTESIAN_POINT('',(0.15,0.502246610957702,7.18246116187073));
#44739=CARTESIAN_POINT('',(0.,0.502246610957702,7.18246116187073));
#44740=CARTESIAN_POINT('',(0.15,0.502246610957702,7.18246116187073));
#44741=CARTESIAN_POINT('Origin',(0.,-0.251276376258007,7.19561395453749));
#44742=CARTESIAN_POINT('',(0.15,-0.251276376258007,7.19561395453749));
#44743=CARTESIAN_POINT('',(0.,-0.251276376258007,7.19561395453749));
#44744=CARTESIAN_POINT('',(0.15,-0.251276376258007,7.19561395453749));
#44745=CARTESIAN_POINT('Origin',(0.,-1.00204632691247,7.12993009493931));
#44746=CARTESIAN_POINT('',(0.15,-1.00204632691247,7.12993009493931));
#44747=CARTESIAN_POINT('',(0.,-1.00204632691247,7.12993009493931));
#44748=CARTESIAN_POINT('',(0.15,-1.00204632691247,7.12993009493931));
#44749=CARTESIAN_POINT('Origin',(0.,-1.74183764831761,6.98612922918717));
#44750=CARTESIAN_POINT('',(0.15,-1.74183764831761,6.98612922918717));
#44751=CARTESIAN_POINT('',(0.,-1.74183764831761,6.98612922918717));
#44752=CARTESIAN_POINT('',(0.15,-1.74183764831761,6.98612922918717));
#44753=CARTESIAN_POINT('Origin',(0.,-2.56437209335648,10.2851346985256));
#44754=CARTESIAN_POINT('',(0.15,-2.56437209335648,10.2851346985256));
#44755=CARTESIAN_POINT('',(0.,-2.56437209335648,10.2851346985256));
#44756=CARTESIAN_POINT('',(0.15,-2.56437209335648,10.2851346985256));
#44757=CARTESIAN_POINT('Origin',(0.,-1.4752348701767,10.4968415286606));
#44758=CARTESIAN_POINT('',(0.15,-1.47523487017669,10.4968415286606));
#44759=CARTESIAN_POINT('',(0.,-1.4752348701767,10.4968415286606));
#44760=CARTESIAN_POINT('',(0.15,-1.4752348701767,10.4968415286606));
#44761=CARTESIAN_POINT('Origin',(0.,-0.36993466504651,10.5935427664024));
#44762=CARTESIAN_POINT('',(0.15,-0.36993466504651,10.5935427664024));
#44763=CARTESIAN_POINT('',(0.,-0.36993466504651,10.5935427664024));
#44764=CARTESIAN_POINT('',(0.15,-0.36993466504651,10.5935427664024));
#44765=CARTESIAN_POINT('Origin',(0.,0.739418621687727,10.5741789327541));
#44766=CARTESIAN_POINT('',(0.15,0.739418621687727,10.5741789327541));
#44767=CARTESIAN_POINT('',(0.,0.739418621687727,10.5741789327541));
#44768=CARTESIAN_POINT('',(0.15,0.739418621687727,10.5741789327541));
#44769=CARTESIAN_POINT('Origin',(0.,1.84067068326946,10.4389621819294));
#44770=CARTESIAN_POINT('',(0.15,1.84067068326946,10.4389621819294));
#44771=CARTESIAN_POINT('',(0.,1.84067068326946,10.4389621819294));
#44772=CARTESIAN_POINT('',(0.15,1.84067068326946,10.4389621819294));
#44773=CARTESIAN_POINT('Origin',(0.,2.92175597166019,10.1893739769462));
#44774=CARTESIAN_POINT('',(0.15,2.92175597166019,10.1893739769462));
#44775=CARTESIAN_POINT('',(0.,2.92175597166019,10.1893739769462));
#44776=CARTESIAN_POINT('',(0.15,2.92175597166019,10.1893739769462));
#44777=CARTESIAN_POINT('Origin',(0.,3.97082989020867,9.82814885840795));
#44778=CARTESIAN_POINT('',(0.15,3.97082989020867,9.82814885840795));
#44779=CARTESIAN_POINT('',(0.,3.97082989020867,9.82814885840795));
#44780=CARTESIAN_POINT('',(0.15,3.97082989020867,9.82814885840795));
#44781=CARTESIAN_POINT('Origin',(0.,2.69716747259457,6.67572375288087));
#44782=CARTESIAN_POINT('',(0.15,2.69716747259457,6.67572375288087));
#44783=CARTESIAN_POINT('Origin',(0.15,0.703228898426094,8.63463325964164));
#44784=CARTESIAN_POINT('Origin',(0.,-5.00154026730478,5.17924656243829));
#44785=CARTESIAN_POINT('',(0.15,-5.00154026730478,5.17924656243829));
#44786=CARTESIAN_POINT('',(0.,-5.00154026730478,5.17924656243829));
#44787=CARTESIAN_POINT('',(0.15,-4.43276262234474,5.6736774259684));
#44788=CARTESIAN_POINT('',(0.15,-5.00154026730478,5.17924656243829));
#44789=CARTESIAN_POINT('',(0.,-4.43276262234474,5.6736774259684));
#44790=CARTESIAN_POINT('Origin',(0.,-5.51551999045664,4.62807078974308));
#44791=CARTESIAN_POINT('',(0.15,-5.51551999045664,4.62807078974308));
#44792=CARTESIAN_POINT('',(0.,-5.51551999045664,4.62807078974308));
#44793=CARTESIAN_POINT('',(0.15,-5.51551999045664,4.62807078974308));
#44794=CARTESIAN_POINT('Origin',(0.,-5.9690705223963,4.02618890498938));
#44795=CARTESIAN_POINT('',(0.15,-5.9690705223963,4.02618890498938));
#44796=CARTESIAN_POINT('',(0.,-5.9690705223963,4.02618890498938));
#44797=CARTESIAN_POINT('',(0.15,-5.9690705223963,4.02618890498938));
#44798=CARTESIAN_POINT('Origin',(0.,-6.35722266858427,3.38019525205841));
#44799=CARTESIAN_POINT('',(0.15,-6.35722266858427,3.38019525205841));
#44800=CARTESIAN_POINT('',(0.,-6.35722266858427,3.38019525205841));
#44801=CARTESIAN_POINT('',(0.15,-6.35722266858427,3.38019525205841));
#44802=CARTESIAN_POINT('Origin',(0.,-6.67572375288087,2.69716747259457));
#44803=CARTESIAN_POINT('',(0.15,-6.67572375288087,2.69716747259457));
#44804=CARTESIAN_POINT('',(0.,-6.67572375288087,2.69716747259457));
#44805=CARTESIAN_POINT('',(0.15,-6.67572375288087,2.69716747259457));
#44806=CARTESIAN_POINT('Origin',(0.,-6.9210842107559,1.98458896188239));
#44807=CARTESIAN_POINT('',(0.15,-6.9210842107559,1.98458896188239));
#44808=CARTESIAN_POINT('',(0.,-6.9210842107559,1.98458896188239));
#44809=CARTESIAN_POINT('',(0.15,-6.9210842107559,1.98458896188239));
#44810=CARTESIAN_POINT('Origin',(0.,-10.1893739769462,2.92175597166019));
#44811=CARTESIAN_POINT('',(0.15,-10.1893739769462,2.92175597166019));
#44812=CARTESIAN_POINT('',(0.,-10.1893739769462,2.92175597166019));
#44813=CARTESIAN_POINT('',(0.15,-10.1893739769462,2.92175597166019));
#44814=CARTESIAN_POINT('Origin',(0.,-9.82814885840794,3.97082989020867));
#44815=CARTESIAN_POINT('',(0.15,-9.82814885840794,3.97082989020867));
#44816=CARTESIAN_POINT('',(0.,-9.82814885840794,3.97082989020867));
#44817=CARTESIAN_POINT('',(0.15,-9.82814885840794,3.97082989020867));
#44818=CARTESIAN_POINT('Origin',(0.,-9.35924448430463,4.97639856553044));
#44819=CARTESIAN_POINT('',(0.15,-9.35924448430463,4.97639856553044));
#44820=CARTESIAN_POINT('',(0.,-9.35924448430463,4.97639856553044));
#44821=CARTESIAN_POINT('',(0.15,-9.35924448430463,4.97639856553044));
#44822=CARTESIAN_POINT('Origin',(0.,-8.78779826908344,5.92744477678992));
#44823=CARTESIAN_POINT('',(0.15,-8.78779826908344,5.92744477678992));
#44824=CARTESIAN_POINT('',(0.,-8.78779826908344,5.92744477678992));
#44825=CARTESIAN_POINT('',(0.15,-8.78779826908344,5.92744477678992));
#44826=CARTESIAN_POINT('Origin',(0.,-8.12007109706117,6.81354866267732));
#44827=CARTESIAN_POINT('',(0.15,-8.12007109706117,6.81354866267732));
#44828=CARTESIAN_POINT('',(0.,-8.12007109706117,6.81354866267732));
#44829=CARTESIAN_POINT('',(0.15,-8.12007109706117,6.81354866267732));
#44830=CARTESIAN_POINT('Origin',(0.,-7.36337872686537,7.6250018835897));
#44831=CARTESIAN_POINT('',(0.15,-7.36337872686537,7.6250018835897));
#44832=CARTESIAN_POINT('',(0.,-7.36337872686537,7.6250018835897));
#44833=CARTESIAN_POINT('',(0.15,-7.36337872686537,7.6250018835897));
#44834=CARTESIAN_POINT('Origin',(0.,-6.52601163845198,8.35291398823125));
#44835=CARTESIAN_POINT('',(0.15,-6.52601163845198,8.35291398823125));
#44836=CARTESIAN_POINT('',(0.,-6.52601163845198,8.35291398823125));
#44837=CARTESIAN_POINT('',(0.15,-6.52601163845198,8.35291398823125));
#44838=CARTESIAN_POINT('Origin',(0.,-4.43276262234474,5.6736774259684));
#44839=CARTESIAN_POINT('',(0.15,-4.43276262234474,5.6736774259684));
#44840=CARTESIAN_POINT('Origin',(0.15,-7.31106829964546,5.16875147505682));
#44841=CARTESIAN_POINT('Origin',(0.,-6.98612922918717,-1.74183764831761));
#44842=CARTESIAN_POINT('',(0.15,-6.98612922918717,-1.74183764831761));
#44843=CARTESIAN_POINT('',(0.,-6.98612922918717,-1.74183764831761));
#44844=CARTESIAN_POINT('',(0.15,-7.12993009493931,-1.00204632691247));
#44845=CARTESIAN_POINT('',(0.15,-6.98612922918717,-1.74183764831761));
#44846=CARTESIAN_POINT('',(0.,-7.12993009493931,-1.00204632691247));
#44847=CARTESIAN_POINT('Origin',(0.,-6.76578686965854,-2.46254503194481));
#44848=CARTESIAN_POINT('',(0.15,-6.76578686965854,-2.46254503194481));
#44849=CARTESIAN_POINT('',(0.,-6.76578686965854,-2.46254503194481));
#44850=CARTESIAN_POINT('',(0.15,-6.76578686965854,-2.46254503194481));
#44851=CARTESIAN_POINT('Origin',(0.,-6.471317133354,-3.15627225688136));
#44852=CARTESIAN_POINT('',(0.15,-6.471317133354,-3.15627225688136));
#44853=CARTESIAN_POINT('',(0.,-6.471317133354,-3.15627225688136));
#44854=CARTESIAN_POINT('',(0.15,-6.471317133354,-3.15627225688136));
#44855=CARTESIAN_POINT('Origin',(0.,-6.10594629232627,-3.81541870247908));
#44856=CARTESIAN_POINT('',(0.15,-6.10594629232627,-3.81541870247908));
#44857=CARTESIAN_POINT('',(0.,-6.10594629232627,-3.81541870247908));
#44858=CARTESIAN_POINT('',(0.15,-6.10594629232627,-3.81541870247908));
#44859=CARTESIAN_POINT('Origin',(0.,-5.6736774259684,-4.43276262234474));
#44860=CARTESIAN_POINT('',(0.15,-5.6736774259684,-4.43276262234474));
#44861=CARTESIAN_POINT('',(0.,-5.6736774259684,-4.43276262234474));
#44862=CARTESIAN_POINT('',(0.15,-5.6736774259684,-4.43276262234474));
#44863=CARTESIAN_POINT('Origin',(0.,-5.17924656243829,-5.00154026730478));
#44864=CARTESIAN_POINT('',(0.15,-5.17924656243829,-5.00154026730478));
#44865=CARTESIAN_POINT('',(0.,-5.17924656243829,-5.00154026730478));
#44866=CARTESIAN_POINT('',(0.15,-5.17924656243829,-5.00154026730478));
#44867=CARTESIAN_POINT('Origin',(0.,-7.6250018835897,-7.36337872686537));
#44868=CARTESIAN_POINT('',(0.15,-7.6250018835897,-7.36337872686537));
#44869=CARTESIAN_POINT('',(0.,-7.6250018835897,-7.36337872686537));
#44870=CARTESIAN_POINT('',(0.15,-7.6250018835897,-7.36337872686537));
#44871=CARTESIAN_POINT('Origin',(0.,-8.35291398823125,-6.52601163845198));
#44872=CARTESIAN_POINT('',(0.15,-8.35291398823125,-6.52601163845198));
#44873=CARTESIAN_POINT('',(0.,-8.35291398823125,-6.52601163845198));
#44874=CARTESIAN_POINT('',(0.15,-8.35291398823125,-6.52601163845198));
#44875=CARTESIAN_POINT('Origin',(0.,-8.98930981925811,-5.61714420087197));
#44876=CARTESIAN_POINT('',(0.15,-8.98930981925811,-5.61714420087197));
#44877=CARTESIAN_POINT('',(0.,-8.98930981925811,-5.61714420087197));
#44878=CARTESIAN_POINT('',(0.15,-8.98930981925811,-5.61714420087197));
#44879=CARTESIAN_POINT('Origin',(0.,-9.52721689077117,-4.64673415596422));
#44880=CARTESIAN_POINT('',(0.15,-9.52721689077117,-4.64673415596422));
#44881=CARTESIAN_POINT('',(0.,-9.52721689077117,-4.64673415596422));
#44882=CARTESIAN_POINT('',(0.15,-9.52721689077117,-4.64673415596422));
#44883=CARTESIAN_POINT('Origin',(0.,-9.96074178033063,-3.62541351925209));
#44884=CARTESIAN_POINT('',(0.15,-9.96074178033063,-3.62541351925209));
#44885=CARTESIAN_POINT('',(0.,-9.96074178033063,-3.62541351925209));
#44886=CARTESIAN_POINT('',(0.15,-9.96074178033063,-3.62541351925209));
#44887=CARTESIAN_POINT('Origin',(0.,-10.2851346985256,-2.56437209335648));
#44888=CARTESIAN_POINT('',(0.15,-10.2851346985256,-2.56437209335648));
#44889=CARTESIAN_POINT('',(0.,-10.2851346985256,-2.56437209335648));
#44890=CARTESIAN_POINT('',(0.15,-10.2851346985256,-2.56437209335648));
#44891=CARTESIAN_POINT('Origin',(0.,-10.4968415286606,-1.47523487017669));
#44892=CARTESIAN_POINT('',(0.15,-10.4968415286606,-1.47523487017669));
#44893=CARTESIAN_POINT('',(0.,-10.4968415286606,-1.47523487017669));
#44894=CARTESIAN_POINT('',(0.15,-10.4968415286606,-1.47523487017669));
#44895=CARTESIAN_POINT('Origin',(0.,-7.12993009493931,-1.00204632691247));
#44896=CARTESIAN_POINT('',(0.15,-7.12993009493931,-1.00204632691247));
#44897=CARTESIAN_POINT('Origin',(0.15,-7.83804404554947,-4.18271252688892));
#44898=CARTESIAN_POINT('Origin',(0.,5.00154026730478,-5.17924656243829));
#44899=CARTESIAN_POINT('',(0.15,5.00154026730478,-5.17924656243829));
#44900=CARTESIAN_POINT('',(0.,5.00154026730478,-5.17924656243829));
#44901=CARTESIAN_POINT('',(0.15,4.43276262234474,-5.6736774259684));
#44902=CARTESIAN_POINT('',(0.15,5.00154026730478,-5.17924656243829));
#44903=CARTESIAN_POINT('',(0.,4.43276262234474,-5.6736774259684));
#44904=CARTESIAN_POINT('Origin',(0.,5.51551999045664,-4.62807078974308));
#44905=CARTESIAN_POINT('',(0.15,5.51551999045664,-4.62807078974308));
#44906=CARTESIAN_POINT('',(0.,5.51551999045664,-4.62807078974308));
#44907=CARTESIAN_POINT('',(0.15,5.51551999045664,-4.62807078974308));
#44908=CARTESIAN_POINT('Origin',(0.,5.9690705223963,-4.02618890498938));
#44909=CARTESIAN_POINT('',(0.15,5.9690705223963,-4.02618890498938));
#44910=CARTESIAN_POINT('',(0.,5.9690705223963,-4.02618890498938));
#44911=CARTESIAN_POINT('',(0.15,5.9690705223963,-4.02618890498938));
#44912=CARTESIAN_POINT('Origin',(0.,6.35722266858427,-3.38019525205841));
#44913=CARTESIAN_POINT('',(0.15,6.35722266858427,-3.38019525205841));
#44914=CARTESIAN_POINT('',(0.,6.35722266858427,-3.38019525205841));
#44915=CARTESIAN_POINT('',(0.15,6.35722266858427,-3.38019525205841));
#44916=CARTESIAN_POINT('Origin',(0.,6.67572375288087,-2.69716747259456));
#44917=CARTESIAN_POINT('',(0.15,6.67572375288087,-2.69716747259456));
#44918=CARTESIAN_POINT('',(0.,6.67572375288087,-2.69716747259456));
#44919=CARTESIAN_POINT('',(0.15,6.67572375288087,-2.69716747259456));
#44920=CARTESIAN_POINT('Origin',(0.,6.9210842107559,-1.98458896188239));
#44921=CARTESIAN_POINT('',(0.15,6.9210842107559,-1.98458896188239));
#44922=CARTESIAN_POINT('',(0.,6.9210842107559,-1.98458896188239));
#44923=CARTESIAN_POINT('',(0.15,6.9210842107559,-1.98458896188239));
#44924=CARTESIAN_POINT('Origin',(0.,10.1893739769462,-2.92175597166019));
#44925=CARTESIAN_POINT('',(0.15,10.1893739769462,-2.92175597166019));
#44926=CARTESIAN_POINT('',(0.,10.1893739769462,-2.92175597166019));
#44927=CARTESIAN_POINT('',(0.15,10.1893739769462,-2.92175597166019));
#44928=CARTESIAN_POINT('Origin',(0.,9.82814885840795,-3.97082989020866));
#44929=CARTESIAN_POINT('',(0.15,9.82814885840795,-3.97082989020866));
#44930=CARTESIAN_POINT('',(0.,9.82814885840795,-3.97082989020866));
#44931=CARTESIAN_POINT('',(0.15,9.82814885840795,-3.97082989020866));
#44932=CARTESIAN_POINT('Origin',(0.,9.35924448430463,-4.97639856553044));
#44933=CARTESIAN_POINT('',(0.15,9.35924448430463,-4.97639856553044));
#44934=CARTESIAN_POINT('',(0.,9.35924448430463,-4.97639856553044));
#44935=CARTESIAN_POINT('',(0.15,9.35924448430463,-4.97639856553044));
#44936=CARTESIAN_POINT('Origin',(0.,8.78779826908344,-5.92744477678991));
#44937=CARTESIAN_POINT('',(0.15,8.78779826908344,-5.92744477678991));
#44938=CARTESIAN_POINT('',(0.,8.78779826908344,-5.92744477678991));
#44939=CARTESIAN_POINT('',(0.15,8.78779826908344,-5.92744477678991));
#44940=CARTESIAN_POINT('Origin',(0.,8.12007109706117,-6.81354866267731));
#44941=CARTESIAN_POINT('',(0.15,8.12007109706117,-6.81354866267731));
#44942=CARTESIAN_POINT('',(0.,8.12007109706117,-6.81354866267731));
#44943=CARTESIAN_POINT('',(0.15,8.12007109706117,-6.81354866267731));
#44944=CARTESIAN_POINT('Origin',(0.,7.36337872686537,-7.6250018835897));
#44945=CARTESIAN_POINT('',(0.15,7.36337872686537,-7.6250018835897));
#44946=CARTESIAN_POINT('',(0.,7.36337872686537,-7.6250018835897));
#44947=CARTESIAN_POINT('',(0.15,7.36337872686537,-7.6250018835897));
#44948=CARTESIAN_POINT('Origin',(0.,6.52601163845198,-8.35291398823125));
#44949=CARTESIAN_POINT('',(0.15,6.52601163845198,-8.35291398823125));
#44950=CARTESIAN_POINT('',(0.,6.52601163845198,-8.35291398823125));
#44951=CARTESIAN_POINT('',(0.15,6.52601163845198,-8.35291398823125));
#44952=CARTESIAN_POINT('Origin',(0.,4.43276262234474,-5.6736774259684));
#44953=CARTESIAN_POINT('',(0.15,4.43276262234474,-5.6736774259684));
#44954=CARTESIAN_POINT('Origin',(0.15,7.31106829964546,-5.16875147505682));
#44955=CARTESIAN_POINT('Origin',(0.,0.,0.));
#44956=CARTESIAN_POINT('',(0.,-7.16418377501202E-16,5.85));
#44957=CARTESIAN_POINT('',(0.,-7.16418377501202E-16,5.85));
#44958=CARTESIAN_POINT('Origin',(0.,5.,16.2480768092719));
#44959=CARTESIAN_POINT('',(0.,0.,0.));
#44960=CARTESIAN_POINT('Origin',(4.1,-3.5,-6.06217782649107));
#44961=CARTESIAN_POINT('',(4.1,-3.5,-5.46217782649107));
#44962=CARTESIAN_POINT('Origin',(4.1,-3.5,-6.06217782649107));
#44963=CARTESIAN_POINT('',(5.7,-3.5,-5.46217782649107));
#44964=CARTESIAN_POINT('',(4.1,-3.5,-5.46217782649107));
#44965=CARTESIAN_POINT('Origin',(5.7,-3.5,-6.06217782649107));
#44966=CARTESIAN_POINT('Origin',(5.7,-3.5,-6.06217782649107));
#44967=CARTESIAN_POINT('Origin',(4.1,7.,0.));
#44968=CARTESIAN_POINT('',(4.1,7.,0.6));
#44969=CARTESIAN_POINT('Origin',(4.1,7.,0.));
#44970=CARTESIAN_POINT('',(5.7,7.,0.6));
#44971=CARTESIAN_POINT('',(4.1,7.,0.6));
#44972=CARTESIAN_POINT('Origin',(5.7,7.,0.));
#44973=CARTESIAN_POINT('Origin',(5.7,7.,0.));
#44974=CARTESIAN_POINT('Origin',(4.1,3.5,6.06217782649107));
#44975=CARTESIAN_POINT('',(4.1,3.5,6.66217782649107));
#44976=CARTESIAN_POINT('Origin',(4.1,3.5,6.06217782649107));
#44977=CARTESIAN_POINT('',(5.7,3.5,6.66217782649107));
#44978=CARTESIAN_POINT('',(4.1,3.5,6.66217782649107));
#44979=CARTESIAN_POINT('Origin',(5.7,3.5,6.06217782649107));
#44980=CARTESIAN_POINT('Origin',(5.7,3.5,6.06217782649107));
#44981=CARTESIAN_POINT('Origin',(4.1,-3.5,6.06217782649107));
#44982=CARTESIAN_POINT('',(4.1,-3.5,6.66217782649107));
#44983=CARTESIAN_POINT('Origin',(4.1,-3.5,6.06217782649107));
#44984=CARTESIAN_POINT('',(5.7,-3.5,6.66217782649107));
#44985=CARTESIAN_POINT('',(4.1,-3.5,6.66217782649107));
#44986=CARTESIAN_POINT('Origin',(5.7,-3.5,6.06217782649107));
#44987=CARTESIAN_POINT('Origin',(5.7,-3.5,6.06217782649107));
#44988=CARTESIAN_POINT('Origin',(4.1,-7.,8.57252759403147E-16));
#44989=CARTESIAN_POINT('',(4.1,-7.,0.600000000000001));
#44990=CARTESIAN_POINT('Origin',(4.1,-7.,8.57252759403147E-16));
#44991=CARTESIAN_POINT('',(5.7,-7.,0.600000000000001));
#44992=CARTESIAN_POINT('',(4.1,-7.,0.600000000000001));
#44993=CARTESIAN_POINT('Origin',(5.7,-7.,8.57252759403147E-16));
#44994=CARTESIAN_POINT('Origin',(5.7,-7.,8.32667268468867E-16));
#44995=CARTESIAN_POINT('Origin',(4.1,3.5,-6.06217782649107));
#44996=CARTESIAN_POINT('',(4.1,3.5,-5.46217782649107));
#44997=CARTESIAN_POINT('Origin',(4.1,3.5,-6.06217782649107));
#44998=CARTESIAN_POINT('',(5.7,3.5,-5.46217782649107));
#44999=CARTESIAN_POINT('',(4.1,3.5,-5.46217782649107));
#45000=CARTESIAN_POINT('Origin',(5.7,3.5,-6.06217782649107));
#45001=CARTESIAN_POINT('Origin',(5.7,3.5,-6.06217782649107));
#45002=CARTESIAN_POINT('Origin',(10.325,0.,0.));
#45003=CARTESIAN_POINT('',(9.5,-6.6,-8.08266887437253E-16));
#45004=CARTESIAN_POINT('Origin',(9.5,0.,0.));
#45005=CARTESIAN_POINT('',(11.15,-6.6,-8.08266887437253E-16));
#45006=CARTESIAN_POINT('',(10.325,-6.6,-8.08266887437253E-16));
#45007=CARTESIAN_POINT('Origin',(11.15,0.,0.));
#45008=CARTESIAN_POINT('Origin',(9.5,8.,0.));
#45009=CARTESIAN_POINT('',(9.5,-7.6,9.30731567351989E-16));
#45010=CARTESIAN_POINT('Origin',(9.5,0.,0.));
#45011=CARTESIAN_POINT('Origin',(11.15,6.6,0.));
#45012=CARTESIAN_POINT('',(11.15,-7.6,-9.30731567351989E-16));
#45013=CARTESIAN_POINT('Origin',(11.15,0.,0.));
#45014=CARTESIAN_POINT('Origin',(10.55,0.,0.));
#45015=CARTESIAN_POINT('',(15.2,-7.6,-9.30731567351989E-16));
#45016=CARTESIAN_POINT('Origin',(15.2,0.,0.));
#45017=CARTESIAN_POINT('',(10.55,-7.6,-9.30731567351989E-16));
#45018=CARTESIAN_POINT('Origin',(0.1,0.,0.));
#45019=CARTESIAN_POINT('',(0.2,-5.75,-7.04171909509728E-16));
#45020=CARTESIAN_POINT('Origin',(0.2,0.,0.));
#45021=CARTESIAN_POINT('',(-1.04083408558608E-16,-5.55,-6.79678973526781E-16));
#45022=CARTESIAN_POINT('',(0.1,-5.65,-6.91925441518255E-16));
#45023=CARTESIAN_POINT('Origin',(0.,0.,0.));
#45024=CARTESIAN_POINT('Origin',(2.15,0.,0.));
#45025=CARTESIAN_POINT('',(4.1,-5.75,-7.04171909509728E-16));
#45026=CARTESIAN_POINT('Origin',(4.1,0.,0.));
#45027=CARTESIAN_POINT('',(2.15,-5.75,-7.04171909509728E-16));
#45028=CARTESIAN_POINT('Origin',(4.1,8.3,0.));
#45029=CARTESIAN_POINT('',(4.1,-8.3,-1.0164568432923E-15));
#45030=CARTESIAN_POINT('Origin',(4.1,0.,0.));
#45031=CARTESIAN_POINT('Origin',(4.2,0.,0.));
#45032=CARTESIAN_POINT('',(4.3,-8.5,-1.04094977927525E-15));
#45033=CARTESIAN_POINT('Origin',(4.3,0.,0.));
#45034=CARTESIAN_POINT('',(4.2,-8.4,-1.02870331128378E-15));
#45035=CARTESIAN_POINT('Origin',(4.9,0.,0.));
#45036=CARTESIAN_POINT('',(5.5,-8.5,-1.04094977927525E-15));
#45037=CARTESIAN_POINT('Origin',(5.5,0.,0.));
#45038=CARTESIAN_POINT('',(4.9,-8.5,-1.04094977927525E-15));
#45039=CARTESIAN_POINT('Origin',(5.6,0.,0.));
#45040=CARTESIAN_POINT('',(5.7,-8.3,-1.0164568432923E-15));
#45041=CARTESIAN_POINT('Origin',(5.7,0.,0.));
#45042=CARTESIAN_POINT('',(5.6,-8.4,-1.02870331128378E-15));
#45043=CARTESIAN_POINT('Origin',(5.7,7.8,0.));
#45044=CARTESIAN_POINT('',(5.7,-7.8,-9.55224503334935E-16));
#45045=CARTESIAN_POINT('Origin',(5.7,0.,0.));
#45046=CARTESIAN_POINT('Origin',(5.8,0.,0.));
#45047=CARTESIAN_POINT('',(5.9,-7.6,-9.30731567351989E-16));
#45048=CARTESIAN_POINT('Origin',(5.9,0.,0.));
#45049=CARTESIAN_POINT('',(5.8,-7.7,-9.42978035343462E-16));
#45050=CARTESIAN_POINT('Origin',(10.55,0.,0.));
#45051=CARTESIAN_POINT('',(10.55,-7.6,-9.30731567351989E-16));
#45052=CARTESIAN_POINT('Origin',(15.35,0.,0.));
#45053=CARTESIAN_POINT('',(15.5,-7.3,-8.93992163377568E-16));
#45054=CARTESIAN_POINT('Origin',(15.5,0.,0.));
#45055=CARTESIAN_POINT('',(15.35,-7.45,-9.12361865364778E-16));
#45056=CARTESIAN_POINT('Origin',(15.5,3.81,0.));
#45057=CARTESIAN_POINT('',(15.5,-3.81,-4.66590430475142E-16));
#45058=CARTESIAN_POINT('Origin',(15.5,0.,0.));
#45059=CARTESIAN_POINT('Origin',(15.35,0.,0.));
#45060=CARTESIAN_POINT('',(15.2,-3.505,-4.29238703101147E-16));
#45061=CARTESIAN_POINT('',(15.35,-3.6575,-4.47914566788144E-16));
#45062=CARTESIAN_POINT('Origin',(15.2,0.,0.));
#45063=CARTESIAN_POINT('Origin',(7.75,0.,0.));
#45064=CARTESIAN_POINT('',(0.299999999999999,-3.505,-4.29238703101147E-16));
#45065=CARTESIAN_POINT('',(7.75,-3.505,-4.29238703101147E-16));
#45066=CARTESIAN_POINT('Origin',(0.3,0.,0.));
#45067=CARTESIAN_POINT('Origin',(0.15,0.,0.));
#45068=CARTESIAN_POINT('',(1.21430643318376E-16,-3.81,-4.66590430475142E-16));
#45069=CARTESIAN_POINT('',(0.15,-3.6575,-4.47914566788144E-16));
#45070=CARTESIAN_POINT('Origin',(0.,0.,0.));
#45071=CARTESIAN_POINT('Origin',(0.,5.55,0.));
#45072=CARTESIAN_POINT('',(0.,0.,0.));
#45073=CARTESIAN_POINT('Ctrl Pts',(1.5,7.84754716719688,0.196222987756156));
#45074=CARTESIAN_POINT('Ctrl Pts',(1.5,7.81119228460987,1.64757063353881));
#45075=CARTESIAN_POINT('Ctrl Pts',(1.5,6.91554447525315,4.51998492486374));
#45076=CARTESIAN_POINT('Ctrl Pts',(1.5,3.50267736434437,7.4868718005881));
#45077=CARTESIAN_POINT('Ctrl Pts',(1.5,0.388976709839364,7.98738647591309));
#45078=CARTESIAN_POINT('Ctrl Pts',(1.5,-3.03605598459972,7.49963380638162));
#45079=CARTESIAN_POINT('Ctrl Pts',(1.5,-6.61228876173712,5.42165566355736));
#45080=CARTESIAN_POINT('Ctrl Pts',(1.5,-8.54932617078778,-0.243176633643623));
#45081=CARTESIAN_POINT('Ctrl Pts',(1.5,-6.22283392853507,-5.96728243109739));
#45082=CARTESIAN_POINT('Ctrl Pts',(1.5,-1.04981238929058,-8.37823413619139));
#45083=CARTESIAN_POINT('Ctrl Pts',(1.5,3.83069172671807,-7.27968997349867));
#45084=CARTESIAN_POINT('Ctrl Pts',(1.5,6.98760878535643,-4.34429198533913));
#45085=CARTESIAN_POINT('Ctrl Pts',(1.5,7.81270707141321,-1.58709781495809));
#45086=CARTESIAN_POINT('Ctrl Pts',(1.5,7.8475471671968,-0.196222987759265));
#45087=CARTESIAN_POINT('Ctrl Pts',(1.45,7.8975314881998,0.197475047609996));
#45088=CARTESIAN_POINT('Ctrl Pts',(1.45,7.86096333275704,1.6580604328562));
#45089=CARTESIAN_POINT('Ctrl Pts',(1.45,6.9595908976357,4.54876633855873));
#45090=CARTESIAN_POINT('Ctrl Pts',(1.45,3.52498432623248,7.53457411142355));
#45091=CARTESIAN_POINT('Ctrl Pts',(1.45,0.391454182214871,8.03823003379014));
#45092=CARTESIAN_POINT('Ctrl Pts',(1.45,-3.05539276487285,7.54742851941855));
#45093=CARTESIAN_POINT('Ctrl Pts',(1.45,-6.65440676033426,5.45617725481441));
#45094=CARTESIAN_POINT('Ctrl Pts',(1.45,-8.60378192629141,-0.244722612287108));
#45095=CARTESIAN_POINT('Ctrl Pts',(1.45,-6.26246888682433,-6.00528658546585));
#45096=CARTESIAN_POINT('Ctrl Pts',(1.45,-1.05649900580092,-8.43160864942561));
#45097=CARTESIAN_POINT('Ctrl Pts',(1.45,3.85509473392834,-7.32602697005844));
#45098=CARTESIAN_POINT('Ctrl Pts',(1.45,7.03210632247969,-4.37199570838387));
#45099=CARTESIAN_POINT('Ctrl Pts',(1.45,7.86249342936929,-1.59716926962579));
#45100=CARTESIAN_POINT('Ctrl Pts',(1.45,7.89753148819974,-0.197475047612075));
#45101=CARTESIAN_POINT('Ctrl Pts',(1.4,7.94751580920271,0.198727107463835));
#45102=CARTESIAN_POINT('Ctrl Pts',(1.39999999999993,7.91068240791007,1.66845448860209));
#45103=CARTESIAN_POINT('Ctrl Pts',(1.40000000000002,7.00364385267458,4.57759399919538));
#45104=CARTESIAN_POINT('Ctrl Pts',(1.39999999999998,3.54730042414692,7.58220147330159));
#45105=CARTESIAN_POINT('Ctrl Pts',(1.40000000000001,0.393932018706067,8.08916896201712));
#45106=CARTESIAN_POINT('Ctrl Pts',(1.4,-3.07473297912541,7.59514305847378));
#45107=CARTESIAN_POINT('Ctrl Pts',(1.4,-6.69652021371548,5.49073393546304));
#45108=CARTESIAN_POINT('Ctrl Pts',(1.4,-8.65823334930758,-0.246279305382362));
#45109=CARTESIAN_POINT('Ctrl Pts',(1.4,-6.30210657736778,-6.04329867241492));
#45110=CARTESIAN_POINT('Ctrl Pts',(1.4,-1.06318590207245,-8.48495865972949));
#45111=CARTESIAN_POINT('Ctrl Pts',(1.4,3.87948701006332,-7.37243510096405));
#45112=CARTESIAN_POINT('Ctrl Pts',(1.4,7.07663300474131,-4.39961875654197));
#45113=CARTESIAN_POINT('Ctrl Pts',(1.4,7.91221070955278,-1.60724928656839));
#45114=CARTESIAN_POINT('Ctrl Pts',(1.4,7.94751580920268,-0.198727107464886));
#45115=CARTESIAN_POINT('Ctrl Pts',(1.35,7.99750013020562,0.199979167317675));
#45116=CARTESIAN_POINT('Ctrl Pts',(1.34999999999993,7.96045345605724,1.67894428791948));
#45117=CARTESIAN_POINT('Ctrl Pts',(1.35000000000002,7.04769027505713,4.60637541289036));
#45118=CARTESIAN_POINT('Ctrl Pts',(1.34999999999998,3.56960738603504,7.62990378413704));
#45119=CARTESIAN_POINT('Ctrl Pts',(1.35000000000001,0.396409491081574,8.14001251989417));
#45120=CARTESIAN_POINT('Ctrl Pts',(1.35,-3.09406975939854,7.6429377715107));
#45121=CARTESIAN_POINT('Ctrl Pts',(1.35,-6.73863821231263,5.52525552672008));
#45122=CARTESIAN_POINT('Ctrl Pts',(1.35,-8.71268910481122,-0.247825284025847));
#45123=CARTESIAN_POINT('Ctrl Pts',(1.35,-6.34174153565703,-6.08130282678338));
#45124=CARTESIAN_POINT('Ctrl Pts',(1.35,-1.06987251858278,-8.53833317296371));
#45125=CARTESIAN_POINT('Ctrl Pts',(1.35,3.9038900172736,-7.41877209752381));
#45126=CARTESIAN_POINT('Ctrl Pts',(1.35,7.12113054186457,-4.42732247958672));
#45127=CARTESIAN_POINT('Ctrl Pts',(1.35,7.96199706750886,-1.61732074123609));
#45128=CARTESIAN_POINT('Ctrl Pts',(1.35,7.99750013020562,-0.199979167317696));
#45129=CARTESIAN_POINT('',(1.35,7.99750013020562,-0.199979167317696));
#45130=CARTESIAN_POINT('',(1.5,7.84754700261759,-0.196229557926748));
#45131=CARTESIAN_POINT('Ctrl Pts',(1.35,7.99750013020562,-0.199979167317696));
#45132=CARTESIAN_POINT('Ctrl Pts',(1.4,7.94751580920268,-0.198727107464886));
#45133=CARTESIAN_POINT('Ctrl Pts',(1.45,7.89753148819974,-0.197475047612075));
#45134=CARTESIAN_POINT('Ctrl Pts',(1.5,7.8475471671968,-0.196222987759265));
#45135=CARTESIAN_POINT('',(1.5,7.8475470026176,0.196229557926727));
#45136=CARTESIAN_POINT('Ctrl Pts',(1.5,7.84754700261754,-0.196229557925989));
#45137=CARTESIAN_POINT('Ctrl Pts',(1.5,7.81270577222208,-1.58710215640402));
#45138=CARTESIAN_POINT('Ctrl Pts',(1.5,6.98760712840792,-4.3442935260205));
#45139=CARTESIAN_POINT('Ctrl Pts',(1.5,3.83069172671807,-7.27968997349867));
#45140=CARTESIAN_POINT('Ctrl Pts',(1.5,-1.04981238929058,-8.37823413619139));
#45141=CARTESIAN_POINT('Ctrl Pts',(1.5,-6.22283392853507,-5.96728243109739));
#45142=CARTESIAN_POINT('Ctrl Pts',(1.5,-8.54932617078778,-0.243176633643623));
#45143=CARTESIAN_POINT('Ctrl Pts',(1.5,-6.61228876173712,5.42165566355736));
#45144=CARTESIAN_POINT('Ctrl Pts',(1.5,-3.03605598459972,7.49963380638162));
#45145=CARTESIAN_POINT('Ctrl Pts',(1.5,0.388976709839364,7.98738647591309));
#45146=CARTESIAN_POINT('Ctrl Pts',(1.5,3.50267736434437,7.4868718005881));
#45147=CARTESIAN_POINT('Ctrl Pts',(1.5,6.91554104195091,4.51998790951536));
#45148=CARTESIAN_POINT('Ctrl Pts',(1.5,7.81118958157476,1.64757930237687));
#45149=CARTESIAN_POINT('Ctrl Pts',(1.5,7.84754683803257,0.196236128096295));
#45150=CARTESIAN_POINT('',(1.35,7.99750013020562,0.199979167317699));
#45151=CARTESIAN_POINT('Ctrl Pts',(1.5,7.84754700261752,0.196229557926939));
#45152=CARTESIAN_POINT('Ctrl Pts',(1.45,7.89753132265494,0.197481659599516));
#45153=CARTESIAN_POINT('Ctrl Pts',(1.4,7.94751564245708,0.198733760838668));
#45154=CARTESIAN_POINT('Ctrl Pts',(1.35,7.9974999624945,0.199985862511245));
#45155=CARTESIAN_POINT('Ctrl Pts',(1.35,7.99750013020562,0.199979167317675));
#45156=CARTESIAN_POINT('Ctrl Pts',(1.34999999999993,7.96045345605724,1.67894428791948));
#45157=CARTESIAN_POINT('Ctrl Pts',(1.35000000000002,7.04769027505713,4.60637541289036));
#45158=CARTESIAN_POINT('Ctrl Pts',(1.34999999999998,3.56960738603504,7.62990378413704));
#45159=CARTESIAN_POINT('Ctrl Pts',(1.35000000000001,0.396409491081574,8.14001251989417));
#45160=CARTESIAN_POINT('Ctrl Pts',(1.35,-3.09406975939854,7.6429377715107));
#45161=CARTESIAN_POINT('Ctrl Pts',(1.35,-6.73863821231263,5.52525552672008));
#45162=CARTESIAN_POINT('Ctrl Pts',(1.35,-8.71268910481122,-0.247825284025847));
#45163=CARTESIAN_POINT('Ctrl Pts',(1.35,-6.34174153565703,-6.08130282678338));
#45164=CARTESIAN_POINT('Ctrl Pts',(1.35,-1.06987251858278,-8.53833317296371));
#45165=CARTESIAN_POINT('Ctrl Pts',(1.35,3.9038900172736,-7.41877209752381));
#45166=CARTESIAN_POINT('Ctrl Pts',(1.35,7.12113054186457,-4.42732247958672));
#45167=CARTESIAN_POINT('Ctrl Pts',(1.35,7.96199706750886,-1.61732074123609));
#45168=CARTESIAN_POINT('Ctrl Pts',(1.35,7.99750013020562,-0.199979167317696));
#45169=CARTESIAN_POINT('Origin',(0.,7.99750013020562,-0.199979167317696));
#45170=CARTESIAN_POINT('',(0.15,7.99750004634874,-0.199982514912803));
#45171=CARTESIAN_POINT('',(0.,7.99750013020562,-0.199979167317696));
#45172=CARTESIAN_POINT('',(0.,7.84754700261759,-0.196229557926829));
#45173=CARTESIAN_POINT('Ctrl Pts',(0.,7.84754700261759,-0.196229557926836));
#45174=CARTESIAN_POINT('Ctrl Pts',(0.05,7.89753132257661,-0.197481659453884));
#45175=CARTESIAN_POINT('Ctrl Pts',(0.1,7.94751564253563,-0.198733760980932));
#45176=CARTESIAN_POINT('Ctrl Pts',(0.15,7.99749996249466,-0.19998586250798));
#45177=CARTESIAN_POINT('',(0.,7.04779698988764,-0.17623164120232));
#45178=CARTESIAN_POINT('',(0.,7.99750013020562,-0.199979167317696));
#45179=CARTESIAN_POINT('',(0.15,6.89784386230235,-0.172482031811513));
#45180=CARTESIAN_POINT('Ctrl Pts',(0.15,6.89784386230235,-0.172482031811513));
#45181=CARTESIAN_POINT('Ctrl Pts',(0.125000000000001,6.92283605023323,-0.173106966709981));
#45182=CARTESIAN_POINT('Ctrl Pts',(0.100000000000001,6.94782823816411,-0.173731901608448));
#45183=CARTESIAN_POINT('Ctrl Pts',(0.0500000000000009,6.99781261402587,
-0.174981771405384));
#45184=CARTESIAN_POINT('Ctrl Pts',(0.0250000000000005,7.02280480195676,
-0.175606706303851));
#45185=CARTESIAN_POINT('Ctrl Pts',(0.,7.04779698988764,-0.176231641202319));
#45186=CARTESIAN_POINT('',(1.35,6.89784386230235,-0.172482031811513));
#45187=CARTESIAN_POINT('',(0.,6.89784386230235,-0.172482031811513));
#45188=CARTESIAN_POINT('',(1.5,7.04779698988764,-0.176231641202319));
#45189=CARTESIAN_POINT('Ctrl Pts',(1.5,7.04779698988764,-0.17623164120232));
#45190=CARTESIAN_POINT('Ctrl Pts',(1.475,7.02280480195676,-0.175606706303852));
#45191=CARTESIAN_POINT('Ctrl Pts',(1.45,6.99781261402588,-0.174981771405384));
#45192=CARTESIAN_POINT('Ctrl Pts',(1.4,6.94782823816411,-0.173731901608449));
#45193=CARTESIAN_POINT('Ctrl Pts',(1.375,6.92283605023323,-0.173106966709981));
#45194=CARTESIAN_POINT('Ctrl Pts',(1.35,6.89784386230235,-0.172482031811513));
#45195=CARTESIAN_POINT('',(1.5,7.99750013020562,-0.199979167317696));
#45196=CARTESIAN_POINT('Ctrl Pts',(0.,7.99750013020562,0.199979167317699));
#45197=CARTESIAN_POINT('Ctrl Pts',(1.5,7.99750013020562,0.199979167317699));
#45198=CARTESIAN_POINT('Ctrl Pts',(0.,7.99680550506533,0.227709763328977));
#45199=CARTESIAN_POINT('Ctrl Pts',(1.5,7.99680550506533,0.227709763328977));
#45200=CARTESIAN_POINT('Ctrl Pts',(0.,7.99517719352766,0.283151319739461));
#45201=CARTESIAN_POINT('Ctrl Pts',(1.5,7.99517719352766,0.283151319739461));
#45202=CARTESIAN_POINT('Ctrl Pts',(0.,7.99201754244988,0.366254747518976));
#45203=CARTESIAN_POINT('Ctrl Pts',(1.5,7.99201754244988,0.366254747518976));
#45204=CARTESIAN_POINT('Ctrl Pts',(0.,7.98637028878955,0.476941502739911));
#45205=CARTESIAN_POINT('Ctrl Pts',(1.5,7.98637028878955,0.476941502739911));
#45206=CARTESIAN_POINT('Ctrl Pts',(0.,7.97692078469299,0.615101120651634));
#45207=CARTESIAN_POINT('Ctrl Pts',(1.5,7.97692078469299,0.615101120651634));
#45208=CARTESIAN_POINT('Ctrl Pts',(0.,7.96508164046245,0.75305452456902));
#45209=CARTESIAN_POINT('Ctrl Pts',(1.5,7.96508164046245,0.75305452456902));
#45210=CARTESIAN_POINT('Ctrl Pts',(0.,7.95085458504529,0.890786949553286));
#45211=CARTESIAN_POINT('Ctrl Pts',(1.5,7.95085458504529,0.890786949553286));
#45212=CARTESIAN_POINT('Ctrl Pts',(0.,7.93424262024774,1.02827379662482));
#45213=CARTESIAN_POINT('Ctrl Pts',(1.5,7.93424262024774,1.02827379662482));
#45214=CARTESIAN_POINT('Ctrl Pts',(0.,7.91525036159975,1.16547817540896));
#45215=CARTESIAN_POINT('Ctrl Pts',(1.5,7.91525036159975,1.16547817540896));
#45216=CARTESIAN_POINT('Ctrl Pts',(0.,7.89388377445281,1.302354563183));
#45217=CARTESIAN_POINT('Ctrl Pts',(1.5,7.89388377445281,1.302354563183));
#45218=CARTESIAN_POINT('Ctrl Pts',(0.,7.8701499101466,1.43885246359671));
#45219=CARTESIAN_POINT('Ctrl Pts',(1.5,7.8701499101466,1.43885246359671));
#45220=CARTESIAN_POINT('Ctrl Pts',(0.,7.84405664223428,1.57492006520944));
#45221=CARTESIAN_POINT('Ctrl Pts',(1.5,7.84405664223428,1.57492006520944));
#45222=CARTESIAN_POINT('Ctrl Pts',(0.,7.81561240275637,1.71050789997905));
#45223=CARTESIAN_POINT('Ctrl Pts',(1.5,7.81561240275637,1.71050789997905));
#45224=CARTESIAN_POINT('Ctrl Pts',(0.,7.78482591855295,1.84557250184531));
#45225=CARTESIAN_POINT('Ctrl Pts',(1.5,7.78482591855295,1.84557250184531));
#45226=CARTESIAN_POINT('Ctrl Pts',(0.,7.7517063259076,1.98007473729323));
#45227=CARTESIAN_POINT('Ctrl Pts',(1.5,7.7517063259076,1.98007473729323));
#45228=CARTESIAN_POINT('Ctrl Pts',(0.,7.71626328522376,2.11397813608642));
#45229=CARTESIAN_POINT('Ctrl Pts',(1.5,7.71626328522376,2.11397813608642));
#45230=CARTESIAN_POINT('Ctrl Pts',(0.,7.67850709573848,2.24724722210367));
#45231=CARTESIAN_POINT('Ctrl Pts',(1.5,7.67850709573848,2.24724722210367));
#45232=CARTESIAN_POINT('Ctrl Pts',(0.,7.63844881027727,2.37984584421849));
#45233=CARTESIAN_POINT('Ctrl Pts',(1.5,7.63844881027727,2.37984584421849));
#45234=CARTESIAN_POINT('Ctrl Pts',(0.,7.59610035005487,2.51173550715644));
#45235=CARTESIAN_POINT('Ctrl Pts',(1.5,7.59610035005487,2.51173550715644));
#45236=CARTESIAN_POINT('Ctrl Pts',(0.,7.55147444968317,2.64287611205357));
#45237=CARTESIAN_POINT('Ctrl Pts',(1.5,7.55147444968317,2.64287611205357));
#45238=CARTESIAN_POINT('Ctrl Pts',(0.,7.50458460222712,2.77322669695875));
#45239=CARTESIAN_POINT('Ctrl Pts',(1.5,7.50458460222712,2.77322669695875));
#45240=CARTESIAN_POINT('Ctrl Pts',(0.,7.4554450043059,2.90274617730927));
#45241=CARTESIAN_POINT('Ctrl Pts',(1.5,7.4554450043059,2.90274617730927));
#45242=CARTESIAN_POINT('Ctrl Pts',(0.,7.40407050123783,3.03139408640743));
#45243=CARTESIAN_POINT('Ctrl Pts',(1.5,7.40407050123783,3.03139408640743));
#45244=CARTESIAN_POINT('Ctrl Pts',(0.,7.3504765322259,3.15913131592731));
#45245=CARTESIAN_POINT('Ctrl Pts',(1.5,7.3504765322259,3.15913131592731));
#45246=CARTESIAN_POINT('Ctrl Pts',(0.,7.29467914718133,3.28591981327769));
#45247=CARTESIAN_POINT('Ctrl Pts',(1.5,7.29467914718133,3.28591981327769));
#45248=CARTESIAN_POINT('Ctrl Pts',(0.,7.23669502358639,3.41172227901232));
#45249=CARTESIAN_POINT('Ctrl Pts',(1.5,7.23669502358639,3.41172227901232));
#45250=CARTESIAN_POINT('Ctrl Pts',(0.,7.17654148339747,3.53650186427506));
#45251=CARTESIAN_POINT('Ctrl Pts',(1.5,7.17654148339747,3.53650186427506));
#45252=CARTESIAN_POINT('Ctrl Pts',(0.,7.11423650998858,3.66022186826995));
#45253=CARTESIAN_POINT('Ctrl Pts',(1.5,7.11423650998858,3.66022186826995));
#45254=CARTESIAN_POINT('Ctrl Pts',(0.,7.0497987651361,3.78284543574385));
#45255=CARTESIAN_POINT('Ctrl Pts',(1.5,7.0497987651361,3.78284543574385));
#45256=CARTESIAN_POINT('Ctrl Pts',(0.,6.98324757351643,3.90433570307324));
#45257=CARTESIAN_POINT('Ctrl Pts',(1.5,6.98324757351643,3.90433570307324));
#45258=CARTESIAN_POINT('Ctrl Pts',(0.,6.91460290724501,4.02465594435869));
#45259=CARTESIAN_POINT('Ctrl Pts',(1.5,6.91460290724501,4.02465594435869));
#45260=CARTESIAN_POINT('Ctrl Pts',(0.,6.84388537045522,4.14376971753289));
#45261=CARTESIAN_POINT('Ctrl Pts',(1.5,6.84388537045522,4.14376971753289));
#45262=CARTESIAN_POINT('Ctrl Pts',(0.,6.7711161839166,4.26164101048806));
#45263=CARTESIAN_POINT('Ctrl Pts',(1.5,6.7711161839166,4.26164101048806));
#45264=CARTESIAN_POINT('Ctrl Pts',(0.,6.69631716969182,4.3782343872287));
#45265=CARTESIAN_POINT('Ctrl Pts',(1.5,6.69631716969182,4.3782343872287));
#45266=CARTESIAN_POINT('Ctrl Pts',(0.,6.61951074822057,4.49351493997149));
#45267=CARTESIAN_POINT('Ctrl Pts',(1.5,6.61951074822057,4.49351493997149));
#45268=CARTESIAN_POINT('Ctrl Pts',(0.,6.54071993544069,4.60744824127455));
#45269=CARTESIAN_POINT('Ctrl Pts',(1.5,6.54071993544069,4.60744824127455));
#45270=CARTESIAN_POINT('Ctrl Pts',(0.,6.45996833994703,4.72000029619479));
#45271=CARTESIAN_POINT('Ctrl Pts',(1.5,6.45996833994703,4.72000029619479));
#45272=CARTESIAN_POINT('Ctrl Pts',(0.,6.37728016018709,4.83113749447132));
#45273=CARTESIAN_POINT('Ctrl Pts',(1.5,6.37728016018709,4.83113749447132));
#45274=CARTESIAN_POINT('Ctrl Pts',(0.,6.29268018169369,4.94082656273376));
#45275=CARTESIAN_POINT('Ctrl Pts',(1.5,6.29268018169369,4.94082656273376));
#45276=CARTESIAN_POINT('Ctrl Pts',(0.,6.20619376748869,5.04903459924095));
#45277=CARTESIAN_POINT('Ctrl Pts',(1.5,6.20619376748869,5.04903459924095));
#45278=CARTESIAN_POINT('Ctrl Pts',(0.,6.11784684852259,5.15572910864443));
#45279=CARTESIAN_POINT('Ctrl Pts',(1.5,6.11784684852259,5.15572910864443));
#45280=CARTESIAN_POINT('Ctrl Pts',(0.,6.02766591414962,5.26087803677814));
#45281=CARTESIAN_POINT('Ctrl Pts',(1.5,6.02766591414962,5.26087803677814));
#45282=CARTESIAN_POINT('Ctrl Pts',(0.,5.93567800263764,5.36444980547617));
#45283=CARTESIAN_POINT('Ctrl Pts',(1.5,5.93567800263764,5.36444980547617));
#45284=CARTESIAN_POINT('Ctrl Pts',(0.,5.84191069171256,5.46641334741981));
#45285=CARTESIAN_POINT('Ctrl Pts',(1.5,5.84191069171256,5.46641334741981));
#45286=CARTESIAN_POINT('Ctrl Pts',(0.,5.7463920906582,5.56673810430368));
#45287=CARTESIAN_POINT('Ctrl Pts',(1.5,5.7463920906582,5.56673810430368));
#45288=CARTESIAN_POINT('Ctrl Pts',(0.,5.64915083244991,5.66539402503307));
#45289=CARTESIAN_POINT('Ctrl Pts',(1.5,5.64915083244991,5.66539402503307));
#45290=CARTESIAN_POINT('Ctrl Pts',(0.,5.55021606592043,5.7623515639526));
#45291=CARTESIAN_POINT('Ctrl Pts',(1.5,5.55021606592043,5.7623515639526));
#45292=CARTESIAN_POINT('Ctrl Pts',(0.,5.4496174479585,5.85758167910642));
#45293=CARTESIAN_POINT('Ctrl Pts',(1.5,5.4496174479585,5.85758167910642));
#45294=CARTESIAN_POINT('Ctrl Pts',(0.,5.34738513573868,5.95105583052966));
#45295=CARTESIAN_POINT('Ctrl Pts',(1.5,5.34738513573868,5.95105583052966));
#45296=CARTESIAN_POINT('Ctrl Pts',(0.,5.24354977700161,6.04274599307213));
#45297=CARTESIAN_POINT('Ctrl Pts',(1.5,5.24354977700161,6.04274599307213));
#45298=CARTESIAN_POINT('Ctrl Pts',(0.,5.13814250036456,6.13262466925426));
#45299=CARTESIAN_POINT('Ctrl Pts',(1.5,5.13814250036456,6.13262466925426));
#45300=CARTESIAN_POINT('Ctrl Pts',(0.,5.03119490566216,6.22066490215623));
#45301=CARTESIAN_POINT('Ctrl Pts',(1.5,5.03119490566216,6.22066490215623));
#45302=CARTESIAN_POINT('Ctrl Pts',(0.,4.92273905431653,6.30684028834105));
#45303=CARTESIAN_POINT('Ctrl Pts',(1.5,4.92273905431653,6.30684028834105));
#45304=CARTESIAN_POINT('Ctrl Pts',(0.,4.81280745973631,6.39112499081213));
#45305=CARTESIAN_POINT('Ctrl Pts',(1.5,4.81280745973631,6.39112499081213));
#45306=CARTESIAN_POINT('Ctrl Pts',(0.,4.70143307738903,6.47349374434624));
#45307=CARTESIAN_POINT('Ctrl Pts',(1.5,4.70143307738903,6.47349374434624));
#45308=CARTESIAN_POINT('Ctrl Pts',(0.,4.58864929490092,6.55392186086201));
#45309=CARTESIAN_POINT('Ctrl Pts',(1.5,4.58864929490092,6.55392186086201));
#45310=CARTESIAN_POINT('Ctrl Pts',(0.,4.47448992218395,6.6323852348246));
#45311=CARTESIAN_POINT('Ctrl Pts',(1.5,4.47448992218395,6.6323852348246));
#45312=CARTESIAN_POINT('Ctrl Pts',(0.,4.35898918158915,6.70886034868665));
#45313=CARTESIAN_POINT('Ctrl Pts',(1.5,4.35898918158915,6.70886034868665));
#45314=CARTESIAN_POINT('Ctrl Pts',(0.,4.24218169808576,6.78332427836609));
#45315=CARTESIAN_POINT('Ctrl Pts',(1.5,4.24218169808576,6.78332427836609));
#45316=CARTESIAN_POINT('Ctrl Pts',(0.,4.12410248853737,6.85575470054339));
#45317=CARTESIAN_POINT('Ctrl Pts',(1.5,4.12410248853737,6.85575470054339));
#45318=CARTESIAN_POINT('Ctrl Pts',(0.,4.00478695100247,6.92612989999665));
#45319=CARTESIAN_POINT('Ctrl Pts',(1.5,4.00478695100247,6.92612989999665));
#45320=CARTESIAN_POINT('Ctrl Pts',(0.,3.8842708540588,6.99442877697431));
#45321=CARTESIAN_POINT('Ctrl Pts',(1.5,3.8842708540588,6.99442877697431));
#45322=CARTESIAN_POINT('Ctrl Pts',(0.,3.76259032615098,7.06063085460664));
#45323=CARTESIAN_POINT('Ctrl Pts',(1.5,3.76259032615098,7.06063085460664));
#45324=CARTESIAN_POINT('Ctrl Pts',(0.,3.6397818449606,7.12471628635595));
#45325=CARTESIAN_POINT('Ctrl Pts',(1.5,3.6397818449606,7.12471628635595));
#45326=CARTESIAN_POINT('Ctrl Pts',(0.,3.51588222625163,7.18666586113527));
#45327=CARTESIAN_POINT('Ctrl Pts',(1.5,3.51588222625163,7.18666586113527));
#45328=CARTESIAN_POINT('Ctrl Pts',(0.,3.39092861273723,7.24646100846688));
#45329=CARTESIAN_POINT('Ctrl Pts',(1.5,3.39092861273723,7.24646100846688));
#45330=CARTESIAN_POINT('Ctrl Pts',(0.,3.26495846296687,7.30408380368079));
#45331=CARTESIAN_POINT('Ctrl Pts',(1.5,3.26495846296687,7.30408380368079));
#45332=CARTESIAN_POINT('Ctrl Pts',(0.,3.13800954023332,7.35951697315365));
#45333=CARTESIAN_POINT('Ctrl Pts',(1.5,3.13800954023332,7.35951697315365));
#45334=CARTESIAN_POINT('Ctrl Pts',(0.,3.01011990149853,7.41274389958825));
#45335=CARTESIAN_POINT('Ctrl Pts',(1.5,3.01011990149853,7.41274389958825));
#45336=CARTESIAN_POINT('Ctrl Pts',(0.,2.88132788576944,7.46374862667568));
#45337=CARTESIAN_POINT('Ctrl Pts',(1.5,2.88132788576944,7.46374862667568));
#45338=CARTESIAN_POINT('Ctrl Pts',(0.,2.75167210249136,7.51251586379888));
#45339=CARTESIAN_POINT('Ctrl Pts',(1.5,2.75167210249136,7.51251586379888));
#45340=CARTESIAN_POINT('Ctrl Pts',(0.,2.62119141995823,7.55903099077765));
#45341=CARTESIAN_POINT('Ctrl Pts',(1.5,2.62119141995823,7.55903099077765));
#45342=CARTESIAN_POINT('Ctrl Pts',(0.,2.48992495373916,7.60328006265563));
#45343=CARTESIAN_POINT('Ctrl Pts',(1.5,2.48992495373916,7.60328006265563));
#45344=CARTESIAN_POINT('Ctrl Pts',(0.,2.35791205512022,7.64524981452938));
#45345=CARTESIAN_POINT('Ctrl Pts',(1.5,2.35791205512022,7.64524981452938));
#45346=CARTESIAN_POINT('Ctrl Pts',(0.,2.22519229915043,7.68492766496107));
#45347=CARTESIAN_POINT('Ctrl Pts',(1.5,2.22519229915043,7.68492766496107));
#45348=CARTESIAN_POINT('Ctrl Pts',(0.,2.09180547270157,7.72230171943385));
#45349=CARTESIAN_POINT('Ctrl Pts',(1.5,2.09180547270157,7.72230171943385));
#45350=CARTESIAN_POINT('Ctrl Pts',(0.,1.95779156254141,7.75736077385028));
#45351=CARTESIAN_POINT('Ctrl Pts',(1.5,1.95779156254141,7.75736077385028));
#45352=CARTESIAN_POINT('Ctrl Pts',(0.,1.82319074341923,7.79009431807383));
#45353=CARTESIAN_POINT('Ctrl Pts',(1.5,1.82319074341923,7.79009431807383));
#45354=CARTESIAN_POINT('Ctrl Pts',(0.,1.68804336616321,7.82049253951376));
#45355=CARTESIAN_POINT('Ctrl Pts',(1.5,1.68804336616321,7.82049253951376));
#45356=CARTESIAN_POINT('Ctrl Pts',(0.,1.55238994546332,7.84854632558908));
#45357=CARTESIAN_POINT('Ctrl Pts',(1.5,1.55238994546332,7.84854632558908));
#45358=CARTESIAN_POINT('Ctrl Pts',(0.,1.41627114766429,7.8742472662363));
#45359=CARTESIAN_POINT('Ctrl Pts',(1.5,1.41627114766429,7.8742472662363));
#45360=CARTESIAN_POINT('Ctrl Pts',(0.,1.27972777856816,7.89758765646114));
#45361=CARTESIAN_POINT('Ctrl Pts',(1.5,1.27972777856816,7.89758765646114));
#45362=CARTESIAN_POINT('Ctrl Pts',(0.,1.14280077124554,7.9185604989343));
#45363=CARTESIAN_POINT('Ctrl Pts',(1.5,1.14280077124554,7.9185604989343));
#45364=CARTESIAN_POINT('Ctrl Pts',(0.,1.00553117385475,7.93715950663143));
#45365=CARTESIAN_POINT('Ctrl Pts',(1.5,1.00553117385475,7.93715950663143));
#45366=CARTESIAN_POINT('Ctrl Pts',(0.,0.867960137262833,7.95337910418951));
#45367=CARTESIAN_POINT('Ctrl Pts',(1.5,0.867960137262833,7.95337910418951));
#45368=CARTESIAN_POINT('Ctrl Pts',(0.,0.730128902672967,7.96721442930753));
#45369=CARTESIAN_POINT('Ctrl Pts',(1.5,0.730128902672967,7.96721442930753));
#45370=CARTESIAN_POINT('Ctrl Pts',(0.,0.5920787892575,7.97866133419203));
#45371=CARTESIAN_POINT('Ctrl Pts',(1.5,0.5920787892575,7.97866133419203));
#45372=CARTESIAN_POINT('Ctrl Pts',(0.,0.453851181796014,7.987716387047));
#45373=CARTESIAN_POINT('Ctrl Pts',(1.5,0.453851181796014,7.987716387047));
#45374=CARTESIAN_POINT('Ctrl Pts',(0.,0.315487518317418,7.99437687360893));
#45375=CARTESIAN_POINT('Ctrl Pts',(1.5,0.315487518317418,7.99437687360893));
#45376=CARTESIAN_POINT('Ctrl Pts',(0.,0.177029277647647,7.99864079744603));
#45377=CARTESIAN_POINT('Ctrl Pts',(1.5,0.177029277647647,7.99864079744603));
#45378=CARTESIAN_POINT('Ctrl Pts',(0.,0.0385179669598796,8.00050688030184));
#45379=CARTESIAN_POINT('Ctrl Pts',(1.5,0.0385179669598796,8.00050688030184));
#45380=CARTESIAN_POINT('Ctrl Pts',(0.,-0.100004890673484,7.99997456248424));
#45381=CARTESIAN_POINT('Ctrl Pts',(1.5,-0.100004890673484,7.99997456248424));
#45382=CARTESIAN_POINT('Ctrl Pts',(0.,-0.238497768727719,7.99704400329904));
#45383=CARTESIAN_POINT('Ctrl Pts',(1.5,-0.238497768727719,7.99704400329904));
#45384=CARTESIAN_POINT('Ctrl Pts',(0.,-0.376919149672484,7.99171608152879));
#45385=CARTESIAN_POINT('Ctrl Pts',(1.5,-0.376919149672484,7.99171608152879));
#45386=CARTESIAN_POINT('Ctrl Pts',(0.,-0.51522753740225,7.98399239464616));
#45387=CARTESIAN_POINT('Ctrl Pts',(1.5,-0.51522753740225,7.98399239464616));
#45388=CARTESIAN_POINT('Ctrl Pts',(0.,-0.653381469668191,7.97387525807239));
#45389=CARTESIAN_POINT('Ctrl Pts',(1.5,-0.653381469668191,7.97387525807239));
#45390=CARTESIAN_POINT('Ctrl Pts',(0.,-0.79133953051216,7.96136770448041));
#45391=CARTESIAN_POINT('Ctrl Pts',(1.5,-0.79133953051216,7.96136770448041));
#45392=CARTESIAN_POINT('Ctrl Pts',(0.,-0.929060362703415,7.9464734831431));
#45393=CARTESIAN_POINT('Ctrl Pts',(1.5,-0.929060362703415,7.9464734831431));
#45394=CARTESIAN_POINT('Ctrl Pts',(0.,-1.06650268017919,7.92919705932597));
#45395=CARTESIAN_POINT('Ctrl Pts',(1.5,-1.06650268017919,7.92919705932597));
#45396=CARTESIAN_POINT('Ctrl Pts',(0.,-1.20362528036102,7.90954361243223));
#45397=CARTESIAN_POINT('Ctrl Pts',(1.5,-1.20362528036102,7.90954361243223));
#45398=CARTESIAN_POINT('Ctrl Pts',(0.,-1.34038705647638,7.88751903419278));
#45399=CARTESIAN_POINT('Ctrl Pts',(1.5,-1.34038705647638,7.88751903419278));
#45400=CARTESIAN_POINT('Ctrl Pts',(0.,-1.47674700988613,7.86312992690012));
#45401=CARTESIAN_POINT('Ctrl Pts',(1.5,-1.47674700988613,7.86312992690012));
#45402=CARTESIAN_POINT('Ctrl Pts',(0.,-1.61266426241897,7.83638360168696));
#45403=CARTESIAN_POINT('Ctrl Pts',(1.5,-1.61266426241897,7.83638360168696));
#45404=CARTESIAN_POINT('Ctrl Pts',(0.,-1.74809806871318,7.80728807684891));
#45405=CARTESIAN_POINT('Ctrl Pts',(1.5,-1.74809806871318,7.80728807684891));
#45406=CARTESIAN_POINT('Ctrl Pts',(0.,-1.88300782832634,7.77585207492992));
#45407=CARTESIAN_POINT('Ctrl Pts',(1.5,-1.88300782832634,7.77585207492992));
#45408=CARTESIAN_POINT('Ctrl Pts',(0.,-2.01735309785401,7.74208501985214));
#45409=CARTESIAN_POINT('Ctrl Pts',(1.5,-2.01735309785401,7.74208501985214));
#45410=CARTESIAN_POINT('Ctrl Pts',(0.,-2.15109360305827,7.70599703408921));
#45411=CARTESIAN_POINT('Ctrl Pts',(1.5,-2.15109360305827,7.70599703408921));
#45412=CARTESIAN_POINT('Ctrl Pts',(0.,-2.28418925100688,7.66759893588344));
#45413=CARTESIAN_POINT('Ctrl Pts',(1.5,-2.28418925100688,7.66759893588344));
#45414=CARTESIAN_POINT('Ctrl Pts',(0.,-2.41660014222365,7.62690223650643));
#45415=CARTESIAN_POINT('Ctrl Pts',(1.5,-2.41660014222365,7.62690223650643));
#45416=CARTESIAN_POINT('Ctrl Pts',(0.,-2.54828658250082,7.58391913630904));
#45417=CARTESIAN_POINT('Ctrl Pts',(1.5,-2.54828658250082,7.58391913630904));
#45418=CARTESIAN_POINT('Ctrl Pts',(0.,-2.67920909472433,7.53866252081464));
#45419=CARTESIAN_POINT('Ctrl Pts',(1.5,-2.67920909472433,7.53866252081464));
#45420=CARTESIAN_POINT('Ctrl Pts',(0.,-2.80932843071254,7.49114595685495));
#45421=CARTESIAN_POINT('Ctrl Pts',(1.5,-2.80932843071254,7.49114595685495));
#45422=CARTESIAN_POINT('Ctrl Pts',(0.,-2.9386055830693,7.44138368874851));
#45423=CARTESIAN_POINT('Ctrl Pts',(1.5,-2.9386055830693,7.44138368874851));
#45424=CARTESIAN_POINT('Ctrl Pts',(0.,-3.06700179705218,7.38939063452162));
#45425=CARTESIAN_POINT('Ctrl Pts',(1.5,-3.06700179705218,7.38939063452162));
#45426=CARTESIAN_POINT('Ctrl Pts',(0.,-3.19447858199903,7.33518238095163));
#45427=CARTESIAN_POINT('Ctrl Pts',(1.5,-3.19447858199903,7.33518238095163));
#45428=CARTESIAN_POINT('Ctrl Pts',(0.,-3.32099772277123,7.27877517865203));
#45429=CARTESIAN_POINT('Ctrl Pts',(1.5,-3.32099772277123,7.27877517865203));
#45430=CARTESIAN_POINT('Ctrl Pts',(0.,-3.44652129121381,7.22018593719872));
#45431=CARTESIAN_POINT('Ctrl Pts',(1.5,-3.44652129121381,7.22018593719872));
#45432=CARTESIAN_POINT('Ctrl Pts',(0.,-3.57101165763383,7.15943222029806));
#45433=CARTESIAN_POINT('Ctrl Pts',(1.5,-3.57101165763383,7.15943222029806));
#45434=CARTESIAN_POINT('Ctrl Pts',(0.,-3.6944315022971,7.09653224099529));
#45435=CARTESIAN_POINT('Ctrl Pts',(1.5,-3.6944315022971,7.09653224099529));
#45436=CARTESIAN_POINT('Ctrl Pts',(0.,-3.8167438263836,7.03150485574848));
#45437=CARTESIAN_POINT('Ctrl Pts',(1.5,-3.8167438263836,7.03150485574848));
#45438=CARTESIAN_POINT('Ctrl Pts',(0.,-3.93791196296269,6.96436955854269));
#45439=CARTESIAN_POINT('Ctrl Pts',(1.5,-3.93791196296269,6.96436955854269));
#45440=CARTESIAN_POINT('Ctrl Pts',(0.,-4.05789958798918,6.89514647504389));
#45441=CARTESIAN_POINT('Ctrl Pts',(1.5,-4.05789958798918,6.89514647504389));
#45442=CARTESIAN_POINT('Ctrl Pts',(0.,-4.17667073132075,6.82385635679251));
#45443=CARTESIAN_POINT('Ctrl Pts',(1.5,-4.17667073132075,6.82385635679251));
#45444=CARTESIAN_POINT('Ctrl Pts',(0.,-4.29418978775755,6.75052057543597));
#45445=CARTESIAN_POINT('Ctrl Pts',(1.5,-4.29418978775755,6.75052057543597));
#45446=CARTESIAN_POINT('Ctrl Pts',(0.,-4.41042152744403,6.67516111587753));
#45447=CARTESIAN_POINT('Ctrl Pts',(1.5,-4.41042152744403,6.67516111587753));
#45448=CARTESIAN_POINT('Ctrl Pts',(0.,-4.52533110629424,6.59780056946357));
#45449=CARTESIAN_POINT('Ctrl Pts',(1.5,-4.52533110629424,6.59780056946357));
#45450=CARTESIAN_POINT('Ctrl Pts',(0.,-4.63888407644116,6.51846212720865));
#45451=CARTESIAN_POINT('Ctrl Pts',(1.5,-4.63888407644116,6.51846212720865));
#45452=CARTESIAN_POINT('Ctrl Pts',(0.,-4.75104639671082,6.43716957305794));
#45453=CARTESIAN_POINT('Ctrl Pts',(1.5,-4.75104639671082,6.43716957305794));
#45454=CARTESIAN_POINT('Ctrl Pts',(0.,-4.86178444312194,6.35394727718697));
#45455=CARTESIAN_POINT('Ctrl Pts',(1.5,-4.86178444312194,6.35394727718697));
#45456=CARTESIAN_POINT('Ctrl Pts',(0.,-4.97106501865637,6.26882018827667));
#45457=CARTESIAN_POINT('Ctrl Pts',(1.5,-4.97106501865637,6.26882018827667));
#45458=CARTESIAN_POINT('Ctrl Pts',(0.,-5.07885536305621,6.18181382582466));
#45459=CARTESIAN_POINT('Ctrl Pts',(1.5,-5.07885536305621,6.18181382582466));
#45460=CARTESIAN_POINT('Ctrl Pts',(0.,-5.18512316264831,6.09295427249219));
#45461=CARTESIAN_POINT('Ctrl Pts',(1.5,-5.18512316264831,6.09295427249219));
#45462=CARTESIAN_POINT('Ctrl Pts',(0.,-5.2898365601966,6.00226816648635));
#45463=CARTESIAN_POINT('Ctrl Pts',(1.5,-5.2898365601966,6.00226816648635));
#45464=CARTESIAN_POINT('Ctrl Pts',(0.,-5.392964164783,5.90978269397704));
#45465=CARTESIAN_POINT('Ctrl Pts',(1.5,-5.392964164783,5.90978269397704));
#45466=CARTESIAN_POINT('Ctrl Pts',(0.,-5.49447506087342,5.81552558055624));
#45467=CARTESIAN_POINT('Ctrl Pts',(1.5,-5.49447506087342,5.81552558055624));
#45468=CARTESIAN_POINT('Ctrl Pts',(0.,-5.59433881741343,5.71952508273097));
#45469=CARTESIAN_POINT('Ctrl Pts',(1.5,-5.59433881741343,5.71952508273097));
#45470=CARTESIAN_POINT('Ctrl Pts',(0.,-5.69252549695431,5.62180997944946));
#45471=CARTESIAN_POINT('Ctrl Pts',(1.5,-5.69252549695431,5.62180997944946));
#45472=CARTESIAN_POINT('Ctrl Pts',(0.,-5.78900566480983,5.52240956365993));
#45473=CARTESIAN_POINT('Ctrl Pts',(1.5,-5.78900566480983,5.52240956365993));
#45474=CARTESIAN_POINT('Ctrl Pts',(0.,-5.88375039824441,5.42135363390141));
#45475=CARTESIAN_POINT('Ctrl Pts',(1.5,-5.88375039824441,5.42135363390141));
#45476=CARTESIAN_POINT('Ctrl Pts',(0.,-5.97673129476659,5.31867248501124));
#45477=CARTESIAN_POINT('Ctrl Pts',(1.5,-5.97673129476659,5.31867248501124));
#45478=CARTESIAN_POINT('Ctrl Pts',(0.,-6.06792048045517,5.21439689886345));
#45479=CARTESIAN_POINT('Ctrl Pts',(1.5,-6.06792048045517,5.21439689886345));
#45480=CARTESIAN_POINT('Ctrl Pts',(0.,-6.15729061831829,5.10855813513777));
#45481=CARTESIAN_POINT('Ctrl Pts',(1.5,-6.15729061831829,5.10855813513777));
#45482=CARTESIAN_POINT('Ctrl Pts',(0.,-6.24481491668612,5.00118792211818));
#45483=CARTESIAN_POINT('Ctrl Pts',(1.5,-6.24481491668612,5.00118792211818));
#45484=CARTESIAN_POINT('Ctrl Pts',(0.,-6.33046713763756,4.89231844752085));
#45485=CARTESIAN_POINT('Ctrl Pts',(1.5,-6.33046713763756,4.89231844752085));
#45486=CARTESIAN_POINT('Ctrl Pts',(0.,-6.4142216044593,4.78198234851926));
#45487=CARTESIAN_POINT('Ctrl Pts',(1.5,-6.4142216044593,4.78198234851926));
#45488=CARTESIAN_POINT('Ctrl Pts',(0.,-6.49605320913994,4.67021270179733));
#45489=CARTESIAN_POINT('Ctrl Pts',(1.5,-6.49605320913994,4.67021270179733));
#45490=CARTESIAN_POINT('Ctrl Pts',(0.,-6.57593741989968,4.55704301363019));
#45491=CARTESIAN_POINT('Ctrl Pts',(1.5,-6.57593741989968,4.55704301363019));
#45492=CARTESIAN_POINT('Ctrl Pts',(0.,-6.65385028875591,4.44250720999153));
#45493=CARTESIAN_POINT('Ctrl Pts',(1.5,-6.65385028875591,4.44250720999153));
#45494=CARTESIAN_POINT('Ctrl Pts',(0.,-6.7297684591252,4.3266396266874));
#45495=CARTESIAN_POINT('Ctrl Pts',(1.5,-6.7297684591252,4.3266396266874));
#45496=CARTESIAN_POINT('Ctrl Pts',(0.,-6.80366917239198,4.20947499877372));
#45497=CARTESIAN_POINT('Ctrl Pts',(1.5,-6.80366917239198,4.20947499877372));
#45498=CARTESIAN_POINT('Ctrl Pts',(0.,-6.87553027451456,4.0910484499988));
#45499=CARTESIAN_POINT('Ctrl Pts',(1.5,-6.87553027451456,4.0910484499988));
#45500=CARTESIAN_POINT('Ctrl Pts',(0.,-6.94533022266887,3.97139548227007));
#45501=CARTESIAN_POINT('Ctrl Pts',(1.5,-6.94533022266887,3.97139548227007));
#45502=CARTESIAN_POINT('Ctrl Pts',(0.,-7.01304809193043,3.85055196514442));
#45503=CARTESIAN_POINT('Ctrl Pts',(1.5,-7.01304809193043,3.85055196514442));
#45504=CARTESIAN_POINT('Ctrl Pts',(0.,-7.07866358199495,3.72855412534148));
#45505=CARTESIAN_POINT('Ctrl Pts',(1.5,-7.07866358199495,3.72855412534148));
#45506=CARTESIAN_POINT('Ctrl Pts',(0.,-7.14215702280734,3.6054385356329));
#45507=CARTESIAN_POINT('Ctrl Pts',(1.5,-7.14215702280734,3.6054385356329));
#45508=CARTESIAN_POINT('Ctrl Pts',(0.,-7.2035093802301,3.48124210375322));
#45509=CARTESIAN_POINT('Ctrl Pts',(1.5,-7.2035093802301,3.48124210375322));
#45510=CARTESIAN_POINT('Ctrl Pts',(0.,-7.26270226175155,3.35600206133158));
#45511=CARTESIAN_POINT('Ctrl Pts',(1.5,-7.26270226175155,3.35600206133158));
#45512=CARTESIAN_POINT('Ctrl Pts',(0.,-7.31971792223396,3.22975595284375));
#45513=CARTESIAN_POINT('Ctrl Pts',(1.5,-7.31971792223396,3.22975595284375));
#45514=CARTESIAN_POINT('Ctrl Pts',(0.,-7.37453926970234,3.10254162458354));
#45515=CARTESIAN_POINT('Ctrl Pts',(1.5,-7.37453926970234,3.10254162458354));
#45516=CARTESIAN_POINT('Ctrl Pts',(0.,-7.42714986999163,2.97439721310696));
#45517=CARTESIAN_POINT('Ctrl Pts',(1.5,-7.42714986999163,2.97439721310696));
#45518=CARTESIAN_POINT('Ctrl Pts',(0.,-7.47753395143493,2.84536113369459));
#45519=CARTESIAN_POINT('Ctrl Pts',(1.5,-7.47753395143493,2.84536113369459));
#45520=CARTESIAN_POINT('Ctrl Pts',(0.,-7.52567640959341,2.7154720688311));
#45521=CARTESIAN_POINT('Ctrl Pts',(1.5,-7.52567640959341,2.7154720688311));
#45522=CARTESIAN_POINT('Ctrl Pts',(0.,-7.57156281202762,2.58476895670172));
#45523=CARTESIAN_POINT('Ctrl Pts',(1.5,-7.57156281202762,2.58476895670172));
#45524=CARTESIAN_POINT('Ctrl Pts',(0.,-7.61517940311102,2.45329097970451));
#45525=CARTESIAN_POINT('Ctrl Pts',(1.5,-7.61517940311102,2.45329097970451));
#45526=CARTESIAN_POINT('Ctrl Pts',(0.,-7.65651310766076,2.32107755253587));
#45527=CARTESIAN_POINT('Ctrl Pts',(1.5,-7.65651310766076,2.32107755253587));
#45528=CARTESIAN_POINT('Ctrl Pts',(0.,-7.69555153461076,2.18816831029056));
#45529=CARTESIAN_POINT('Ctrl Pts',(1.5,-7.69555153461076,2.18816831029056));
#45530=CARTESIAN_POINT('Ctrl Pts',(0.,-7.7322829807279,2.05460309657569));
#45531=CARTESIAN_POINT('Ctrl Pts',(1.5,-7.7322829807279,2.05460309657569));
#45532=CARTESIAN_POINT('Ctrl Pts',(0.,-7.76669643437085,1.92042195163751));
#45533=CARTESIAN_POINT('Ctrl Pts',(1.5,-7.76669643437085,1.92042195163751));
#45534=CARTESIAN_POINT('Ctrl Pts',(0.,-7.79878157929215,1.78566510050061));
#45535=CARTESIAN_POINT('Ctrl Pts',(1.5,-7.79878157929215,1.78566510050061));
#45536=CARTESIAN_POINT('Ctrl Pts',(0.,-7.82852879722494,1.65037294078415));
#45537=CARTESIAN_POINT('Ctrl Pts',(1.5,-7.82852879722494,1.65037294078415));
#45538=CARTESIAN_POINT('Ctrl Pts',(0.,-7.85592917051368,1.51458603052897));
#45539=CARTESIAN_POINT('Ctrl Pts',(1.5,-7.85592917051368,1.51458603052897));
#45540=CARTESIAN_POINT('Ctrl Pts',(0.,-7.88097448478828,1.37834507603462));
#45541=CARTESIAN_POINT('Ctrl Pts',(1.5,-7.88097448478828,1.37834507603462));
#45542=CARTESIAN_POINT('Ctrl Pts',(0.,-7.90365723168263,1.24169091970572));
#45543=CARTESIAN_POINT('Ctrl Pts',(1.5,-7.90365723168263,1.24169091970572));
#45544=CARTESIAN_POINT('Ctrl Pts',(0.,-7.92397061159682,1.10466452790671));
#45545=CARTESIAN_POINT('Ctrl Pts',(1.5,-7.92397061159682,1.10466452790671));
#45546=CARTESIAN_POINT('Ctrl Pts',(0.,-7.94190853522107,0.967306978600068));
#45547=CARTESIAN_POINT('Ctrl Pts',(1.5,-7.94190853522107,0.967306978600068));
#45548=CARTESIAN_POINT('Ctrl Pts',(0.,-7.95746562510374,0.829659448991489));
#45549=CARTESIAN_POINT('Ctrl Pts',(1.5,-7.95746562510374,0.829659448991489));
#45550=CARTESIAN_POINT('Ctrl Pts',(0.,-7.97063721726419,0.691763203181292));
#45551=CARTESIAN_POINT('Ctrl Pts',(1.5,-7.97063721726419,0.691763203181292));
#45552=CARTESIAN_POINT('Ctrl Pts',(0.,-7.98141936284981,0.553659579821253));
#45553=CARTESIAN_POINT('Ctrl Pts',(1.5,-7.98141936284981,0.553659579821253));
#45554=CARTESIAN_POINT('Ctrl Pts',(0.,-7.98980882983796,0.41538997977611));
#45555=CARTESIAN_POINT('Ctrl Pts',(1.5,-7.98980882983796,0.41538997977611));
#45556=CARTESIAN_POINT('Ctrl Pts',(0.,-7.9958031034851,0.276995853676294));
#45557=CARTESIAN_POINT('Ctrl Pts',(1.5,-7.9958031034851,0.276995853676294));
#45558=CARTESIAN_POINT('Ctrl Pts',(0.,-7.99940038682089,0.138518689473731));
#45559=CARTESIAN_POINT('Ctrl Pts',(1.5,-7.99940038682089,0.138518689473731));
#45560=CARTESIAN_POINT('Ctrl Pts',(0.,-8.00059960118697,7.404667157207E-14));
#45561=CARTESIAN_POINT('Ctrl Pts',(1.5,-8.00059960118697,7.404667157207E-14));
#45562=CARTESIAN_POINT('Ctrl Pts',(0.,-7.99940038682102,-0.138518689473581));
#45563=CARTESIAN_POINT('Ctrl Pts',(1.5,-7.99940038682102,-0.138518689473581));
#45564=CARTESIAN_POINT('Ctrl Pts',(0.,-7.99580310348534,-0.276995853676148));
#45565=CARTESIAN_POINT('Ctrl Pts',(1.5,-7.99580310348534,-0.276995853676148));
#45566=CARTESIAN_POINT('Ctrl Pts',(0.,-7.98980882983822,-0.415389979775981));
#45567=CARTESIAN_POINT('Ctrl Pts',(1.5,-7.98980882983822,-0.415389979775981));
#45568=CARTESIAN_POINT('Ctrl Pts',(0.,-7.98141936285002,-0.55365957982111));
#45569=CARTESIAN_POINT('Ctrl Pts',(1.5,-7.98141936285002,-0.55365957982111));
#45570=CARTESIAN_POINT('Ctrl Pts',(0.,-7.97063721726421,-0.691763203181143));
#45571=CARTESIAN_POINT('Ctrl Pts',(1.5,-7.97063721726421,-0.691763203181143));
#45572=CARTESIAN_POINT('Ctrl Pts',(0.,-7.95746562510355,-0.829659448991339));
#45573=CARTESIAN_POINT('Ctrl Pts',(1.5,-7.95746562510355,-0.829659448991339));
#45574=CARTESIAN_POINT('Ctrl Pts',(0.,-7.94190853522072,-0.96730697859992));
#45575=CARTESIAN_POINT('Ctrl Pts',(1.5,-7.94190853522072,-0.96730697859992));
#45576=CARTESIAN_POINT('Ctrl Pts',(0.,-7.92397061159648,-1.10466452790657));
#45577=CARTESIAN_POINT('Ctrl Pts',(1.5,-7.92397061159648,-1.10466452790657));
#45578=CARTESIAN_POINT('Ctrl Pts',(0.,-7.90365723168241,-1.24169091970559));
#45579=CARTESIAN_POINT('Ctrl Pts',(1.5,-7.90365723168241,-1.24169091970559));
#45580=CARTESIAN_POINT('Ctrl Pts',(0.,-7.88097448478831,-1.37834507603449));
#45581=CARTESIAN_POINT('Ctrl Pts',(1.5,-7.88097448478831,-1.37834507603449));
#45582=CARTESIAN_POINT('Ctrl Pts',(0.,-7.85592917051396,-1.5145860305288));
#45583=CARTESIAN_POINT('Ctrl Pts',(1.5,-7.85592917051396,-1.5145860305288));
#45584=CARTESIAN_POINT('Ctrl Pts',(0.,-7.82852879722539,-1.65037294078395));
#45585=CARTESIAN_POINT('Ctrl Pts',(1.5,-7.82852879722539,-1.65037294078395));
#45586=CARTESIAN_POINT('Ctrl Pts',(0.,-7.7987815792926,-1.78566510050039));
#45587=CARTESIAN_POINT('Ctrl Pts',(1.5,-7.7987815792926,-1.78566510050039));
#45588=CARTESIAN_POINT('Ctrl Pts',(0.,-7.76669643437116,-1.92042195163732));
#45589=CARTESIAN_POINT('Ctrl Pts',(1.5,-7.76669643437116,-1.92042195163732));
#45590=CARTESIAN_POINT('Ctrl Pts',(0.,-7.73228298072794,-2.05460309657555));
#45591=CARTESIAN_POINT('Ctrl Pts',(1.5,-7.73228298072794,-2.05460309657555));
#45592=CARTESIAN_POINT('Ctrl Pts',(0.,-7.69555153461053,-2.18816831029048));
#45593=CARTESIAN_POINT('Ctrl Pts',(1.5,-7.69555153461053,-2.18816831029048));
#45594=CARTESIAN_POINT('Ctrl Pts',(0.,-7.6565131076604,-2.32107755253582));
#45595=CARTESIAN_POINT('Ctrl Pts',(1.5,-7.6565131076604,-2.32107755253582));
#45596=CARTESIAN_POINT('Ctrl Pts',(0.,-7.61517940311072,-2.45329097970447));
#45597=CARTESIAN_POINT('Ctrl Pts',(1.5,-7.61517940311072,-2.45329097970447));
#45598=CARTESIAN_POINT('Ctrl Pts',(0.,-7.57156281202747,-2.58476895670164));
#45599=CARTESIAN_POINT('Ctrl Pts',(1.5,-7.57156281202747,-2.58476895670164));
#45600=CARTESIAN_POINT('Ctrl Pts',(0.,-7.52567640959347,-2.71547206883096));
#45601=CARTESIAN_POINT('Ctrl Pts',(1.5,-7.52567640959347,-2.71547206883096));
#45602=CARTESIAN_POINT('Ctrl Pts',(0.,-7.47753395143517,-2.8453611336944));
#45603=CARTESIAN_POINT('Ctrl Pts',(1.5,-7.47753395143517,-2.8453611336944));
#45604=CARTESIAN_POINT('Ctrl Pts',(0.,-7.42714986999194,-2.97439721310677));
#45605=CARTESIAN_POINT('Ctrl Pts',(1.5,-7.42714986999194,-2.97439721310677));
#45606=CARTESIAN_POINT('Ctrl Pts',(0.,-7.37453926970263,-3.10254162458336));
#45607=CARTESIAN_POINT('Ctrl Pts',(1.5,-7.37453926970263,-3.10254162458336));
#45608=CARTESIAN_POINT('Ctrl Pts',(0.,-7.31971792223413,-3.22975595284362));
#45609=CARTESIAN_POINT('Ctrl Pts',(1.5,-7.31971792223413,-3.22975595284362));
#45610=CARTESIAN_POINT('Ctrl Pts',(0.,-7.26270226175159,-3.35600206133147));
#45611=CARTESIAN_POINT('Ctrl Pts',(1.5,-7.26270226175159,-3.35600206133147));
#45612=CARTESIAN_POINT('Ctrl Pts',(0.,-7.20350938023008,-3.48124210375305));
#45613=CARTESIAN_POINT('Ctrl Pts',(1.5,-7.20350938023008,-3.48124210375305));
#45614=CARTESIAN_POINT('Ctrl Pts',(0.,-7.14215702280731,-3.60543853563268));
#45615=CARTESIAN_POINT('Ctrl Pts',(1.5,-7.14215702280731,-3.60543853563268));
#45616=CARTESIAN_POINT('Ctrl Pts',(0.,-7.07866358199493,-3.72855412534125));
#45617=CARTESIAN_POINT('Ctrl Pts',(1.5,-7.07866358199493,-3.72855412534125));
#45618=CARTESIAN_POINT('Ctrl Pts',(0.,-7.01304809193044,-3.85055196514423));
#45619=CARTESIAN_POINT('Ctrl Pts',(1.5,-7.01304809193044,-3.85055196514423));
#45620=CARTESIAN_POINT('Ctrl Pts',(0.,-6.94533022266893,-3.97139548226995));
#45621=CARTESIAN_POINT('Ctrl Pts',(1.5,-6.94533022266893,-3.97139548226995));
#45622=CARTESIAN_POINT('Ctrl Pts',(0.,-6.8755302745147,-4.09104844999872));
#45623=CARTESIAN_POINT('Ctrl Pts',(1.5,-6.8755302745147,-4.09104844999872));
#45624=CARTESIAN_POINT('Ctrl Pts',(0.,-6.80366917239217,-4.20947499877361));
#45625=CARTESIAN_POINT('Ctrl Pts',(1.5,-6.80366917239217,-4.20947499877361));
#45626=CARTESIAN_POINT('Ctrl Pts',(0.,-6.7297684591254,-4.32663962668727));
#45627=CARTESIAN_POINT('Ctrl Pts',(1.5,-6.7297684591254,-4.32663962668727));
#45628=CARTESIAN_POINT('Ctrl Pts',(0.,-6.65385028875609,-4.44250720999139));
#45629=CARTESIAN_POINT('Ctrl Pts',(1.5,-6.65385028875609,-4.44250720999139));
#45630=CARTESIAN_POINT('Ctrl Pts',(0.,-6.57593741989978,-4.55704301363008));
#45631=CARTESIAN_POINT('Ctrl Pts',(1.5,-6.57593741989978,-4.55704301363008));
#45632=CARTESIAN_POINT('Ctrl Pts',(0.,-6.49605320913988,-4.67021270179723));
#45633=CARTESIAN_POINT('Ctrl Pts',(1.5,-6.49605320913988,-4.67021270179723));
#45634=CARTESIAN_POINT('Ctrl Pts',(0.,-6.41422160445912,-4.78198234851915));
#45635=CARTESIAN_POINT('Ctrl Pts',(1.5,-6.41422160445912,-4.78198234851915));
#45636=CARTESIAN_POINT('Ctrl Pts',(0.,-6.33046713763739,-4.89231844752076));
#45637=CARTESIAN_POINT('Ctrl Pts',(1.5,-6.33046713763739,-4.89231844752076));
#45638=CARTESIAN_POINT('Ctrl Pts',(0.,-6.24481491668607,-5.00118792211809));
#45639=CARTESIAN_POINT('Ctrl Pts',(1.5,-6.24481491668607,-5.00118792211809));
#45640=CARTESIAN_POINT('Ctrl Pts',(0.,-6.15729061831839,-5.10855813513767));
#45641=CARTESIAN_POINT('Ctrl Pts',(1.5,-6.15729061831839,-5.10855813513767));
#45642=CARTESIAN_POINT('Ctrl Pts',(0.,-6.06792048045539,-5.21439689886329));
#45643=CARTESIAN_POINT('Ctrl Pts',(1.5,-6.06792048045539,-5.21439689886329));
#45644=CARTESIAN_POINT('Ctrl Pts',(0.,-5.97673129476691,-5.31867248501106));
#45645=CARTESIAN_POINT('Ctrl Pts',(1.5,-5.97673129476691,-5.31867248501106));
#45646=CARTESIAN_POINT('Ctrl Pts',(0.,-5.88375039824476,-5.42135363390127));
#45647=CARTESIAN_POINT('Ctrl Pts',(1.5,-5.88375039824476,-5.42135363390127));
#45648=CARTESIAN_POINT('Ctrl Pts',(0.,-5.78900566481012,-5.52240956365984));
#45649=CARTESIAN_POINT('Ctrl Pts',(1.5,-5.78900566481012,-5.52240956365984));
#45650=CARTESIAN_POINT('Ctrl Pts',(0.,-5.69252549695442,-5.62180997944938));
#45651=CARTESIAN_POINT('Ctrl Pts',(1.5,-5.69252549695442,-5.62180997944938));
#45652=CARTESIAN_POINT('Ctrl Pts',(0.,-5.59433881741333,-5.71952508273083));
#45653=CARTESIAN_POINT('Ctrl Pts',(1.5,-5.59433881741333,-5.71952508273083));
#45654=CARTESIAN_POINT('Ctrl Pts',(0.,-5.4944750608732,-5.81552558055602));
#45655=CARTESIAN_POINT('Ctrl Pts',(1.5,-5.4944750608732,-5.81552558055602));
#45656=CARTESIAN_POINT('Ctrl Pts',(0.,-5.39296416478281,-5.90978269397678));
#45657=CARTESIAN_POINT('Ctrl Pts',(1.5,-5.39296416478281,-5.90978269397678));
#45658=CARTESIAN_POINT('Ctrl Pts',(0.,-5.28983656019654,-6.00226816648613));
#45659=CARTESIAN_POINT('Ctrl Pts',(1.5,-5.28983656019654,-6.00226816648613));
#45660=CARTESIAN_POINT('Ctrl Pts',(0.,-5.18512316264843,-6.09295427249209));
#45661=CARTESIAN_POINT('Ctrl Pts',(1.5,-5.18512316264843,-6.09295427249209));
#45662=CARTESIAN_POINT('Ctrl Pts',(0.,-5.07885536305647,-6.18181382582471));
#45663=CARTESIAN_POINT('Ctrl Pts',(1.5,-5.07885536305647,-6.18181382582471));
#45664=CARTESIAN_POINT('Ctrl Pts',(0.,-4.9710650186567,-6.26882018827681));
#45665=CARTESIAN_POINT('Ctrl Pts',(1.5,-4.9710650186567,-6.26882018827681));
#45666=CARTESIAN_POINT('Ctrl Pts',(0.,-4.86178444312227,-6.3539472771871));
#45667=CARTESIAN_POINT('Ctrl Pts',(1.5,-4.86178444312227,-6.3539472771871));
#45668=CARTESIAN_POINT('Ctrl Pts',(0.,-4.75104639671106,-6.43716957305797));
#45669=CARTESIAN_POINT('Ctrl Pts',(1.5,-4.75104639671106,-6.43716957305797));
#45670=CARTESIAN_POINT('Ctrl Pts',(0.,-4.63888407644128,-6.51846212720856));
#45671=CARTESIAN_POINT('Ctrl Pts',(1.5,-4.63888407644128,-6.51846212720856));
#45672=CARTESIAN_POINT('Ctrl Pts',(0.,-4.52533110629424,-6.59780056946339));
#45673=CARTESIAN_POINT('Ctrl Pts',(1.5,-4.52533110629424,-6.59780056946339));
#45674=CARTESIAN_POINT('Ctrl Pts',(0.,-4.41042152744394,-6.67516111587727));
#45675=CARTESIAN_POINT('Ctrl Pts',(1.5,-4.41042152744394,-6.67516111587727));
#45676=CARTESIAN_POINT('Ctrl Pts',(0.,-4.29418978775745,-6.75052057543572));
#45677=CARTESIAN_POINT('Ctrl Pts',(1.5,-4.29418978775745,-6.75052057543572));
#45678=CARTESIAN_POINT('Ctrl Pts',(0.,-4.17667073132073,-6.82385635679236));
#45679=CARTESIAN_POINT('Ctrl Pts',(1.5,-4.17667073132073,-6.82385635679236));
#45680=CARTESIAN_POINT('Ctrl Pts',(0.,-4.0578995879893,-6.89514647504383));
#45681=CARTESIAN_POINT('Ctrl Pts',(1.5,-4.0578995879893,-6.89514647504383));
#45682=CARTESIAN_POINT('Ctrl Pts',(0.,-3.93791196296294,-6.96436955854269));
#45683=CARTESIAN_POINT('Ctrl Pts',(1.5,-3.93791196296294,-6.96436955854269));
#45684=CARTESIAN_POINT('Ctrl Pts',(0.,-3.81674382638391,-7.03150485574852));
#45685=CARTESIAN_POINT('Ctrl Pts',(1.5,-3.81674382638391,-7.03150485574852));
#45686=CARTESIAN_POINT('Ctrl Pts',(0.,-3.69443150229741,-7.09653224099531));
#45687=CARTESIAN_POINT('Ctrl Pts',(1.5,-3.69443150229741,-7.09653224099531));
#45688=CARTESIAN_POINT('Ctrl Pts',(0.,-3.57101165763407,-7.15943222029805));
#45689=CARTESIAN_POINT('Ctrl Pts',(1.5,-3.57101165763407,-7.15943222029805));
#45690=CARTESIAN_POINT('Ctrl Pts',(0.,-3.44652129121395,-7.22018593719866));
#45691=CARTESIAN_POINT('Ctrl Pts',(1.5,-3.44652129121395,-7.22018593719866));
#45692=CARTESIAN_POINT('Ctrl Pts',(0.,-3.32099772277122,-7.27877517865193));
#45693=CARTESIAN_POINT('Ctrl Pts',(1.5,-3.32099772277122,-7.27877517865193));
#45694=CARTESIAN_POINT('Ctrl Pts',(0.,-3.19447858199892,-7.33518238095157));
#45695=CARTESIAN_POINT('Ctrl Pts',(1.5,-3.19447858199892,-7.33518238095157));
#45696=CARTESIAN_POINT('Ctrl Pts',(0.,-3.06700179705205,-7.38939063452155));
#45697=CARTESIAN_POINT('Ctrl Pts',(1.5,-3.06700179705205,-7.38939063452155));
#45698=CARTESIAN_POINT('Ctrl Pts',(0.,-2.93860558306928,-7.44138368874846));
#45699=CARTESIAN_POINT('Ctrl Pts',(1.5,-2.93860558306928,-7.44138368874846));
#45700=CARTESIAN_POINT('Ctrl Pts',(0.,-2.80932843071268,-7.49114595685492));
#45701=CARTESIAN_POINT('Ctrl Pts',(1.5,-2.80932843071268,-7.49114595685492));
#45702=CARTESIAN_POINT('Ctrl Pts',(0.,-2.67920909472461,-7.53866252081456));
#45703=CARTESIAN_POINT('Ctrl Pts',(1.5,-2.67920909472461,-7.53866252081456));
#45704=CARTESIAN_POINT('Ctrl Pts',(0.,-2.54828658250114,-7.58391913630888));
#45705=CARTESIAN_POINT('Ctrl Pts',(1.5,-2.54828658250114,-7.58391913630888));
#45706=CARTESIAN_POINT('Ctrl Pts',(0.,-2.41660014222393,-7.62690223650621));
#45707=CARTESIAN_POINT('Ctrl Pts',(1.5,-2.41660014222393,-7.62690223650621));
#45708=CARTESIAN_POINT('Ctrl Pts',(0.,-2.28418925100709,-7.66759893588327));
#45709=CARTESIAN_POINT('Ctrl Pts',(1.5,-2.28418925100709,-7.66759893588327));
#45710=CARTESIAN_POINT('Ctrl Pts',(0.,-2.15109360305841,-7.70599703408915));
#45711=CARTESIAN_POINT('Ctrl Pts',(1.5,-2.15109360305841,-7.70599703408915));
#45712=CARTESIAN_POINT('Ctrl Pts',(0.,-2.01735309785409,-7.74208501985227));
#45713=CARTESIAN_POINT('Ctrl Pts',(1.5,-2.01735309785409,-7.74208501985227));
#45714=CARTESIAN_POINT('Ctrl Pts',(0.,-1.88300782832642,-7.77585207493021));
#45715=CARTESIAN_POINT('Ctrl Pts',(1.5,-1.88300782832642,-7.77585207493021));
#45716=CARTESIAN_POINT('Ctrl Pts',(0.,-1.74809806871328,-7.80728807684922));
#45717=CARTESIAN_POINT('Ctrl Pts',(1.5,-1.74809806871328,-7.80728807684922));
#45718=CARTESIAN_POINT('Ctrl Pts',(0.,-1.61266426241909,-7.83638360168719));
#45719=CARTESIAN_POINT('Ctrl Pts',(1.5,-1.61266426241909,-7.83638360168719));
#45720=CARTESIAN_POINT('Ctrl Pts',(0.,-1.47674700988627,-7.86312992690011));
#45721=CARTESIAN_POINT('Ctrl Pts',(1.5,-1.47674700988627,-7.86312992690011));
#45722=CARTESIAN_POINT('Ctrl Pts',(0.,-1.34038705647653,-7.88751903419248));
#45723=CARTESIAN_POINT('Ctrl Pts',(1.5,-1.34038705647653,-7.88751903419248));
#45724=CARTESIAN_POINT('Ctrl Pts',(0.,-1.20362528036119,-7.90954361243176));
#45725=CARTESIAN_POINT('Ctrl Pts',(1.5,-1.20362528036119,-7.90954361243176));
#45726=CARTESIAN_POINT('Ctrl Pts',(0.,-1.06650268017935,-7.92919705932551));
#45727=CARTESIAN_POINT('Ctrl Pts',(1.5,-1.06650268017935,-7.92919705932551));
#45728=CARTESIAN_POINT('Ctrl Pts',(0.,-0.929060362703573,-7.94647348314288));
#45729=CARTESIAN_POINT('Ctrl Pts',(1.5,-0.929060362703573,-7.94647348314288));
#45730=CARTESIAN_POINT('Ctrl Pts',(0.,-0.791339530512307,-7.96136770448042));
#45731=CARTESIAN_POINT('Ctrl Pts',(1.5,-0.791339530512307,-7.96136770448042));
#45732=CARTESIAN_POINT('Ctrl Pts',(0.,-0.653381469668319,-7.97387525807254));
#45733=CARTESIAN_POINT('Ctrl Pts',(1.5,-0.653381469668319,-7.97387525807254));
#45734=CARTESIAN_POINT('Ctrl Pts',(0.,-0.515227537402346,-7.98399239464636));
#45735=CARTESIAN_POINT('Ctrl Pts',(1.5,-0.515227537402346,-7.98399239464636));
#45736=CARTESIAN_POINT('Ctrl Pts',(0.,-0.376919149672593,-7.99171608152895));
#45737=CARTESIAN_POINT('Ctrl Pts',(1.5,-0.376919149672593,-7.99171608152895));
#45738=CARTESIAN_POINT('Ctrl Pts',(0.,-0.238497768727867,-7.99704400329913));
#45739=CARTESIAN_POINT('Ctrl Pts',(1.5,-0.238497768727867,-7.99704400329913));
#45740=CARTESIAN_POINT('Ctrl Pts',(0.,-0.100004890673634,-7.99997456248423));
#45741=CARTESIAN_POINT('Ctrl Pts',(1.5,-0.100004890673634,-7.99997456248423));
#45742=CARTESIAN_POINT('Ctrl Pts',(0.,0.0385179669597413,-8.00050688030175));
#45743=CARTESIAN_POINT('Ctrl Pts',(1.5,0.0385179669597413,-8.00050688030175));
#45744=CARTESIAN_POINT('Ctrl Pts',(0.,0.177029277647508,-7.99864079744583));
#45745=CARTESIAN_POINT('Ctrl Pts',(1.5,0.177029277647508,-7.99864079744583));
#45746=CARTESIAN_POINT('Ctrl Pts',(0.,0.31548751831724,-7.99437687360868));
#45747=CARTESIAN_POINT('Ctrl Pts',(1.5,0.31548751831724,-7.99437687360868));
#45748=CARTESIAN_POINT('Ctrl Pts',(0.,0.453851181795815,-7.98771638704679));
#45749=CARTESIAN_POINT('Ctrl Pts',(1.5,0.453851181795815,-7.98771638704679));
#45750=CARTESIAN_POINT('Ctrl Pts',(0.,0.59207878925734,-7.97866133419203));
#45751=CARTESIAN_POINT('Ctrl Pts',(1.5,0.59207878925734,-7.97866133419203));
#45752=CARTESIAN_POINT('Ctrl Pts',(0.,0.730128902672901,-7.9672144293078));
#45753=CARTESIAN_POINT('Ctrl Pts',(1.5,0.730128902672901,-7.9672144293078));
#45754=CARTESIAN_POINT('Ctrl Pts',(0.,0.867960137262859,-7.95337910418991));
#45755=CARTESIAN_POINT('Ctrl Pts',(1.5,0.867960137262859,-7.95337910418991));
#45756=CARTESIAN_POINT('Ctrl Pts',(0.,1.00553117385478,-7.9371595066318));
#45757=CARTESIAN_POINT('Ctrl Pts',(1.5,1.00553117385478,-7.9371595066318));
#45758=CARTESIAN_POINT('Ctrl Pts',(0.,1.14280077124549,-7.91856049893449));
#45759=CARTESIAN_POINT('Ctrl Pts',(1.5,1.14280077124549,-7.91856049893449));
#45760=CARTESIAN_POINT('Ctrl Pts',(0.,1.27972777856801,-7.89758765646115));
#45761=CARTESIAN_POINT('Ctrl Pts',(1.5,1.27972777856801,-7.89758765646115));
#45762=CARTESIAN_POINT('Ctrl Pts',(0.,1.41627114766405,-7.87424726623619));
#45763=CARTESIAN_POINT('Ctrl Pts',(1.5,1.41627114766405,-7.87424726623619));
#45764=CARTESIAN_POINT('Ctrl Pts',(0.,1.55238994546304,-7.8485463255889));
#45765=CARTESIAN_POINT('Ctrl Pts',(1.5,1.55238994546304,-7.8485463255889));
#45766=CARTESIAN_POINT('Ctrl Pts',(0.,1.68804336616293,-7.8204925395136));
#45767=CARTESIAN_POINT('Ctrl Pts',(1.5,1.68804336616293,-7.8204925395136));
#45768=CARTESIAN_POINT('Ctrl Pts',(0.,1.823190743419,-7.79009431807374));
#45769=CARTESIAN_POINT('Ctrl Pts',(1.5,1.823190743419,-7.79009431807374));
#45770=CARTESIAN_POINT('Ctrl Pts',(0.,1.95779156254127,-7.7573607738503));
#45771=CARTESIAN_POINT('Ctrl Pts',(1.5,1.95779156254127,-7.7573607738503));
#45772=CARTESIAN_POINT('Ctrl Pts',(0.,2.09180547270151,-7.72230171943405));
#45773=CARTESIAN_POINT('Ctrl Pts',(1.5,2.09180547270151,-7.72230171943405));
#45774=CARTESIAN_POINT('Ctrl Pts',(0.,2.22519229915041,-7.68492766496142));
#45775=CARTESIAN_POINT('Ctrl Pts',(1.5,2.22519229915041,-7.68492766496142));
#45776=CARTESIAN_POINT('Ctrl Pts',(0.,2.35791205512021,-7.6452498145298));
#45777=CARTESIAN_POINT('Ctrl Pts',(1.5,2.35791205512021,-7.6452498145298));
#45778=CARTESIAN_POINT('Ctrl Pts',(0.,2.48992495373911,-7.60328006265592));
#45779=CARTESIAN_POINT('Ctrl Pts',(1.5,2.48992495373911,-7.60328006265592));
#45780=CARTESIAN_POINT('Ctrl Pts',(0.,2.62119141995809,-7.55903099077771));
#45781=CARTESIAN_POINT('Ctrl Pts',(1.5,2.62119141995809,-7.55903099077771));
#45782=CARTESIAN_POINT('Ctrl Pts',(0.,2.75167210249111,-7.51251586379867));
#45783=CARTESIAN_POINT('Ctrl Pts',(1.5,2.75167210249111,-7.51251586379867));
#45784=CARTESIAN_POINT('Ctrl Pts',(0.,2.88132788576913,-7.4637486266753));
#45785=CARTESIAN_POINT('Ctrl Pts',(1.5,2.88132788576913,-7.4637486266753));
#45786=CARTESIAN_POINT('Ctrl Pts',(0.,3.01011990149821,-7.41274389958788));
#45787=CARTESIAN_POINT('Ctrl Pts',(1.5,3.01011990149821,-7.41274389958788));
#45788=CARTESIAN_POINT('Ctrl Pts',(0.,3.13800954023306,-7.35951697315347));
#45789=CARTESIAN_POINT('Ctrl Pts',(1.5,3.13800954023306,-7.35951697315347));
#45790=CARTESIAN_POINT('Ctrl Pts',(0.,3.26495846296673,-7.30408380368086));
#45791=CARTESIAN_POINT('Ctrl Pts',(1.5,3.26495846296673,-7.30408380368086));
#45792=CARTESIAN_POINT('Ctrl Pts',(0.,3.3909286127372,-7.24646100846717));
#45793=CARTESIAN_POINT('Ctrl Pts',(1.5,3.3909286127372,-7.24646100846717));
#45794=CARTESIAN_POINT('Ctrl Pts',(0.,3.51588222625169,-7.18666586113568));
#45795=CARTESIAN_POINT('Ctrl Pts',(1.5,3.51588222625169,-7.18666586113568));
#45796=CARTESIAN_POINT('Ctrl Pts',(0.,3.63978184496066,-7.12471628635636));
#45797=CARTESIAN_POINT('Ctrl Pts',(1.5,3.63978184496066,-7.12471628635636));
#45798=CARTESIAN_POINT('Ctrl Pts',(0.,3.76259032615096,-7.06063085460692));
#45799=CARTESIAN_POINT('Ctrl Pts',(1.5,3.76259032615096,-7.06063085460692));
#45800=CARTESIAN_POINT('Ctrl Pts',(0.,3.88427085405865,-6.99442877697438));
#45801=CARTESIAN_POINT('Ctrl Pts',(1.5,3.88427085405865,-6.99442877697438));
#45802=CARTESIAN_POINT('Ctrl Pts',(0.,4.00478695100224,-6.92612989999653));
#45803=CARTESIAN_POINT('Ctrl Pts',(1.5,4.00478695100224,-6.92612989999653));
#45804=CARTESIAN_POINT('Ctrl Pts',(0.,4.12410248853711,-6.85575470054316));
#45805=CARTESIAN_POINT('Ctrl Pts',(1.5,4.12410248853711,-6.85575470054316));
#45806=CARTESIAN_POINT('Ctrl Pts',(0.,4.24218169808549,-6.78332427836585));
#45807=CARTESIAN_POINT('Ctrl Pts',(1.5,4.24218169808549,-6.78332427836585));
#45808=CARTESIAN_POINT('Ctrl Pts',(0.,4.35898918158893,-6.70886034868655));
#45809=CARTESIAN_POINT('Ctrl Pts',(1.5,4.35898918158893,-6.70886034868655));
#45810=CARTESIAN_POINT('Ctrl Pts',(0.,4.47448992218382,-6.6323852348247));
#45811=CARTESIAN_POINT('Ctrl Pts',(1.5,4.47448992218382,-6.6323852348247));
#45812=CARTESIAN_POINT('Ctrl Pts',(0.,4.58864929490088,-6.55392186086227));
#45813=CARTESIAN_POINT('Ctrl Pts',(1.5,4.58864929490088,-6.55392186086227));
#45814=CARTESIAN_POINT('Ctrl Pts',(0.,4.70143307738904,-6.47349374434655));
#45815=CARTESIAN_POINT('Ctrl Pts',(1.5,4.70143307738904,-6.47349374434655));
#45816=CARTESIAN_POINT('Ctrl Pts',(0.,4.8128074597363,-6.39112499081239));
#45817=CARTESIAN_POINT('Ctrl Pts',(1.5,4.8128074597363,-6.39112499081239));
#45818=CARTESIAN_POINT('Ctrl Pts',(0.,4.92273905431645,-6.3068402883412));
#45819=CARTESIAN_POINT('Ctrl Pts',(1.5,4.92273905431645,-6.3068402883412));
#45820=CARTESIAN_POINT('Ctrl Pts',(0.,5.03119490566203,-6.22066490215631));
#45821=CARTESIAN_POINT('Ctrl Pts',(1.5,5.03119490566203,-6.22066490215631));
#45822=CARTESIAN_POINT('Ctrl Pts',(0.,5.13814250036441,-6.13262466925436));
#45823=CARTESIAN_POINT('Ctrl Pts',(1.5,5.13814250036441,-6.13262466925436));
#45824=CARTESIAN_POINT('Ctrl Pts',(0.,5.24354977700144,-6.04274599307227));
#45825=CARTESIAN_POINT('Ctrl Pts',(1.5,5.24354977700144,-6.04274599307227));
#45826=CARTESIAN_POINT('Ctrl Pts',(0.,5.34738513573851,-5.95105583052982));
#45827=CARTESIAN_POINT('Ctrl Pts',(1.5,5.34738513573851,-5.95105583052982));
#45828=CARTESIAN_POINT('Ctrl Pts',(0.,5.44961744795835,-5.85758167910657));
#45829=CARTESIAN_POINT('Ctrl Pts',(1.5,5.44961744795835,-5.85758167910657));
#45830=CARTESIAN_POINT('Ctrl Pts',(0.,5.55021606592032,-5.76235156395272));
#45831=CARTESIAN_POINT('Ctrl Pts',(1.5,5.55021606592032,-5.76235156395272));
#45832=CARTESIAN_POINT('Ctrl Pts',(0.,5.6491508324498,-5.66539402503311));
#45833=CARTESIAN_POINT('Ctrl Pts',(1.5,5.6491508324498,-5.66539402503311));
#45834=CARTESIAN_POINT('Ctrl Pts',(0.,5.74639209065813,-5.56673810430373));
#45835=CARTESIAN_POINT('Ctrl Pts',(1.5,5.74639209065813,-5.56673810430373));
#45836=CARTESIAN_POINT('Ctrl Pts',(0.,5.84191069171249,-5.46641334741991));
#45837=CARTESIAN_POINT('Ctrl Pts',(1.5,5.84191069171249,-5.46641334741991));
#45838=CARTESIAN_POINT('Ctrl Pts',(0.,5.93567800263758,-5.3644498054763));
#45839=CARTESIAN_POINT('Ctrl Pts',(1.5,5.93567800263758,-5.3644498054763));
#45840=CARTESIAN_POINT('Ctrl Pts',(0.,6.02766591414951,-5.26087803677827));
#45841=CARTESIAN_POINT('Ctrl Pts',(1.5,6.02766591414951,-5.26087803677827));
#45842=CARTESIAN_POINT('Ctrl Pts',(0.,6.11784684852245,-5.15572910864454));
#45843=CARTESIAN_POINT('Ctrl Pts',(1.5,6.11784684852245,-5.15572910864454));
#45844=CARTESIAN_POINT('Ctrl Pts',(0.,6.20619376748852,-5.04903459924103));
#45845=CARTESIAN_POINT('Ctrl Pts',(1.5,6.20619376748852,-5.04903459924103));
#45846=CARTESIAN_POINT('Ctrl Pts',(0.,6.29268018169352,-4.94082656273383));
#45847=CARTESIAN_POINT('Ctrl Pts',(1.5,6.29268018169352,-4.94082656273383));
#45848=CARTESIAN_POINT('Ctrl Pts',(0.,6.37728016018695,-4.83113749447141));
#45849=CARTESIAN_POINT('Ctrl Pts',(1.5,6.37728016018695,-4.83113749447141));
#45850=CARTESIAN_POINT('Ctrl Pts',(0.,6.45996833994694,-4.72000029619493));
#45851=CARTESIAN_POINT('Ctrl Pts',(1.5,6.45996833994694,-4.72000029619493));
#45852=CARTESIAN_POINT('Ctrl Pts',(0.,6.54071993544062,-4.60744824127475));
#45853=CARTESIAN_POINT('Ctrl Pts',(1.5,6.54071993544062,-4.60744824127475));
#45854=CARTESIAN_POINT('Ctrl Pts',(0.,6.61951074822048,-4.49351493997171));
#45855=CARTESIAN_POINT('Ctrl Pts',(1.5,6.61951074822048,-4.49351493997171));
#45856=CARTESIAN_POINT('Ctrl Pts',(0.,6.69631716969172,-4.37823438722894));
#45857=CARTESIAN_POINT('Ctrl Pts',(1.5,6.69631716969172,-4.37823438722894));
#45858=CARTESIAN_POINT('Ctrl Pts',(0.,6.77111618391648,-4.26164101048826));
#45859=CARTESIAN_POINT('Ctrl Pts',(1.5,6.77111618391648,-4.26164101048826));
#45860=CARTESIAN_POINT('Ctrl Pts',(0.,6.84388537045513,-4.14376971753304));
#45861=CARTESIAN_POINT('Ctrl Pts',(1.5,6.84388537045513,-4.14376971753304));
#45862=CARTESIAN_POINT('Ctrl Pts',(0.,6.91460290724495,-4.02465594435878));
#45863=CARTESIAN_POINT('Ctrl Pts',(1.5,6.91460290724495,-4.02465594435878));
#45864=CARTESIAN_POINT('Ctrl Pts',(0.,6.98324757351635,-3.90433570307326));
#45865=CARTESIAN_POINT('Ctrl Pts',(1.5,6.98324757351635,-3.90433570307326));
#45866=CARTESIAN_POINT('Ctrl Pts',(0.,7.04979876513603,-3.78284543574385));
#45867=CARTESIAN_POINT('Ctrl Pts',(1.5,7.04979876513603,-3.78284543574385));
#45868=CARTESIAN_POINT('Ctrl Pts',(0.,7.11423650998851,-3.66022186827001));
#45869=CARTESIAN_POINT('Ctrl Pts',(1.5,7.11423650998851,-3.66022186827001));
#45870=CARTESIAN_POINT('Ctrl Pts',(0.,7.17654148339738,-3.53650186427521));
#45871=CARTESIAN_POINT('Ctrl Pts',(1.5,7.17654148339738,-3.53650186427521));
#45872=CARTESIAN_POINT('Ctrl Pts',(0.,7.23669502358634,-3.41172227901257));
#45873=CARTESIAN_POINT('Ctrl Pts',(1.5,7.23669502358634,-3.41172227901257));
#45874=CARTESIAN_POINT('Ctrl Pts',(0.,7.29467914718136,-3.28591981327804));
#45875=CARTESIAN_POINT('Ctrl Pts',(1.5,7.29467914718136,-3.28591981327804));
#45876=CARTESIAN_POINT('Ctrl Pts',(0.,7.350476532226,-3.15913131592765));
#45877=CARTESIAN_POINT('Ctrl Pts',(1.5,7.350476532226,-3.15913131592765));
#45878=CARTESIAN_POINT('Ctrl Pts',(0.,7.40407050123789,-3.03139408640772));
#45879=CARTESIAN_POINT('Ctrl Pts',(1.5,7.40407050123789,-3.03139408640772));
#45880=CARTESIAN_POINT('Ctrl Pts',(0.,7.45544500430585,-2.90274617730943));
#45881=CARTESIAN_POINT('Ctrl Pts',(1.5,7.45544500430585,-2.90274617730943));
#45882=CARTESIAN_POINT('Ctrl Pts',(0.,7.5045846022269,-2.7732266969588));
#45883=CARTESIAN_POINT('Ctrl Pts',(1.5,7.5045846022269,-2.7732266969588));
#45884=CARTESIAN_POINT('Ctrl Pts',(0.,7.55147444968283,-2.64287611205352));
#45885=CARTESIAN_POINT('Ctrl Pts',(1.5,7.55147444968283,-2.64287611205352));
#45886=CARTESIAN_POINT('Ctrl Pts',(0.,7.5961003500545,-2.51173550715636));
#45887=CARTESIAN_POINT('Ctrl Pts',(1.5,7.5961003500545,-2.51173550715636));
#45888=CARTESIAN_POINT('Ctrl Pts',(0.,7.638448810277,-2.37984584421852));
#45889=CARTESIAN_POINT('Ctrl Pts',(1.5,7.638448810277,-2.37984584421852));
#45890=CARTESIAN_POINT('Ctrl Pts',(0.,7.67850709573841,-2.24724722210384));
#45891=CARTESIAN_POINT('Ctrl Pts',(1.5,7.67850709573841,-2.24724722210384));
#45892=CARTESIAN_POINT('Ctrl Pts',(0.,7.71626328522396,-2.11397813608674));
#45893=CARTESIAN_POINT('Ctrl Pts',(1.5,7.71626328522396,-2.11397813608674));
#45894=CARTESIAN_POINT('Ctrl Pts',(0.,7.75170632590802,-1.98007473729369));
#45895=CARTESIAN_POINT('Ctrl Pts',(1.5,7.75170632590802,-1.98007473729369));
#45896=CARTESIAN_POINT('Ctrl Pts',(0.,7.78482591855345,-1.84557250184578));
#45897=CARTESIAN_POINT('Ctrl Pts',(1.5,7.78482591855345,-1.84557250184578));
#45898=CARTESIAN_POINT('Ctrl Pts',(0.,7.81561240275672,-1.71050789997943));
#45899=CARTESIAN_POINT('Ctrl Pts',(1.5,7.81561240275672,-1.71050789997943));
#45900=CARTESIAN_POINT('Ctrl Pts',(0.,7.84405664223427,-1.57492006520963));
#45901=CARTESIAN_POINT('Ctrl Pts',(1.5,7.84405664223427,-1.57492006520963));
#45902=CARTESIAN_POINT('Ctrl Pts',(0.,7.87014991014611,-1.43885246359668));
#45903=CARTESIAN_POINT('Ctrl Pts',(1.5,7.87014991014611,-1.43885246359668));
#45904=CARTESIAN_POINT('Ctrl Pts',(0.,7.89388377445188,-1.30235456318281));
#45905=CARTESIAN_POINT('Ctrl Pts',(1.5,7.89388377445188,-1.30235456318281));
#45906=CARTESIAN_POINT('Ctrl Pts',(0.,7.91525036159865,-1.16547817540872));
#45907=CARTESIAN_POINT('Ctrl Pts',(1.5,7.91525036159865,-1.16547817540872));
#45908=CARTESIAN_POINT('Ctrl Pts',(0.,7.93424262024687,-1.0282737966247));
#45909=CARTESIAN_POINT('Ctrl Pts',(1.5,7.93424262024687,-1.0282737966247));
#45910=CARTESIAN_POINT('Ctrl Pts',(0.,7.95085458504517,-0.890786949553448));
#45911=CARTESIAN_POINT('Ctrl Pts',(1.5,7.95085458504517,-0.890786949553448));
#45912=CARTESIAN_POINT('Ctrl Pts',(0.,7.96508164046348,-0.753054524569566));
#45913=CARTESIAN_POINT('Ctrl Pts',(1.5,7.96508164046348,-0.753054524569566));
#45914=CARTESIAN_POINT('Ctrl Pts',(0.,7.97692078469519,-0.615101120652533));
#45915=CARTESIAN_POINT('Ctrl Pts',(1.5,7.97692078469519,-0.615101120652533));
#45916=CARTESIAN_POINT('Ctrl Pts',(0.,7.98637028879241,-0.476941502740932));
#45917=CARTESIAN_POINT('Ctrl Pts',(1.5,7.98637028879241,-0.476941502740932));
#45918=CARTESIAN_POINT('Ctrl Pts',(0.,7.99201754245236,-0.366254747519825));
#45919=CARTESIAN_POINT('Ctrl Pts',(1.5,7.99201754245236,-0.366254747519825));
#45920=CARTESIAN_POINT('Ctrl Pts',(0.,7.99517719352919,-0.283151319739979));
#45921=CARTESIAN_POINT('Ctrl Pts',(1.5,7.99517719352919,-0.283151319739979));
#45922=CARTESIAN_POINT('Ctrl Pts',(0.,7.9968055050659,-0.227709763329173));
#45923=CARTESIAN_POINT('Ctrl Pts',(1.5,7.9968055050659,-0.227709763329173));
#45924=CARTESIAN_POINT('Ctrl Pts',(0.,7.99750013020562,-0.199979167317696));
#45925=CARTESIAN_POINT('Ctrl Pts',(1.5,7.99750013020562,-0.199979167317696));
#45926=CARTESIAN_POINT('',(0.15,7.99750013020562,0.199979167317619));
#45927=CARTESIAN_POINT('',(0.,7.99750013020562,0.199979167317699));
#45928=CARTESIAN_POINT('Ctrl Pts',(0.15,7.99749996249466,-0.19998586250798));
#45929=CARTESIAN_POINT('Ctrl Pts',(0.15,7.961995738416,-1.61732659559412));
#45930=CARTESIAN_POINT('Ctrl Pts',(0.15,7.12114441317228,-4.42734848781943));
#45931=CARTESIAN_POINT('Ctrl Pts',(0.15,3.90389095991274,-7.41867892302632));
#45932=CARTESIAN_POINT('Ctrl Pts',(0.15,-1.06985836751423,-8.53832254812639));
#45933=CARTESIAN_POINT('Ctrl Pts',(0.15,-6.34173425813201,-6.08127940476401));
#45934=CARTESIAN_POINT('Ctrl Pts',(0.15,-8.7127134194499,-0.24784357163776));
#45935=CARTESIAN_POINT('Ctrl Pts',(0.15,-6.73863305333642,5.52529506822021));
#45936=CARTESIAN_POINT('Ctrl Pts',(0.15,-3.09413630122569,7.64282159505089));
#45937=CARTESIAN_POINT('Ctrl Pts',(0.15,0.396398773959542,8.13986317370034));
#45938=CARTESIAN_POINT('Ctrl Pts',(0.15,3.56795524744049,7.62772577919895));
#45939=CARTESIAN_POINT('Ctrl Pts',(0.15,7.04944249732077,4.60837388453871));
#45940=CARTESIAN_POINT('Ctrl Pts',(0.15,7.96045345605701,1.67894428791899));
#45941=CARTESIAN_POINT('Ctrl Pts',(0.15,7.99750013020563,0.19997916731746));
#45942=CARTESIAN_POINT('Ctrl Pts',(0.15,7.99750013020563,0.19997916731746));
#45943=CARTESIAN_POINT('Ctrl Pts',(0.15,7.96045345605701,1.67894428791899));
#45944=CARTESIAN_POINT('Ctrl Pts',(0.15,7.04944249732077,4.60837388453871));
#45945=CARTESIAN_POINT('Ctrl Pts',(0.15,3.56795524744049,7.62772577919895));
#45946=CARTESIAN_POINT('Ctrl Pts',(0.15,0.396398773959542,8.13986317370034));
#45947=CARTESIAN_POINT('Ctrl Pts',(0.15,-3.09413630122569,7.64282159505089));
#45948=CARTESIAN_POINT('Ctrl Pts',(0.15,-6.73863305333642,5.52529506822021));
#45949=CARTESIAN_POINT('Ctrl Pts',(0.15,-8.7127134194499,-0.24784357163776));
#45950=CARTESIAN_POINT('Ctrl Pts',(0.15,-6.34173425813201,-6.08127940476401));
#45951=CARTESIAN_POINT('Ctrl Pts',(0.15,-1.06985836751423,-8.53832254812639));
#45952=CARTESIAN_POINT('Ctrl Pts',(0.15,3.90389095991274,-7.41867892302632));
#45953=CARTESIAN_POINT('Ctrl Pts',(0.15,7.12114441317228,-4.42734848781943));
#45954=CARTESIAN_POINT('Ctrl Pts',(0.15,7.961995738416,-1.61732659559412));
#45955=CARTESIAN_POINT('Ctrl Pts',(0.15,7.99749996249466,-0.19998586250798));
#45956=CARTESIAN_POINT('Ctrl Pts',(0.1,7.94751580920271,0.19872710746362));
#45957=CARTESIAN_POINT('Ctrl Pts',(0.0999999999999999,7.91068175784103,
1.66845202534325));
#45958=CARTESIAN_POINT('Ctrl Pts',(0.1,7.00539776889503,4.57959570636687));
#45959=CARTESIAN_POINT('Ctrl Pts',(0.1,3.54564541349769,7.58002805922958));
#45960=CARTESIAN_POINT('Ctrl Pts',(0.1,0.393922023965292,8.08901822676633));
#45961=CARTESIAN_POINT('Ctrl Pts',(0.1,-3.07480005979067,7.59502792370097));
#45962=CARTESIAN_POINT('Ctrl Pts',(0.1,-6.69651470180966,5.49077279428345));
#45963=CARTESIAN_POINT('Ctrl Pts',(0.1,-8.65825783268014,-0.246297266556145));
#45964=CARTESIAN_POINT('Ctrl Pts',(0.1,-6.30209920788036,-6.04327542832943));
#45965=CARTESIAN_POINT('Ctrl Pts',(0.1,-1.06317179958156,-8.48494793422131));
#45966=CARTESIAN_POINT('Ctrl Pts',(0.1,3.87948800454988,-7.37234199492993));
#45967=CARTESIAN_POINT('Ctrl Pts',(0.1,7.07664686572023,-4.39964468727081));
#45968=CARTESIAN_POINT('Ctrl Pts',(0.1,7.91220940446938,-1.60725513423082));
#45969=CARTESIAN_POINT('Ctrl Pts',(0.1,7.94751564253563,-0.198733760980932));
#45970=CARTESIAN_POINT('Ctrl Pts',(0.05,7.8975314881998,0.19747504760978));
#45971=CARTESIAN_POINT('Ctrl Pts',(0.0500000000000001,7.86096398282589,
1.6580628961152));
#45972=CARTESIAN_POINT('Ctrl Pts',(0.0499999999999999,6.96130852626912,
4.55073165493979));
#45973=CARTESIAN_POINT('Ctrl Pts',(0.0500000000000001,3.52336618735535,
7.53242134786548));
#45974=CARTESIAN_POINT('Ctrl Pts',(0.05,0.391442899960782,8.03808465462494));
#45975=CARTESIAN_POINT('Ctrl Pts',(0.05,-3.05545752250296,7.54731294656525));
#45976=CARTESIAN_POINT('Ctrl Pts',(0.05,-6.6544020560685,5.45621682823237));
#45977=CARTESIAN_POINT('Ctrl Pts',(0.05,-8.60380561359923,-0.244740933791259));
#45978=CARTESIAN_POINT('Ctrl Pts',(0.05,-6.26246183682716,-6.00526335382877));
#45979=CARTESIAN_POINT('Ctrl Pts',(0.05,-1.05648506055284,-8.43159806974257));
#45980=CARTESIAN_POINT('Ctrl Pts',(0.05,3.85509562628092,-7.32593505111813));
#45981=CARTESIAN_POINT('Ctrl Pts',(0.05,7.0321200317712,-4.37201968712336));
#45982=CARTESIAN_POINT('Ctrl Pts',(0.05,7.86249210118029,-1.59717501758574));
#45983=CARTESIAN_POINT('Ctrl Pts',(0.05,7.89753132257661,-0.197481659453884));
#45984=CARTESIAN_POINT('Ctrl Pts',(0.,7.84754716719688,0.19622298775594));
#45985=CARTESIAN_POINT('Ctrl Pts',(0.,7.81119228460991,1.64757063353946));
#45986=CARTESIAN_POINT('Ctrl Pts',(0.,6.91726379784338,4.52195347676795));
#45987=CARTESIAN_POINT('Ctrl Pts',(0.,3.50105635341255,7.48472362789611));
#45988=CARTESIAN_POINT('Ctrl Pts',(0.,0.388966149966533,7.98723970769094));
#45989=CARTESIAN_POINT('Ctrl Pts',(0.,-3.03612128106794,7.49951927521533));
#45990=CARTESIAN_POINT('Ctrl Pts',(0.,-6.61228370454174,5.42169455429562));
#45991=CARTESIAN_POINT('Ctrl Pts',(0.,-8.54935002682948,-0.243194628709643));
#45992=CARTESIAN_POINT('Ctrl Pts',(0.,-6.22282678657551,-5.96725937739419));
#45993=CARTESIAN_POINT('Ctrl Pts',(0.,-1.04979849262017,-8.37822345583749));
#45994=CARTESIAN_POINT('Ctrl Pts',(0.,3.83069267091806,-7.27959812302174));
#45995=CARTESIAN_POINT('Ctrl Pts',(0.,6.98762248431915,-4.34431588657474));
#45996=CARTESIAN_POINT('Ctrl Pts',(0.,7.81270576723367,-1.58710355622244));
#45997=CARTESIAN_POINT('Ctrl Pts',(0.,7.84754700261759,-0.196229557926836));
#45998=CARTESIAN_POINT('',(0.,7.84754700261759,0.196229557926824));
#45999=CARTESIAN_POINT('Ctrl Pts',(0.15,7.99750013020562,0.199979167317699));
#46000=CARTESIAN_POINT('Ctrl Pts',(0.1,7.94751580920271,0.198727107463857));
#46001=CARTESIAN_POINT('Ctrl Pts',(0.05,7.89753148819979,0.197475047610016));
#46002=CARTESIAN_POINT('Ctrl Pts',(0.,7.84754716719688,0.196222987756174));
#46003=CARTESIAN_POINT('Ctrl Pts',(0.,7.84754700261752,0.196229557926955));
#46004=CARTESIAN_POINT('Ctrl Pts',(0.,7.81119093568739,1.64757497093006));
#46005=CARTESIAN_POINT('Ctrl Pts',(0.,6.91726207951188,4.52195496702326));
#46006=CARTESIAN_POINT('Ctrl Pts',(0.,3.50105635341255,7.48472362789611));
#46007=CARTESIAN_POINT('Ctrl Pts',(0.,0.388966149966533,7.98723970769094));
#46008=CARTESIAN_POINT('Ctrl Pts',(0.,-3.03612128106794,7.49951927521533));
#46009=CARTESIAN_POINT('Ctrl Pts',(0.,-6.61228370454174,5.42169455429562));
#46010=CARTESIAN_POINT('Ctrl Pts',(0.,-8.54935002682948,-0.243194628709643));
#46011=CARTESIAN_POINT('Ctrl Pts',(0.,-6.22282678657551,-5.96725937739419));
#46012=CARTESIAN_POINT('Ctrl Pts',(0.,-1.04979849262017,-8.37822345583749));
#46013=CARTESIAN_POINT('Ctrl Pts',(0.,3.83069267091806,-7.27959812302174));
#46014=CARTESIAN_POINT('Ctrl Pts',(0.,6.98762248431915,-4.34431588657474));
#46015=CARTESIAN_POINT('Ctrl Pts',(0.,7.81270576723367,-1.58710355622244));
#46016=CARTESIAN_POINT('Ctrl Pts',(0.,7.84754700261759,-0.196229557926836));
#46017=CARTESIAN_POINT('Ctrl Pts',(1.5,7.04779698988764,-0.176231641202319));
#46018=CARTESIAN_POINT('Ctrl Pts',(1.5,7.04679841138751,-0.216096563028019));
#46019=CARTESIAN_POINT('Ctrl Pts',(1.5,7.02210915861748,-0.950460970728723));
#46020=CARTESIAN_POINT('Ctrl Pts',(1.5,6.73567311075118,-2.4431876756519));
#46021=CARTESIAN_POINT('Ctrl Pts',(1.5,6.00262529198976,-3.78210604931351));
#46022=CARTESIAN_POINT('Ctrl Pts',(1.5,5.26585512838814,-4.70378009980091));
#46023=CARTESIAN_POINT('Ctrl Pts',(1.5,4.81558620855694,-5.17668232873438));
#46024=CARTESIAN_POINT('Ctrl Pts',(1.50000000000001,4.30870466570876,-5.58661807788342));
#46025=CARTESIAN_POINT('Ctrl Pts',(1.5,3.97740575868414,-5.82285201212594));
#46026=CARTESIAN_POINT('Ctrl Pts',(1.5,3.11208933639409,-6.39613745229425));
#46027=CARTESIAN_POINT('Ctrl Pts',(1.5,1.33885201664721,-7.0889077154724));
#46028=CARTESIAN_POINT('Ctrl Pts',(1.5,-1.68411245569617,-7.09281159181233));
#46029=CARTESIAN_POINT('Ctrl Pts',(1.5,-4.62775288425511,-5.68940118968998));
#46030=CARTESIAN_POINT('Ctrl Pts',(1.5,-6.32134574348598,-3.41161455311364));
#46031=CARTESIAN_POINT('Ctrl Pts',(1.5,-7.16221072057386,-0.803465361099522));
#46032=CARTESIAN_POINT('Ctrl Pts',(1.5,-7.02869221054055,2.3863506274691));
#46033=CARTESIAN_POINT('Ctrl Pts',(1.5,-5.37642314477699,4.81506856485811));
#46034=CARTESIAN_POINT('Ctrl Pts',(1.5,-3.72631177636962,6.00861903758754));
#46035=CARTESIAN_POINT('Ctrl Pts',(1.5,-3.15225899889574,6.32066033764087));
#46036=CARTESIAN_POINT('Ctrl Pts',(1.5,-1.99143161293444,6.81376111970392));
#46037=CARTESIAN_POINT('Ctrl Pts',(1.5,0.487779908623596,7.37998777732575));
#46038=CARTESIAN_POINT('Ctrl Pts',(1.5,4.65659822313403,6.07462569563999));
#46039=CARTESIAN_POINT('Ctrl Pts',(1.5,6.69920345996918,2.86157096981349));
#46040=CARTESIAN_POINT('Ctrl Pts',(1.5,7.01651072249489,0.785791900119064));
#46041=CARTESIAN_POINT('Ctrl Pts',(1.5,7.04371625681567,0.339141322789337));
#46042=CARTESIAN_POINT('Ctrl Pts',(1.5,7.04779682531124,0.17623821136714));
#46043=CARTESIAN_POINT('Ctrl Pts',(1.45,6.99781266888479,-0.174979581345908));
#46044=CARTESIAN_POINT('Ctrl Pts',(1.45,6.99682147563086,-0.214557224352159));
#46045=CARTESIAN_POINT('Ctrl Pts',(1.45,6.97230420129675,-0.943733162635674));
#46046=CARTESIAN_POINT('Ctrl Pts',(1.45,6.68790467738006,-2.42585669145555));
#46047=CARTESIAN_POINT('Ctrl Pts',(1.45,5.96005079855331,-3.75528320175119));
#46048=CARTESIAN_POINT('Ctrl Pts',(1.45,5.22851006715451,-4.67042136148825));
#46049=CARTESIAN_POINT('Ctrl Pts',(1.45,4.78143238941665,-5.13996980373977));
#46050=CARTESIAN_POINT('Ctrl Pts',(1.45000000000001,4.27814675891659,-5.54699633461483));
#46051=CARTESIAN_POINT('Ctrl Pts',(1.45,3.94919749215172,-5.78155720403649));
#46052=CARTESIAN_POINT('Ctrl Pts',(1.45,3.09001661915318,-6.35076805597684));
#46053=CARTESIAN_POINT('Ctrl Pts',(1.45,1.32935731991496,-7.03863662198873));
#46054=CARTESIAN_POINT('Ctrl Pts',(1.45,-1.67216942797454,-7.04250475985423));
#46055=CARTESIAN_POINT('Ctrl Pts',(1.45,-4.59492940793848,-5.64905133658995));
#46056=CARTESIAN_POINT('Ctrl Pts',(1.45,-6.2765164025017,-3.387419573102));
#46057=CARTESIAN_POINT('Ctrl Pts',(1.45,-7.11141233623102,-0.797768988290111));
#46058=CARTESIAN_POINT('Ctrl Pts',(1.45,-6.97885055702535,2.36943805784273));
#46059=CARTESIAN_POINT('Ctrl Pts',(1.45,-5.33827403269554,4.7808924535148));
#46060=CARTESIAN_POINT('Ctrl Pts',(1.45,-3.69989160340351,5.96601615936688));
#46061=CARTESIAN_POINT('Ctrl Pts',(1.45,-3.12990393400893,6.27581629241273));
#46062=CARTESIAN_POINT('Ctrl Pts',(1.45,-1.97730629927358,6.76546702941564));
#46063=CARTESIAN_POINT('Ctrl Pts',(1.45,0.484310761962725,7.32762492052164));
#46064=CARTESIAN_POINT('Ctrl Pts',(1.45,4.62359284627412,6.03155923010541));
#46065=CARTESIAN_POINT('Ctrl Pts',(1.45,6.65165743453235,2.84126958716708));
#46066=CARTESIAN_POINT('Ctrl Pts',(1.45,6.96676461290019,0.780220626486363));
#46067=CARTESIAN_POINT('Ctrl Pts',(1.45,6.99374990469182,0.336735818412981));
#46068=CARTESIAN_POINT('Ctrl Pts',(1.45,6.99781250430828,0.174986151515265));
#46069=CARTESIAN_POINT('Ctrl Pts',(1.4,6.94782834788194,-0.173727521489497));
#46070=CARTESIAN_POINT('Ctrl Pts',(1.4,6.94682238413562,-0.213879722134646));
#46071=CARTESIAN_POINT('Ctrl Pts',(1.4,6.92253452269999,-0.935880701452195));
#46072=CARTESIAN_POINT('Ctrl Pts',(1.4,6.64011424361582,-2.40913955069607));
#46073=CARTESIAN_POINT('Ctrl Pts',(1.4,5.91748619336573,-3.7283597794975));
#46074=CARTESIAN_POINT('Ctrl Pts',(1.4,5.19116104062186,-4.63701500758754));
#46075=CARTESIAN_POINT('Ctrl Pts',(1.4,4.74728136227759,-5.10321492888003));
#46076=CARTESIAN_POINT('Ctrl Pts',(1.4,4.24758832208607,-5.50734849491544));
#46077=CARTESIAN_POINT('Ctrl Pts',(1.4,3.92098870849758,-5.74022965314134));
#46078=CARTESIAN_POINT('Ctrl Pts',(1.4,3.06794764178653,-6.30539534847945));
#46079=CARTESIAN_POINT('Ctrl Pts',(1.4,1.31986057164665,-6.98834485012048));
#46080=CARTESIAN_POINT('Ctrl Pts',(1.4,-1.66022325421088,-6.99220276121136));
#46081=CARTESIAN_POINT('Ctrl Pts',(1.4,-4.56211352938548,-5.60870006630621));
#46082=CARTESIAN_POINT('Ctrl Pts',(1.4,-6.23167836095184,-3.36322153640607));
#46083=CARTESIAN_POINT('Ctrl Pts',(1.4,-7.06062164022606,-0.792066687527311));
#46084=CARTESIAN_POINT('Ctrl Pts',(1.4,-6.92898721977216,2.35248988333773));
#46085=CARTESIAN_POINT('Ctrl Pts',(1.4,-5.30018025186195,4.74679632662372));
#46086=CARTESIAN_POINT('Ctrl Pts',(1.4,-3.67344868840864,5.9233788475635));
#46087=CARTESIAN_POINT('Ctrl Pts',(1.4,-3.10754468665178,6.2310221356181));
#46088=CARTESIAN_POINT('Ctrl Pts',(1.4,-1.96318596506224,6.71708128064611));
#46089=CARTESIAN_POINT('Ctrl Pts',(1.4,0.480870252832169,7.27533268572036));
#46090=CARTESIAN_POINT('Ctrl Pts',(1.4,4.59052892370703,5.98843660249075));
#46091=CARTESIAN_POINT('Ctrl Pts',(1.4,6.60421294758832,2.82099443701422));
#46092=CARTESIAN_POINT('Ctrl Pts',(1.4,6.9169695694088,0.774639474633935));
#46093=CARTESIAN_POINT('Ctrl Pts',(1.4,6.94381611987581,0.334338463253306));
#46094=CARTESIAN_POINT('Ctrl Pts',(1.4,6.94782818330531,0.17373409166339));
#46095=CARTESIAN_POINT('Ctrl Pts',(1.35,6.89784402687909,-0.172475461633086));
#46096=CARTESIAN_POINT('Ctrl Pts',(1.35,6.89684544837896,-0.212340383458786));
#46097=CARTESIAN_POINT('Ctrl Pts',(1.35,6.87272956537927,-0.929152893359146));
#46098=CARTESIAN_POINT('Ctrl Pts',(1.35,6.5923458102447,-2.39180856649973));
#46099=CARTESIAN_POINT('Ctrl Pts',(1.35,5.87491169992928,-3.70153693193518));
#46100=CARTESIAN_POINT('Ctrl Pts',(1.35,5.15381597938823,-4.60365626927488));
#46101=CARTESIAN_POINT('Ctrl Pts',(1.35,4.7131275431373,-5.06650240388542));
#46102=CARTESIAN_POINT('Ctrl Pts',(1.35,4.2170304152939,-5.46772675164685));
#46103=CARTESIAN_POINT('Ctrl Pts',(1.35,3.89278044196515,-5.69893484505189));
#46104=CARTESIAN_POINT('Ctrl Pts',(1.35,3.04587492454562,-6.26002595216204));
#46105=CARTESIAN_POINT('Ctrl Pts',(1.35,1.3103658749144,-6.93807375663681));
#46106=CARTESIAN_POINT('Ctrl Pts',(1.35,-1.64828022648925,-6.94189592925327));
#46107=CARTESIAN_POINT('Ctrl Pts',(1.35,-4.52929005306886,-5.56835021320618));
#46108=CARTESIAN_POINT('Ctrl Pts',(1.35,-6.18684901996756,-3.33902655639443));
#46109=CARTESIAN_POINT('Ctrl Pts',(1.35,-7.00982325588322,-0.7863703147179));
#46110=CARTESIAN_POINT('Ctrl Pts',(1.35,-6.87914556625695,2.33557731371137));
#46111=CARTESIAN_POINT('Ctrl Pts',(1.35,-5.2620311397805,4.71262021528042));
#46112=CARTESIAN_POINT('Ctrl Pts',(1.35,-3.64702851544254,5.88077596934284));
#46113=CARTESIAN_POINT('Ctrl Pts',(1.35,-3.08518962176498,6.18617809038997));
#46114=CARTESIAN_POINT('Ctrl Pts',(1.35,-1.94906065140137,6.66878719035783));
#46115=CARTESIAN_POINT('Ctrl Pts',(1.35,0.477401106171298,7.22296982891625));
#46116=CARTESIAN_POINT('Ctrl Pts',(1.35,4.55752354684712,5.94537013695617));
#46117=CARTESIAN_POINT('Ctrl Pts',(1.35,6.5566669221515,2.80069305436781));
#46118=CARTESIAN_POINT('Ctrl Pts',(1.35,6.86722345981409,0.769068201001234));
#46119=CARTESIAN_POINT('Ctrl Pts',(1.35,6.89384976775196,0.33193295887695));
#46120=CARTESIAN_POINT('Ctrl Pts',(1.35,6.89784386230235,0.172482031811515));
#46121=CARTESIAN_POINT('',(1.35,6.89784386230235,0.172482031811515));
#46122=CARTESIAN_POINT('',(1.5,7.0477969074555,0.176234926281131));
#46123=CARTESIAN_POINT('Ctrl Pts',(1.35,6.89784386230235,0.172482031811515));
#46124=CARTESIAN_POINT('Ctrl Pts',(1.4,6.94782818330531,0.17373409166339));
#46125=CARTESIAN_POINT('Ctrl Pts',(1.45,6.99781250430828,0.174986151515265));
#46126=CARTESIAN_POINT('Ctrl Pts',(1.5,7.04779682531124,0.17623821136714));
#46127=CARTESIAN_POINT('Ctrl Pts',(1.5,7.04779682531124,0.17623821136714));
#46128=CARTESIAN_POINT('Ctrl Pts',(1.5,7.04371625681567,0.339141322789337));
#46129=CARTESIAN_POINT('Ctrl Pts',(1.5,7.01651072249489,0.785791900119064));
#46130=CARTESIAN_POINT('Ctrl Pts',(1.5,6.69920345996918,2.86157096981349));
#46131=CARTESIAN_POINT('Ctrl Pts',(1.5,4.65659822313403,6.07462569563999));
#46132=CARTESIAN_POINT('Ctrl Pts',(1.5,0.487779908623596,7.37998777732575));
#46133=CARTESIAN_POINT('Ctrl Pts',(1.5,-1.99143161293444,6.81376111970392));
#46134=CARTESIAN_POINT('Ctrl Pts',(1.5,-3.15225899889574,6.32066033764087));
#46135=CARTESIAN_POINT('Ctrl Pts',(1.5,-3.72631177636962,6.00861903758754));
#46136=CARTESIAN_POINT('Ctrl Pts',(1.5,-5.37642314477699,4.81506856485811));
#46137=CARTESIAN_POINT('Ctrl Pts',(1.5,-7.02869221054055,2.3863506274691));
#46138=CARTESIAN_POINT('Ctrl Pts',(1.5,-7.16221072057386,-0.803465361099522));
#46139=CARTESIAN_POINT('Ctrl Pts',(1.5,-6.32134574348598,-3.41161455311364));
#46140=CARTESIAN_POINT('Ctrl Pts',(1.5,-4.62775288425511,-5.68940118968998));
#46141=CARTESIAN_POINT('Ctrl Pts',(1.5,-1.68411245569617,-7.09281159181233));
#46142=CARTESIAN_POINT('Ctrl Pts',(1.5,1.33885201664721,-7.0889077154724));
#46143=CARTESIAN_POINT('Ctrl Pts',(1.5,3.11208933639409,-6.39613745229425));
#46144=CARTESIAN_POINT('Ctrl Pts',(1.5,3.97740575868414,-5.82285201212594));
#46145=CARTESIAN_POINT('Ctrl Pts',(1.50000000000001,4.30870466570876,-5.58661807788342));
#46146=CARTESIAN_POINT('Ctrl Pts',(1.5,4.81558620855694,-5.17668232873438));
#46147=CARTESIAN_POINT('Ctrl Pts',(1.5,5.26585512838814,-4.70378009980091));
#46148=CARTESIAN_POINT('Ctrl Pts',(1.5,6.00262529198976,-3.78210604931351));
#46149=CARTESIAN_POINT('Ctrl Pts',(1.5,6.73567311075118,-2.4431876756519));
#46150=CARTESIAN_POINT('Ctrl Pts',(1.5,7.02210915861748,-0.950460970728723));
#46151=CARTESIAN_POINT('Ctrl Pts',(1.5,7.04679841138751,-0.216096563028019));
#46152=CARTESIAN_POINT('Ctrl Pts',(1.5,7.04779698988764,-0.176231641202319));
#46153=CARTESIAN_POINT('Ctrl Pts',(1.35,6.89784386229926,-0.172482031811152));
#46154=CARTESIAN_POINT('Ctrl Pts',(1.35,6.89684530116423,-0.212344759189508));
#46155=CARTESIAN_POINT('Ctrl Pts',(1.35,6.87272914904771,-0.929155065202924));
#46156=CARTESIAN_POINT('Ctrl Pts',(1.35,6.5923458102447,-2.39180856649973));
#46157=CARTESIAN_POINT('Ctrl Pts',(1.35,5.87491169992928,-3.70153693193518));
#46158=CARTESIAN_POINT('Ctrl Pts',(1.35,5.15381597938823,-4.60365626927488));
#46159=CARTESIAN_POINT('Ctrl Pts',(1.35,4.7131275431373,-5.06650240388542));
#46160=CARTESIAN_POINT('Ctrl Pts',(1.35,4.2170304152939,-5.46772675164685));
#46161=CARTESIAN_POINT('Ctrl Pts',(1.35,3.89278044196515,-5.69893484505189));
#46162=CARTESIAN_POINT('Ctrl Pts',(1.35,3.04587492454562,-6.26002595216204));
#46163=CARTESIAN_POINT('Ctrl Pts',(1.35,1.3103658749144,-6.93807375663681));
#46164=CARTESIAN_POINT('Ctrl Pts',(1.35,-1.64828022648925,-6.94189592925327));
#46165=CARTESIAN_POINT('Ctrl Pts',(1.35,-4.52929005306886,-5.56835021320618));
#46166=CARTESIAN_POINT('Ctrl Pts',(1.35,-6.18684901996756,-3.33902655639443));
#46167=CARTESIAN_POINT('Ctrl Pts',(1.35,-7.00982325588322,-0.7863703147179));
#46168=CARTESIAN_POINT('Ctrl Pts',(1.35,-6.87914556625695,2.33557731371137));
#46169=CARTESIAN_POINT('Ctrl Pts',(1.35,-5.2620311397805,4.71262021528042));
#46170=CARTESIAN_POINT('Ctrl Pts',(1.35,-3.64702851544254,5.88077596934284));
#46171=CARTESIAN_POINT('Ctrl Pts',(1.35,-3.08518962176498,6.18617809038997));
#46172=CARTESIAN_POINT('Ctrl Pts',(1.35,-1.94906065140137,6.66878719035783));
#46173=CARTESIAN_POINT('Ctrl Pts',(1.35,0.477401106171298,7.22296982891625));
#46174=CARTESIAN_POINT('Ctrl Pts',(1.35,4.55752354684712,5.94537013695617));
#46175=CARTESIAN_POINT('Ctrl Pts',(1.35,6.5566669221515,2.80069305436781));
#46176=CARTESIAN_POINT('Ctrl Pts',(1.35,6.86722345981409,0.769068201001234));
#46177=CARTESIAN_POINT('Ctrl Pts',(1.35,6.89384976775196,0.33193295887695));
#46178=CARTESIAN_POINT('Ctrl Pts',(1.35,6.89784386230235,0.172482031811515));
#46179=CARTESIAN_POINT('Ctrl Pts',(0.,6.89784386230235,-0.172482031811513));
#46180=CARTESIAN_POINT('Ctrl Pts',(1.5,6.89784386230235,-0.172482031811513));
#46181=CARTESIAN_POINT('Ctrl Pts',(0.,6.89724474811762,-0.196399670871248));
#46182=CARTESIAN_POINT('Ctrl Pts',(1.5,6.89724474811762,-0.196399670871248));
#46183=CARTESIAN_POINT('Ctrl Pts',(0.,6.89584032941428,-0.244218013275302));
#46184=CARTESIAN_POINT('Ctrl Pts',(1.5,6.89584032941428,-0.244218013275302));
#46185=CARTESIAN_POINT('Ctrl Pts',(0.,6.89311513035763,-0.315894719735146));
#46186=CARTESIAN_POINT('Ctrl Pts',(1.5,6.89311513035763,-0.315894719735146));
#46187=CARTESIAN_POINT('Ctrl Pts',(0.,6.88824437407485,-0.411362046113201));
#46188=CARTESIAN_POINT('Ctrl Pts',(1.5,6.88824437407485,-0.411362046113201));
#46189=CARTESIAN_POINT('Ctrl Pts',(0.,6.88009417679297,-0.530524716562061));
#46190=CARTESIAN_POINT('Ctrl Pts',(1.5,6.88009417679297,-0.530524716562061));
#46191=CARTESIAN_POINT('Ctrl Pts',(0.,6.86988291489663,-0.649509527440788));
#46192=CARTESIAN_POINT('Ctrl Pts',(1.5,6.86988291489663,-0.649509527440788));
#46193=CARTESIAN_POINT('Ctrl Pts',(0.,6.85761207960178,-0.768303743989707));
#46194=CARTESIAN_POINT('Ctrl Pts',(1.5,6.85761207960178,-0.768303743989707));
#46195=CARTESIAN_POINT('Ctrl Pts',(0.,6.84328425996545,-0.886886149588898));
#46196=CARTESIAN_POINT('Ctrl Pts',(1.5,6.84328425996545,-0.886886149588898));
#46197=CARTESIAN_POINT('Ctrl Pts',(0.,6.82690343688202,-1.00522492629022));
#46198=CARTESIAN_POINT('Ctrl Pts',(1.5,6.82690343688202,-1.00522492629022));
#46199=CARTESIAN_POINT('Ctrl Pts',(0.,6.80847475546732,-1.12328081074534));
#46200=CARTESIAN_POINT('Ctrl Pts',(1.5,6.80847475546732,-1.12328081074534));
#46201=CARTESIAN_POINT('Ctrl Pts',(0.,6.78800429750229,-1.24101024985217));
#46202=CARTESIAN_POINT('Ctrl Pts',(1.5,6.78800429750229,-1.24101024985217));
#46203=CARTESIAN_POINT('Ctrl Pts',(0.,6.76549885392698,-1.35836855624314));
#46204=CARTESIAN_POINT('Ctrl Pts',(1.5,6.76549885392698,-1.35836855624314));
#46205=CARTESIAN_POINT('Ctrl Pts',(0.,6.7409656973767,-1.47531306373193));
#46206=CARTESIAN_POINT('Ctrl Pts',(1.5,6.7409656973767,-1.47531306373193));
#46207=CARTESIAN_POINT('Ctrl Pts',(0.,6.71441235475108,-1.59180628284158));
#46208=CARTESIAN_POINT('Ctrl Pts',(1.5,6.71441235475108,-1.59180628284158));
#46209=CARTESIAN_POINT('Ctrl Pts',(0.,6.68584670609465,-1.70781446091543));
#46210=CARTESIAN_POINT('Ctrl Pts',(1.5,6.68584670609465,-1.70781446091543));
#46211=CARTESIAN_POINT('Ctrl Pts',(0.,6.65527708350519,-1.82330614237454));
#46212=CARTESIAN_POINT('Ctrl Pts',(1.5,6.65527708350519,-1.82330614237454));
#46213=CARTESIAN_POINT('Ctrl Pts',(0.,6.62271237007447,-1.93825072906442));
#46214=CARTESIAN_POINT('Ctrl Pts',(1.5,6.62271237007447,-1.93825072906442));
#46215=CARTESIAN_POINT('Ctrl Pts',(0.,6.58816209886438,-2.05261704063842));
#46216=CARTESIAN_POINT('Ctrl Pts',(1.5,6.58816209886438,-2.05261704063842));
#46217=CARTESIAN_POINT('Ctrl Pts',(0.,6.55163655192257,-2.16637187492234));
#46218=CARTESIAN_POINT('Ctrl Pts',(1.5,6.55163655192257,-2.16637187492234));
#46219=CARTESIAN_POINT('Ctrl Pts',(0.,6.5131467128519,-2.2794806466461));
#46220=CARTESIAN_POINT('Ctrl Pts',(1.5,6.5131467128519,-2.2794806466461));
#46221=CARTESIAN_POINT('Ctrl Pts',(0.,6.47270421942094,-2.39190802612683));
#46222=CARTESIAN_POINT('Ctrl Pts',(1.5,6.47270421942094,-2.39190802612683));
#46223=CARTESIAN_POINT('Ctrl Pts',(0.,6.43032131621383,-2.50361857792922));
#46224=CARTESIAN_POINT('Ctrl Pts',(1.5,6.43032131621383,-2.50361857792922));
#46225=CARTESIAN_POINT('Ctrl Pts',(0.,6.38601080731761,-2.61457739952654));
#46226=CARTESIAN_POINT('Ctrl Pts',(1.5,6.38601080731761,-2.61457739952654));
#46227=CARTESIAN_POINT('Ctrl Pts',(0.,6.33978600904486,-2.72475075998758));
#46228=CARTESIAN_POINT('Ctrl Pts',(1.5,6.33978600904486,-2.72475075998758));
#46229=CARTESIAN_POINT('Ctrl Pts',(0.,6.29166076444393,-2.83410583895234));
#46230=CARTESIAN_POINT('Ctrl Pts',(1.5,6.29166076444393,-2.83410583895234));
#46231=CARTESIAN_POINT('Ctrl Pts',(0.,6.24164945784327,-2.94261046564831));
#46232=CARTESIAN_POINT('Ctrl Pts',(1.5,6.24164945784327,-2.94261046564831));
#46233=CARTESIAN_POINT('Ctrl Pts',(0.,6.18976702943031,-3.05023285793724));
#46234=CARTESIAN_POINT('Ctrl Pts',(1.5,6.18976702943031,-3.05023285793724));
#46235=CARTESIAN_POINT('Ctrl Pts',(0.,6.13602898986516,-3.15694136138263));
#46236=CARTESIAN_POINT('Ctrl Pts',(1.5,6.13602898986516,-3.15694136138263));
#46237=CARTESIAN_POINT('Ctrl Pts',(0.,6.0804514349299,-3.26270418832876));
#46238=CARTESIAN_POINT('Ctrl Pts',(1.5,6.0804514349299,-3.26270418832876));
#46239=CARTESIAN_POINT('Ctrl Pts',(0.,6.02305103215795,-3.3674895439004));
#46240=CARTESIAN_POINT('Ctrl Pts',(1.5,6.02305103215795,-3.3674895439004));
#46241=CARTESIAN_POINT('Ctrl Pts',(0.,5.96384500749886,-3.47126575200923));
#46242=CARTESIAN_POINT('Ctrl Pts',(1.5,5.96384500749886,-3.47126575200923));
#46243=CARTESIAN_POINT('Ctrl Pts',(0.,5.90285113201764,-3.57400138137212));
#46244=CARTESIAN_POINT('Ctrl Pts',(1.5,5.90285113201764,-3.57400138137212));
#46245=CARTESIAN_POINT('Ctrl Pts',(0.,5.84008770862799,-3.67566537154608));
#46246=CARTESIAN_POINT('Ctrl Pts',(1.5,5.84008770862799,-3.67566537154608));
#46247=CARTESIAN_POINT('Ctrl Pts',(0.,5.77557355885907,-3.77622715898496));
#46248=CARTESIAN_POINT('Ctrl Pts',(1.5,5.77557355885907,-3.77622715898496));
#46249=CARTESIAN_POINT('Ctrl Pts',(0.,5.70932802034008,-3.87565663572559));
#46250=CARTESIAN_POINT('Ctrl Pts',(1.5,5.70932802034008,-3.87565663572559));
#46251=CARTESIAN_POINT('Ctrl Pts',(0.,5.6413709443175,-3.97392410809942));
#46252=CARTESIAN_POINT('Ctrl Pts',(1.5,5.6413709443175,-3.97392410809942));
#46253=CARTESIAN_POINT('Ctrl Pts',(0.,5.5717226932043,-4.071000255468));
#46254=CARTESIAN_POINT('Ctrl Pts',(1.5,5.5717226932043,-4.071000255468));
#46255=CARTESIAN_POINT('Ctrl Pts',(0.,5.5004041381615,-4.16685608898142));
#46256=CARTESIAN_POINT('Ctrl Pts',(1.5,5.5004041381615,-4.16685608898142));
#46257=CARTESIAN_POINT('Ctrl Pts',(0.,5.42743665671107,-4.26146291035777));
#46258=CARTESIAN_POINT('Ctrl Pts',(1.5,5.42743665671107,-4.26146291035777));
#46259=CARTESIAN_POINT('Ctrl Pts',(0.,5.35284212445925,-4.35479234184529));
#46260=CARTESIAN_POINT('Ctrl Pts',(1.5,5.35284212445925,-4.35479234184529));
#46261=CARTESIAN_POINT('Ctrl Pts',(0.,5.27664290685087,-4.44681635620583));
#46262=CARTESIAN_POINT('Ctrl Pts',(1.5,5.27664290685087,-4.44681635620583));
#46263=CARTESIAN_POINT('Ctrl Pts',(0.,5.19886185095403,-4.53750730672115));
#46264=CARTESIAN_POINT('Ctrl Pts',(1.5,5.19886185095403,-4.53750730672115));
#46265=CARTESIAN_POINT('Ctrl Pts',(0.,5.11952227727487,-4.62683795722317));
#46266=CARTESIAN_POINT('Ctrl Pts',(1.5,5.11952227727487,-4.62683795722317));
#46267=CARTESIAN_POINT('Ctrl Pts',(0.,5.03864797160198,-4.71478151214955));
#46268=CARTESIAN_POINT('Ctrl Pts',(1.5,5.03864797160198,-4.71478151214955));
#46269=CARTESIAN_POINT('Ctrl Pts',(0.,4.95626317819267,-4.80131161496185));
#46270=CARTESIAN_POINT('Ctrl Pts',(1.5,4.95626317819267,-4.80131161496185));
#46271=CARTESIAN_POINT('Ctrl Pts',(0.,4.87239259298808,-4.88640234659096));
#46272=CARTESIAN_POINT('Ctrl Pts',(1.5,4.87239259298808,-4.88640234659096));
#46273=CARTESIAN_POINT('Ctrl Pts',(0.,4.78706135685639,-4.97002822390911));
#46274=CARTESIAN_POINT('Ctrl Pts',(1.5,4.78706135685639,-4.97002822390911));
#46275=CARTESIAN_POINT('Ctrl Pts',(0.,4.70029504886414,-5.05216419822937));
#46276=CARTESIAN_POINT('Ctrl Pts',(1.5,4.70029504886414,-5.05216419822937));
#46277=CARTESIAN_POINT('Ctrl Pts',(0.,4.61211967957449,-5.13278565383202));
#46278=CARTESIAN_POINT('Ctrl Pts',(1.5,4.61211967957449,-5.13278565383202));
#46279=CARTESIAN_POINT('Ctrl Pts',(0.,4.52256168266376,-5.21186841902494));
#46280=CARTESIAN_POINT('Ctrl Pts',(1.5,4.52256168266376,-5.21186841902494));
#46281=CARTESIAN_POINT('Ctrl Pts',(0.,4.43164790656435,-5.28938877723193));
#46282=CARTESIAN_POINT('Ctrl Pts',(1.5,4.43164790656435,-5.28938877723193));
#46283=CARTESIAN_POINT('Ctrl Pts',(0.,4.33940560613361,-5.36532347810974));
#46284=CARTESIAN_POINT('Ctrl Pts',(1.5,4.33940560613361,-5.36532347810974));
#46285=CARTESIAN_POINT('Ctrl Pts',(0.,4.24586243434812,-5.43964974869403));
#46286=CARTESIAN_POINT('Ctrl Pts',(1.5,4.24586243434812,-5.43964974869403));
#46287=CARTESIAN_POINT('Ctrl Pts',(0.,4.1510464340228,-5.51234530457529));
#46288=CARTESIAN_POINT('Ctrl Pts',(1.5,4.1510464340228,-5.51234530457529));
#46289=CARTESIAN_POINT('Ctrl Pts',(0.,4.05498602924829,-5.58338835449849));
#46290=CARTESIAN_POINT('Ctrl Pts',(1.5,4.05498602924829,-5.58338835449849));
#46291=CARTESIAN_POINT('Ctrl Pts',(0.,3.95771001685222,-5.65275760499342));
#46292=CARTESIAN_POINT('Ctrl Pts',(1.5,3.95771001685222,-5.65275760499342));
#46293=CARTESIAN_POINT('Ctrl Pts',(0.,3.85924755788366,-5.72043226503622));
#46294=CARTESIAN_POINT('Ctrl Pts',(1.5,3.85924755788366,-5.72043226503622));
#46295=CARTESIAN_POINT('Ctrl Pts',(0.,3.75962816912048,-5.7863920507423));
#46296=CARTESIAN_POINT('Ctrl Pts',(1.5,3.75962816912048,-5.7863920507423));
#46297=CARTESIAN_POINT('Ctrl Pts',(0.,3.65888171459871,-5.85061719009085));
#46298=CARTESIAN_POINT('Ctrl Pts',(1.5,3.65888171459871,-5.85061719009085));
#46299=CARTESIAN_POINT('Ctrl Pts',(0.,3.55703839636322,-5.91308842921879));
#46300=CARTESIAN_POINT('Ctrl Pts',(1.5,3.55703839636322,-5.91308842921879));
#46301=CARTESIAN_POINT('Ctrl Pts',(0.,3.45412874523946,-5.97378703874717));
#46302=CARTESIAN_POINT('Ctrl Pts',(1.5,3.45412874523946,-5.97378703874717));
#46303=CARTESIAN_POINT('Ctrl Pts',(0.,3.35018361162571,-6.03269482014034));
#46304=CARTESIAN_POINT('Ctrl Pts',(1.5,3.35018361162571,-6.03269482014034));
#46305=CARTESIAN_POINT('Ctrl Pts',(0.,3.2452341563054,-6.08979411209817));
#46306=CARTESIAN_POINT('Ctrl Pts',(1.5,3.2452341563054,-6.08979411209817));
#46307=CARTESIAN_POINT('Ctrl Pts',(0.,3.13931184127879,-6.14506779698192));
#46308=CARTESIAN_POINT('Ctrl Pts',(1.5,3.13931184127879,-6.14506779698192));
#46309=CARTESIAN_POINT('Ctrl Pts',(0.,3.03244842014227,-6.1984993052291));
#46310=CARTESIAN_POINT('Ctrl Pts',(1.5,3.03244842014227,-6.1984993052291));
#46311=CARTESIAN_POINT('Ctrl Pts',(0.,2.92467592848598,-6.25007261980265));
#46312=CARTESIAN_POINT('Ctrl Pts',(1.5,2.92467592848598,-6.25007261980265));
#46313=CARTESIAN_POINT('Ctrl Pts',(0.,2.81602667430891,-6.29977228067469));
#46314=CARTESIAN_POINT('Ctrl Pts',(1.5,2.81602667430891,-6.29977228067469));
#46315=CARTESIAN_POINT('Ctrl Pts',(0.,2.70653322845114,-6.34758338934502));
#46316=CARTESIAN_POINT('Ctrl Pts',(1.5,2.70653322845114,-6.34758338934502));
#46317=CARTESIAN_POINT('Ctrl Pts',(0.,2.59622841504235,-6.39349161339477));
#46318=CARTESIAN_POINT('Ctrl Pts',(1.5,2.59622841504235,-6.39349161339477));
#46319=CARTESIAN_POINT('Ctrl Pts',(0.,2.48514530147603,-6.43748319050759));
#46320=CARTESIAN_POINT('Ctrl Pts',(1.5,2.48514530147603,-6.43748319050759));
#46321=CARTESIAN_POINT('Ctrl Pts',(0.,2.37331718839874,-6.47954493252637));
#46322=CARTESIAN_POINT('Ctrl Pts',(1.5,2.37331718839874,-6.47954493252637));
#46323=CARTESIAN_POINT('Ctrl Pts',(0.,2.26077759971398,-6.51966422954569));
#46324=CARTESIAN_POINT('Ctrl Pts',(1.5,2.26077759971398,-6.51966422954569));
#46325=CARTESIAN_POINT('Ctrl Pts',(0.,2.14756027260008,-6.55782905404073));
#46326=CARTESIAN_POINT('Ctrl Pts',(1.5,2.14756027260008,-6.55782905404073));
#46327=CARTESIAN_POINT('Ctrl Pts',(0.,2.03369914754128,-6.5940279650321));
#46328=CARTESIAN_POINT('Ctrl Pts',(1.5,2.03369914754128,-6.5940279650321));
#46329=CARTESIAN_POINT('Ctrl Pts',(0.,1.91922835801735,-6.6282501110295));
#46330=CARTESIAN_POINT('Ctrl Pts',(1.5,1.91922835801735,-6.6282501110295));
#46331=CARTESIAN_POINT('Ctrl Pts',(0.,1.8041822202052,-6.6604852330121));
#46332=CARTESIAN_POINT('Ctrl Pts',(1.5,1.8041822202052,-6.6604852330121));
#46333=CARTESIAN_POINT('Ctrl Pts',(0.,1.68859522269198,-6.69072366744589));
#46334=CARTESIAN_POINT('Ctrl Pts',(1.5,1.68859522269198,-6.69072366744589));
#46335=CARTESIAN_POINT('Ctrl Pts',(0.,1.57250201619896,-6.71895634933824));
#46336=CARTESIAN_POINT('Ctrl Pts',(1.5,1.57250201619896,-6.71895634933824));
#46337=CARTESIAN_POINT('Ctrl Pts',(0.,1.45593740331553,-6.74517481532982));
#46338=CARTESIAN_POINT('Ctrl Pts',(1.5,1.45593740331553,-6.74517481532982));
#46339=CARTESIAN_POINT('Ctrl Pts',(0.,1.33893632796183,-6.76937120581976));
#46340=CARTESIAN_POINT('Ctrl Pts',(1.5,1.33893632796183,-6.76937120581976));
#46341=CARTESIAN_POINT('Ctrl Pts',(0.,1.22153386486024,-6.79153826712829));
#46342=CARTESIAN_POINT('Ctrl Pts',(1.5,1.22153386486024,-6.79153826712829));
#46343=CARTESIAN_POINT('Ctrl Pts',(0.,1.10376520901503,-6.81166935369773));
#46344=CARTESIAN_POINT('Ctrl Pts',(1.5,1.10376520901503,-6.81166935369773));
#46345=CARTESIAN_POINT('Ctrl Pts',(0.,0.985665665199513,-6.82975843033136));
#46346=CARTESIAN_POINT('Ctrl Pts',(1.5,0.985665665199513,-6.82975843033136));
#46347=CARTESIAN_POINT('Ctrl Pts',(0.,0.867270637450104,-6.84580007447043));
#46348=CARTESIAN_POINT('Ctrl Pts',(1.5,0.867270637450104,-6.84580007447043));
#46349=CARTESIAN_POINT('Ctrl Pts',(0.,0.748615618389539,-6.85978947736425));
#46350=CARTESIAN_POINT('Ctrl Pts',(1.5,0.748615618389539,-6.85978947736425));
#46351=CARTESIAN_POINT('Ctrl Pts',(0.,0.629736178555588,-6.87172244527821));
#46352=CARTESIAN_POINT('Ctrl Pts',(1.5,0.629736178555588,-6.87172244527821));
#46353=CARTESIAN_POINT('Ctrl Pts',(0.,0.510667955734564,-6.8815954007406));
#46354=CARTESIAN_POINT('Ctrl Pts',(1.5,0.510667955734564,-6.8815954007406));
#46355=CARTESIAN_POINT('Ctrl Pts',(0.,0.391446644298975,-6.88940538382764));
#46356=CARTESIAN_POINT('Ctrl Pts',(1.5,0.391446644298975,-6.88940538382764));
#46357=CARTESIAN_POINT('Ctrl Pts',(0.,0.272107984548754,-6.8951500534872));
#46358=CARTESIAN_POINT('Ctrl Pts',(1.5,0.272107984548754,-6.8951500534872));
#46359=CARTESIAN_POINT('Ctrl Pts',(0.,0.152687751971164,-6.89882768779677));
#46360=CARTESIAN_POINT('Ctrl Pts',(1.5,0.152687751971164,-6.89882768779677));
#46361=CARTESIAN_POINT('Ctrl Pts',(0.,0.0332217465029873,-6.90043718426009));
#46362=CARTESIAN_POINT('Ctrl Pts',(1.5,0.0332217465029873,-6.90043718426009));
#46363=CARTESIAN_POINT('Ctrl Pts',(0.,-0.0862542182058646,-6.89997806014264));
#46364=CARTESIAN_POINT('Ctrl Pts',(1.5,-0.0862542182058646,-6.89997806014264));
#46365=CARTESIAN_POINT('Ctrl Pts',(0.,-0.205704325527785,-6.8974504528457));
#46366=CARTESIAN_POINT('Ctrl Pts',(1.5,-0.205704325527785,-6.8974504528457));
#46367=CARTESIAN_POINT('Ctrl Pts',(0.,-0.325092766592762,-6.89285512031913));
#46368=CARTESIAN_POINT('Ctrl Pts',(1.5,-0.325092766592762,-6.89285512031913));
#46369=CARTESIAN_POINT('Ctrl Pts',(0.,-0.444383751009717,-6.88619344038296));
#46370=CARTESIAN_POINT('Ctrl Pts',(1.5,-0.444383751009717,-6.88619344038296));
#46371=CARTESIAN_POINT('Ctrl Pts',(0.,-0.563541517589008,-6.87746741008788));
#46372=CARTESIAN_POINT('Ctrl Pts',(1.5,-0.563541517589008,-6.87746741008788));
#46373=CARTESIAN_POINT('Ctrl Pts',(0.,-0.682530345066741,-6.86667964511437));
#46374=CARTESIAN_POINT('Ctrl Pts',(1.5,-0.682530345066741,-6.86667964511437));
#46375=CARTESIAN_POINT('Ctrl Pts',(0.,-0.801314562831502,-6.85383337921045));
#46376=CARTESIAN_POINT('Ctrl Pts',(1.5,-0.801314562831502,-6.85383337921045));
#46377=CARTESIAN_POINT('Ctrl Pts',(0.,-0.919858561654232,-6.83893246366781));
#46378=CARTESIAN_POINT('Ctrl Pts',(1.5,-0.919858561654232,-6.83893246366781));
#46379=CARTESIAN_POINT('Ctrl Pts',(0.,-1.03812680431107,-6.82198136572201));
#46380=CARTESIAN_POINT('Ctrl Pts',(1.5,-1.03812680431107,-6.82198136572201));
#46381=CARTESIAN_POINT('Ctrl Pts',(0.,-1.15608383621068,-6.80298516699082));
#46382=CARTESIAN_POINT('Ctrl Pts',(1.5,-1.15608383621068,-6.80298516699082));
#46383=CARTESIAN_POINT('Ctrl Pts',(0.,-1.27369429602679,-6.78194956195138));
#46384=CARTESIAN_POINT('Ctrl Pts',(1.5,-1.27369429602679,-6.78194956195138));
#46385=CARTESIAN_POINT('Ctrl Pts',(0.,-1.39092292633656,-6.7588808564554));
#46386=CARTESIAN_POINT('Ctrl Pts',(1.5,-1.39092292633656,-6.7588808564554));
#46387=CARTESIAN_POINT('Ctrl Pts',(0.,-1.50773458426541,-6.73378596628269));
#46388=CARTESIAN_POINT('Ctrl Pts',(1.5,-1.50773458426541,-6.73378596628269));
#46389=CARTESIAN_POINT('Ctrl Pts',(0.,-1.62409425193172,-6.70667241462751));
#46390=CARTESIAN_POINT('Ctrl Pts',(1.5,-1.62409425193172,-6.70667241462751));
#46391=CARTESIAN_POINT('Ctrl Pts',(0.,-1.7399670468992,-6.67754832962271));
#46392=CARTESIAN_POINT('Ctrl Pts',(1.5,-1.7399670468992,-6.67754832962271));
#46393=CARTESIAN_POINT('Ctrl Pts',(0.,-1.85531823263776,-6.64642244190193));
#46394=CARTESIAN_POINT('Ctrl Pts',(1.5,-1.85531823263776,-6.64642244190193));
#46395=CARTESIAN_POINT('Ctrl Pts',(0.,-1.97011322899335,-6.61330408219923));
#46396=CARTESIAN_POINT('Ctrl Pts',(1.5,-1.97011322899335,-6.61330408219923));
#46397=CARTESIAN_POINT('Ctrl Pts',(0.,-2.08431762266778,-6.57820317898646));
#46398=CARTESIAN_POINT('Ctrl Pts',(1.5,-2.08431762266778,-6.57820317898646));
#46399=CARTESIAN_POINT('Ctrl Pts',(0.,-2.19789717740688,-6.54113025506627));
#46400=CARTESIAN_POINT('Ctrl Pts',(1.5,-2.19789717740688,-6.54113025506627));
#46401=CARTESIAN_POINT('Ctrl Pts',(0.,-2.31081784419971,-6.5020964242025));
#46402=CARTESIAN_POINT('Ctrl Pts',(1.5,-2.31081784419971,-6.5020964242025));
#46403=CARTESIAN_POINT('Ctrl Pts',(0.,-2.42304577148957,-6.4611133877874));
#46404=CARTESIAN_POINT('Ctrl Pts',(1.5,-2.42304577148957,-6.4611133877874));
#46405=CARTESIAN_POINT('Ctrl Pts',(0.,-2.53454731539729,-6.41819343154569));
#46406=CARTESIAN_POINT('Ctrl Pts',(1.5,-2.53454731539729,-6.41819343154569));
#46407=CARTESIAN_POINT('Ctrl Pts',(0.,-2.64528904995755,-6.37334942227507));
#46408=CARTESIAN_POINT('Ctrl Pts',(1.5,-2.64528904995755,-6.37334942227507));
#46409=CARTESIAN_POINT('Ctrl Pts',(0.,-2.75523777697425,-6.32659480357096));
#46410=CARTESIAN_POINT('Ctrl Pts',(1.5,-2.75523777697425,-6.32659480357096));
#46411=CARTESIAN_POINT('Ctrl Pts',(0.,-2.86436053589027,-6.27794359158745));
#46412=CARTESIAN_POINT('Ctrl Pts',(1.5,-2.86436053589027,-6.27794359158745));
#46413=CARTESIAN_POINT('Ctrl Pts',(0.,-2.97262461367192,-6.22741037083388));
#46414=CARTESIAN_POINT('Ctrl Pts',(1.5,-2.97262461367192,-6.22741037083388));
#46415=CARTESIAN_POINT('Ctrl Pts',(0.,-3.07999755470908,-6.17501029000702));
#46416=CARTESIAN_POINT('Ctrl Pts',(1.5,-3.07999755470908,-6.17501029000702));
#46417=CARTESIAN_POINT('Ctrl Pts',(0.,-3.18644717073111,-6.12075905785837));
#46418=CARTESIAN_POINT('Ctrl Pts',(1.5,-3.18644717073111,-6.12075905785837));
#46419=CARTESIAN_POINT('Ctrl Pts',(0.,-3.29194155025575,-6.06467293808302));
#46420=CARTESIAN_POINT('Ctrl Pts',(1.5,-3.29194155025575,-6.06467293808302));
#46421=CARTESIAN_POINT('Ctrl Pts',(0.,-3.39644906805528,-6.00676874424304));
#46422=CARTESIAN_POINT('Ctrl Pts',(1.5,-3.39644906805528,-6.00676874424304));
#46423=CARTESIAN_POINT('Ctrl Pts',(0.,-3.49993839464067,-5.94706383472536));
#46424=CARTESIAN_POINT('Ctrl Pts',(1.5,-3.49993839464067,-5.94706383472536));
#46425=CARTESIAN_POINT('Ctrl Pts',(0.,-3.60237850576418,-5.88557610773356));
#46426=CARTESIAN_POINT('Ctrl Pts',(1.5,-3.60237850576418,-5.88557610773356));
#46427=CARTESIAN_POINT('Ctrl Pts',(0.,-3.70373869194093,-5.82232399631353));
#46428=CARTESIAN_POINT('Ctrl Pts',(1.5,-3.70373869194093,-5.82232399631353));
#46429=CARTESIAN_POINT('Ctrl Pts',(0.,-3.80398856742054,-5.75732646244435));
#46430=CARTESIAN_POINT('Ctrl Pts',(1.5,-3.80398856742054,-5.75732646244435));
#46431=CARTESIAN_POINT('Ctrl Pts',(0.,-3.90309807917881,-5.69060299116233));
#46432=CARTESIAN_POINT('Ctrl Pts',(1.5,-3.90309807917881,-5.69060299116233));
#46433=CARTESIAN_POINT('Ctrl Pts',(0.,-4.00103751593049,-5.62217358471744));
#46434=CARTESIAN_POINT('Ctrl Pts',(1.5,-4.00103751593049,-5.62217358471744));
#46435=CARTESIAN_POINT('Ctrl Pts',(0.,-4.09777751716309,-5.55205875676251));
#46436=CARTESIAN_POINT('Ctrl Pts',(1.5,-4.09777751716309,-5.55205875676251));
#46437=CARTESIAN_POINT('Ctrl Pts',(0.,-4.19328908219274,-5.48027952657387));
#46438=CARTESIAN_POINT('Ctrl Pts',(1.5,-4.19328908219274,-5.48027952657387));
#46439=CARTESIAN_POINT('Ctrl Pts',(0.,-4.28754357859123,-5.4068574123888));
#46440=CARTESIAN_POINT('Ctrl Pts',(1.5,-4.28754357859123,-5.4068574123888));
#46441=CARTESIAN_POINT('Ctrl Pts',(0.,-4.38051275063608,-5.33181442477391));
#46442=CARTESIAN_POINT('Ctrl Pts',(1.5,-4.38051275063608,-5.33181442477391));
#46443=CARTESIAN_POINT('Ctrl Pts',(0.,-4.47216872778419,-5.25517306002452));
#46444=CARTESIAN_POINT('Ctrl Pts',(1.5,-4.47216872778419,-5.25517306002452));
#46445=CARTESIAN_POINT('Ctrl Pts',(0.,-4.56248403316946,-5.17695629359431));
#46446=CARTESIAN_POINT('Ctrl Pts',(1.5,-4.56248403316946,-5.17695629359431));
#46447=CARTESIAN_POINT('Ctrl Pts',(0.,-4.65143159212514,-5.09718757355493));
#46448=CARTESIAN_POINT('Ctrl Pts',(1.5,-4.65143159212514,-5.09718757355493));
#46449=CARTESIAN_POINT('Ctrl Pts',(0.,-4.7389847400031,-5.01589081322949));
#46450=CARTESIAN_POINT('Ctrl Pts',(1.5,-4.7389847400031,-5.01589081322949));
#46451=CARTESIAN_POINT('Ctrl Pts',(0.,-4.82511723001895,-4.93309038385534));
#46452=CARTESIAN_POINT('Ctrl Pts',(1.5,-4.82511723001895,-4.93309038385534));
#46453=CARTESIAN_POINT('Ctrl Pts',(0.,-4.9098032411231,-4.84881110727519));
#46454=CARTESIAN_POINT('Ctrl Pts',(1.5,-4.9098032411231,-4.84881110727519));
#46455=CARTESIAN_POINT('Ctrl Pts',(0.,-4.99301738589862,-4.76307824865675));
#46456=CARTESIAN_POINT('Ctrl Pts',(1.5,-4.99301738589862,-4.76307824865675));
#46457=CARTESIAN_POINT('Ctrl Pts',(0.,-5.07473471848603,-4.67591750924002));
#46458=CARTESIAN_POINT('Ctrl Pts',(1.5,-5.07473471848603,-4.67591750924002));
#46459=CARTESIAN_POINT('Ctrl Pts',(0.,-5.1549307417364,-4.5873550183222));
#46460=CARTESIAN_POINT('Ctrl Pts',(1.5,-5.1549307417364,-4.5873550183222));
#46461=CARTESIAN_POINT('Ctrl Pts',(0.,-5.23358141439273,-4.49741732526974));
#46462=CARTESIAN_POINT('Ctrl Pts',(1.5,-5.23358141439273,-4.49741732526974));
#46463=CARTESIAN_POINT('Ctrl Pts',(0.,-5.31066315829954,-4.40613139155633));
#46464=CARTESIAN_POINT('Ctrl Pts',(1.5,-5.31066315829954,-4.40613139155633));
#46465=CARTESIAN_POINT('Ctrl Pts',(0.,-5.38615286564164,-4.31352458282688));
#46466=CARTESIAN_POINT('Ctrl Pts',(1.5,-5.38615286564164,-4.31352458282688));
#46467=CARTESIAN_POINT('Ctrl Pts',(0.,-5.46002790621214,-4.21962466098661));
#46468=CARTESIAN_POINT('Ctrl Pts',(1.5,-5.46002790621214,-4.21962466098661));
#46469=CARTESIAN_POINT('Ctrl Pts',(0.,-5.53226613384586,-4.12445977559767));
#46470=CARTESIAN_POINT('Ctrl Pts',(1.5,-5.53226613384586,-4.12445977559767));
#46471=CARTESIAN_POINT('Ctrl Pts',(0.,-5.60284589288301,-4.02805845530006));
#46472=CARTESIAN_POINT('Ctrl Pts',(1.5,-5.60284589288301,-4.02805845530006));
#46473=CARTESIAN_POINT('Ctrl Pts',(0.,-5.67174602466349,-3.93044959925604));
#46474=CARTESIAN_POINT('Ctrl Pts',(1.5,-5.67174602466349,-3.93044959925604));
#46475=CARTESIAN_POINT('Ctrl Pts',(0.,-5.73894587405215,-3.8316624686178));
#46476=CARTESIAN_POINT('Ctrl Pts',(1.5,-5.73894587405215,-3.8316624686178));
#46477=CARTESIAN_POINT('Ctrl Pts',(0.,-5.80442529599575,-3.731726678018));
#46478=CARTESIAN_POINT('Ctrl Pts',(1.5,-5.80442529599575,-3.731726678018));
#46479=CARTESIAN_POINT('Ctrl Pts',(0.,-5.86816466118834,-3.63067218644238));
#46480=CARTESIAN_POINT('Ctrl Pts',(1.5,-5.86816466118834,-3.63067218644238));
#46481=CARTESIAN_POINT('Ctrl Pts',(0.,-5.93014486176895,-3.52852928812396));
#46482=CARTESIAN_POINT('Ctrl Pts',(1.5,-5.93014486176895,-3.52852928812396));
#46483=CARTESIAN_POINT('Ctrl Pts',(0.,-5.99034731705189,-3.42532860345791));
#46484=CARTESIAN_POINT('Ctrl Pts',(1.5,-5.99034731705189,-3.42532860345791));
#46485=CARTESIAN_POINT('Ctrl Pts',(0.,-6.04875397928989,-3.32110106993708));
#46486=CARTESIAN_POINT('Ctrl Pts',(1.5,-6.04875397928989,-3.32110106993708));
#46487=CARTESIAN_POINT('Ctrl Pts',(0.,-6.10534733947052,-3.2158779331071));
#46488=CARTESIAN_POINT('Ctrl Pts',(1.5,-6.10534733947052,-3.2158779331071));
#46489=CARTESIAN_POINT('Ctrl Pts',(0.,-6.16011043217119,-3.10969073698348));
#46490=CARTESIAN_POINT('Ctrl Pts',(1.5,-6.16011043217119,-3.10969073698348));
#46491=CARTESIAN_POINT('Ctrl Pts',(0.,-6.21302684044837,-3.00257131448723));
#46492=CARTESIAN_POINT('Ctrl Pts',(1.5,-6.21302684044837,-3.00257131448723));
#46493=CARTESIAN_POINT('Ctrl Pts',(0.,-6.26408070076069,-2.89455177789849));
#46494=CARTESIAN_POINT('Ctrl Pts',(1.5,-6.26408070076069,-2.89455177789849));
#46495=CARTESIAN_POINT('Ctrl Pts',(0.,-6.31325670792693,-2.78566450932763));
#46496=CARTESIAN_POINT('Ctrl Pts',(1.5,-6.31325670792693,-2.78566450932763));
#46497=CARTESIAN_POINT('Ctrl Pts',(0.,-6.36054012011854,-2.67594215120311));
#46498=CARTESIAN_POINT('Ctrl Pts',(1.5,-6.36054012011854,-2.67594215120311));
#46499=CARTESIAN_POINT('Ctrl Pts',(0.,-6.40591676286809,-2.56541759630458));
#46500=CARTESIAN_POINT('Ctrl Pts',(1.5,-6.40591676286809,-2.56541759630458));
#46501=CARTESIAN_POINT('Ctrl Pts',(0.,-6.44937303311288,-2.45412397781148));
#46502=CARTESIAN_POINT('Ctrl Pts',(1.5,-6.44937303311288,-2.45412397781148));
#46503=CARTESIAN_POINT('Ctrl Pts',(0.,-6.49089590327433,-2.34209465936682));
#46504=CARTESIAN_POINT('Ctrl Pts',(1.5,-6.49089590327433,-2.34209465936682));
#46505=CARTESIAN_POINT('Ctrl Pts',(0.,-6.53047292537357,-2.22936322515532));
#46506=CARTESIAN_POINT('Ctrl Pts',(1.5,-6.53047292537357,-2.22936322515532));
#46507=CARTESIAN_POINT('Ctrl Pts',(0.,-6.56809223518283,-2.11596346999528));
#46508=CARTESIAN_POINT('Ctrl Pts',(1.5,-6.56809223518283,-2.11596346999528));
#46509=CARTESIAN_POINT('Ctrl Pts',(0.,-6.60374255535696,-2.00192938906232));
#46510=CARTESIAN_POINT('Ctrl Pts',(1.5,-6.60374255535696,-2.00192938906232));
#46511=CARTESIAN_POINT('Ctrl Pts',(0.,-6.63741319860151,-1.8872951676257));
#46512=CARTESIAN_POINT('Ctrl Pts',(1.5,-6.63741319860151,-1.8872951676257));
#46513=CARTESIAN_POINT('Ctrl Pts',(0.,-6.66909407087783,-1.77209517079654));
#46514=CARTESIAN_POINT('Ctrl Pts',(1.5,-6.66909407087783,-1.77209517079654));
#46515=CARTESIAN_POINT('Ctrl Pts',(0.,-6.69877567464511,-1.65636393328722));
#46516=CARTESIAN_POINT('Ctrl Pts',(1.5,-6.69877567464511,-1.65636393328722));
#46517=CARTESIAN_POINT('Ctrl Pts',(0.,-6.72644911213981,-1.54013614918151));
#46518=CARTESIAN_POINT('Ctrl Pts',(1.5,-6.72644911213981,-1.54013614918151));
#46519=CARTESIAN_POINT('Ctrl Pts',(0.,-6.75210608760682,-1.42344666142604));
#46520=CARTESIAN_POINT('Ctrl Pts',(1.5,-6.75210608760682,-1.42344666142604));
#46521=CARTESIAN_POINT('Ctrl Pts',(0.,-6.77573890956821,-1.30633045133105));
#46522=CARTESIAN_POINT('Ctrl Pts',(1.5,-6.77573890956821,-1.30633045133105));
#46523=CARTESIAN_POINT('Ctrl Pts',(0.,-6.79734049312989,-1.18882262807986));
#46524=CARTESIAN_POINT('Ctrl Pts',(1.5,-6.79734049312989,-1.18882262807986));
#46525=CARTESIAN_POINT('Ctrl Pts',(0.,-6.81690436232613,-1.07095841824634));
#46526=CARTESIAN_POINT('Ctrl Pts',(1.5,-6.81690436232613,-1.07095841824634));
#46527=CARTESIAN_POINT('Ctrl Pts',(0.,-6.83442465250206,-0.952773155319746));
#46528=CARTESIAN_POINT('Ctrl Pts',(1.5,-6.83442465250206,-0.952773155319746));
#46529=CARTESIAN_POINT('Ctrl Pts',(0.,-6.84989611162797,-0.834302269042729));
#46530=CARTESIAN_POINT('Ctrl Pts',(1.5,-6.84989611162797,-0.834302269042729));
#46531=CARTESIAN_POINT('Ctrl Pts',(0.,-6.86331410165185,-0.715581274755232));
#46532=CARTESIAN_POINT('Ctrl Pts',(1.5,-6.86331410165185,-0.715581274755232));
#46533=CARTESIAN_POINT('Ctrl Pts',(0.,-6.87467459989036,-0.596645762743843));
#46534=CARTESIAN_POINT('Ctrl Pts',(1.5,-6.87467459989036,-0.596645762743843));
#46535=CARTESIAN_POINT('Ctrl Pts',(0.,-6.88397420045809,-0.477531387595776));
#46536=CARTESIAN_POINT('Ctrl Pts',(1.5,-6.88397420045809,-0.477531387595776));
#46537=CARTESIAN_POINT('Ctrl Pts',(0.,-6.89121011573542,-0.358273857556864));
#46538=CARTESIAN_POINT('Ctrl Pts',(1.5,-6.89121011573542,-0.358273857556864));
#46539=CARTESIAN_POINT('Ctrl Pts',(0.,-6.89638017675603,-0.238908923795811));
#46540=CARTESIAN_POINT('Ctrl Pts',(1.5,-6.89638017675603,-0.238908923795811));
#46541=CARTESIAN_POINT('Ctrl Pts',(0.,-6.89948283363306,-0.119472369671119));
#46542=CARTESIAN_POINT('Ctrl Pts',(1.5,-6.89948283363306,-0.119472369671119));
#46543=CARTESIAN_POINT('Ctrl Pts',(0.,-6.90051715602375,-6.41517004448811E-14));
#46544=CARTESIAN_POINT('Ctrl Pts',(1.5,-6.90051715602375,-6.41517004448811E-14));
#46545=CARTESIAN_POINT('Ctrl Pts',(0.,-6.89948283363311,0.119472369671016));
#46546=CARTESIAN_POINT('Ctrl Pts',(1.5,-6.89948283363311,0.119472369671016));
#46547=CARTESIAN_POINT('Ctrl Pts',(0.,-6.8963801767561,0.238908923795769));
#46548=CARTESIAN_POINT('Ctrl Pts',(1.5,-6.8963801767561,0.238908923795769));
#46549=CARTESIAN_POINT('Ctrl Pts',(0.,-6.89121011573547,0.358273857556871));
#46550=CARTESIAN_POINT('Ctrl Pts',(1.5,-6.89121011573547,0.358273857556871));
#46551=CARTESIAN_POINT('Ctrl Pts',(0.,-6.88397420045813,0.477531387595768));
#46552=CARTESIAN_POINT('Ctrl Pts',(1.5,-6.88397420045813,0.477531387595768));
#46553=CARTESIAN_POINT('Ctrl Pts',(0.,-6.87467459989038,0.596645762743742));
#46554=CARTESIAN_POINT('Ctrl Pts',(1.5,-6.87467459989038,0.596645762743742));
#46555=CARTESIAN_POINT('Ctrl Pts',(0.,-6.8633141016518,0.715581274754981));
#46556=CARTESIAN_POINT('Ctrl Pts',(1.5,-6.8633141016518,0.715581274754981));
#46557=CARTESIAN_POINT('Ctrl Pts',(0.,-6.84989611162784,0.834302269042349));
#46558=CARTESIAN_POINT('Ctrl Pts',(1.5,-6.84989611162784,0.834302269042349));
#46559=CARTESIAN_POINT('Ctrl Pts',(0.,-6.83442465250195,0.952773155319338));
#46560=CARTESIAN_POINT('Ctrl Pts',(1.5,-6.83442465250195,0.952773155319338));
#46561=CARTESIAN_POINT('Ctrl Pts',(0.,-6.81690436232608,1.07095841824604));
#46562=CARTESIAN_POINT('Ctrl Pts',(1.5,-6.81690436232608,1.07095841824604));
#46563=CARTESIAN_POINT('Ctrl Pts',(0.,-6.79734049312992,1.18882262807975));
#46564=CARTESIAN_POINT('Ctrl Pts',(1.5,-6.79734049312992,1.18882262807975));
#46565=CARTESIAN_POINT('Ctrl Pts',(0.,-6.77573890956825,1.30633045133112));
#46566=CARTESIAN_POINT('Ctrl Pts',(1.5,-6.77573890956825,1.30633045133112));
#46567=CARTESIAN_POINT('Ctrl Pts',(0.,-6.75210608760686,1.42344666142619));
#46568=CARTESIAN_POINT('Ctrl Pts',(1.5,-6.75210608760686,1.42344666142619));
#46569=CARTESIAN_POINT('Ctrl Pts',(0.,-6.72644911213985,1.54013614918161));
#46570=CARTESIAN_POINT('Ctrl Pts',(1.5,-6.72644911213985,1.54013614918161));
#46571=CARTESIAN_POINT('Ctrl Pts',(0.,-6.69877567464515,1.6563639332872));
#46572=CARTESIAN_POINT('Ctrl Pts',(1.5,-6.69877567464515,1.6563639332872));
#46573=CARTESIAN_POINT('Ctrl Pts',(0.,-6.66909407087785,1.77209517079641));
#46574=CARTESIAN_POINT('Ctrl Pts',(1.5,-6.66909407087785,1.77209517079641));
#46575=CARTESIAN_POINT('Ctrl Pts',(0.,-6.63741319860154,1.88729516762555));
#46576=CARTESIAN_POINT('Ctrl Pts',(1.5,-6.63741319860154,1.88729516762555));
#46577=CARTESIAN_POINT('Ctrl Pts',(0.,-6.603742555357,2.0019293890622));
#46578=CARTESIAN_POINT('Ctrl Pts',(1.5,-6.603742555357,2.0019293890622));
#46579=CARTESIAN_POINT('Ctrl Pts',(0.,-6.56809223518289,2.11596346999519));
#46580=CARTESIAN_POINT('Ctrl Pts',(1.5,-6.56809223518289,2.11596346999519));
#46581=CARTESIAN_POINT('Ctrl Pts',(0.,-6.53047292537362,2.22936322515524));
#46582=CARTESIAN_POINT('Ctrl Pts',(1.5,-6.53047292537362,2.22936322515524));
#46583=CARTESIAN_POINT('Ctrl Pts',(0.,-6.49089590327437,2.34209465936671));
#46584=CARTESIAN_POINT('Ctrl Pts',(1.5,-6.49089590327437,2.34209465936671));
#46585=CARTESIAN_POINT('Ctrl Pts',(0.,-6.44937303311289,2.45412397781135));
#46586=CARTESIAN_POINT('Ctrl Pts',(1.5,-6.44937303311289,2.45412397781135));
#46587=CARTESIAN_POINT('Ctrl Pts',(0.,-6.40591676286813,2.56541759630447));
#46588=CARTESIAN_POINT('Ctrl Pts',(1.5,-6.40591676286813,2.56541759630447));
#46589=CARTESIAN_POINT('Ctrl Pts',(0.,-6.3605401201186,2.67594215120304));
#46590=CARTESIAN_POINT('Ctrl Pts',(1.5,-6.3605401201186,2.67594215120304));
#46591=CARTESIAN_POINT('Ctrl Pts',(0.,-6.31325670792698,2.78566450932757));
#46592=CARTESIAN_POINT('Ctrl Pts',(1.5,-6.31325670792698,2.78566450932757));
#46593=CARTESIAN_POINT('Ctrl Pts',(0.,-6.26408070076075,2.8945517778984));
#46594=CARTESIAN_POINT('Ctrl Pts',(1.5,-6.26408070076075,2.8945517778984));
#46595=CARTESIAN_POINT('Ctrl Pts',(0.,-6.2130268404484,3.00257131448706));
#46596=CARTESIAN_POINT('Ctrl Pts',(1.5,-6.2130268404484,3.00257131448706));
#46597=CARTESIAN_POINT('Ctrl Pts',(0.,-6.16011043217123,3.10969073698327));
#46598=CARTESIAN_POINT('Ctrl Pts',(1.5,-6.16011043217123,3.10969073698327));
#46599=CARTESIAN_POINT('Ctrl Pts',(0.,-6.10534733947057,3.2158779331069));
#46600=CARTESIAN_POINT('Ctrl Pts',(1.5,-6.10534733947057,3.2158779331069));
#46601=CARTESIAN_POINT('Ctrl Pts',(0.,-6.04875397928998,3.32110106993695));
#46602=CARTESIAN_POINT('Ctrl Pts',(1.5,-6.04875397928998,3.32110106993695));
#46603=CARTESIAN_POINT('Ctrl Pts',(0.,-5.99034731705195,3.42532860345784));
#46604=CARTESIAN_POINT('Ctrl Pts',(1.5,-5.99034731705195,3.42532860345784));
#46605=CARTESIAN_POINT('Ctrl Pts',(0.,-5.93014486176895,3.52852928812384));
#46606=CARTESIAN_POINT('Ctrl Pts',(1.5,-5.93014486176895,3.52852928812384));
#46607=CARTESIAN_POINT('Ctrl Pts',(0.,-5.86816466118828,3.63067218644218));
#46608=CARTESIAN_POINT('Ctrl Pts',(1.5,-5.86816466118828,3.63067218644218));
#46609=CARTESIAN_POINT('Ctrl Pts',(0.,-5.8044252959957,3.73172667801772));
#46610=CARTESIAN_POINT('Ctrl Pts',(1.5,-5.8044252959957,3.73172667801772));
#46611=CARTESIAN_POINT('Ctrl Pts',(0.,-5.73894587405215,3.83166246861755));
#46612=CARTESIAN_POINT('Ctrl Pts',(1.5,-5.73894587405215,3.83166246861755));
#46613=CARTESIAN_POINT('Ctrl Pts',(0.,-5.67174602466356,3.93044959925594));
#46614=CARTESIAN_POINT('Ctrl Pts',(1.5,-5.67174602466356,3.93044959925594));
#46615=CARTESIAN_POINT('Ctrl Pts',(0.,-5.60284589288313,4.02805845530014));
#46616=CARTESIAN_POINT('Ctrl Pts',(1.5,-5.60284589288313,4.02805845530014));
#46617=CARTESIAN_POINT('Ctrl Pts',(0.,-5.53226613384595,4.12445977559781));
#46618=CARTESIAN_POINT('Ctrl Pts',(1.5,-5.53226613384595,4.12445977559781));
#46619=CARTESIAN_POINT('Ctrl Pts',(0.,-5.46002790621221,4.2196246609867));
#46620=CARTESIAN_POINT('Ctrl Pts',(1.5,-5.46002790621221,4.2196246609867));
#46621=CARTESIAN_POINT('Ctrl Pts',(0.,-5.38615286564171,4.3135245828269));
#46622=CARTESIAN_POINT('Ctrl Pts',(1.5,-5.38615286564171,4.3135245828269));
#46623=CARTESIAN_POINT('Ctrl Pts',(0.,-5.31066315829961,4.40613139155624));
#46624=CARTESIAN_POINT('Ctrl Pts',(1.5,-5.31066315829961,4.40613139155624));
#46625=CARTESIAN_POINT('Ctrl Pts',(0.,-5.2335814143928,4.49741732526956));
#46626=CARTESIAN_POINT('Ctrl Pts',(1.5,-5.2335814143928,4.49741732526956));
#46627=CARTESIAN_POINT('Ctrl Pts',(0.,-5.15493074173648,4.58735501832194));
#46628=CARTESIAN_POINT('Ctrl Pts',(1.5,-5.15493074173648,4.58735501832194));
#46629=CARTESIAN_POINT('Ctrl Pts',(0.,-5.0747347184861,4.67591750923974));
#46630=CARTESIAN_POINT('Ctrl Pts',(1.5,-5.0747347184861,4.67591750923974));
#46631=CARTESIAN_POINT('Ctrl Pts',(0.,-4.9930173858987,4.76307824865654));
#46632=CARTESIAN_POINT('Ctrl Pts',(1.5,-4.9930173858987,4.76307824865654));
#46633=CARTESIAN_POINT('Ctrl Pts',(0.,-4.90980324112317,4.84881110727509));
#46634=CARTESIAN_POINT('Ctrl Pts',(1.5,-4.90980324112317,4.84881110727509));
#46635=CARTESIAN_POINT('Ctrl Pts',(0.,-4.82511723001905,4.93309038385543));
#46636=CARTESIAN_POINT('Ctrl Pts',(1.5,-4.82511723001905,4.93309038385543));
#46637=CARTESIAN_POINT('Ctrl Pts',(0.,-4.73898474000325,5.01589081322972));
#46638=CARTESIAN_POINT('Ctrl Pts',(1.5,-4.73898474000325,5.01589081322972));
#46639=CARTESIAN_POINT('Ctrl Pts',(0.,-4.6514315921253,5.09718757355513));
#46640=CARTESIAN_POINT('Ctrl Pts',(1.5,-4.6514315921253,5.09718757355513));
#46641=CARTESIAN_POINT('Ctrl Pts',(0.,-4.5624840331696,5.17695629359438));
#46642=CARTESIAN_POINT('Ctrl Pts',(1.5,-4.5624840331696,5.17695629359438));
#46643=CARTESIAN_POINT('Ctrl Pts',(0.,-4.47216872778426,5.25517306002443));
#46644=CARTESIAN_POINT('Ctrl Pts',(1.5,-4.47216872778426,5.25517306002443));
#46645=CARTESIAN_POINT('Ctrl Pts',(0.,-4.38051275063613,5.33181442477374));
#46646=CARTESIAN_POINT('Ctrl Pts',(1.5,-4.38051275063613,5.33181442477374));
#46647=CARTESIAN_POINT('Ctrl Pts',(0.,-4.28754357859128,5.40685741238864));
#46648=CARTESIAN_POINT('Ctrl Pts',(1.5,-4.28754357859128,5.40685741238864));
#46649=CARTESIAN_POINT('Ctrl Pts',(0.,-4.19328908219282,5.48027952657378));
#46650=CARTESIAN_POINT('Ctrl Pts',(1.5,-4.19328908219282,5.48027952657378));
#46651=CARTESIAN_POINT('Ctrl Pts',(0.,-4.0977775171632,5.55205875676246));
#46652=CARTESIAN_POINT('Ctrl Pts',(1.5,-4.0977775171632,5.55205875676246));
#46653=CARTESIAN_POINT('Ctrl Pts',(0.,-4.0010375159306,5.62217358471739));
#46654=CARTESIAN_POINT('Ctrl Pts',(1.5,-4.0010375159306,5.62217358471739));
#46655=CARTESIAN_POINT('Ctrl Pts',(0.,-3.90309807917886,5.69060299116221));
#46656=CARTESIAN_POINT('Ctrl Pts',(1.5,-3.90309807917886,5.69060299116221));
#46657=CARTESIAN_POINT('Ctrl Pts',(0.,-3.80398856742053,5.7573264624442));
#46658=CARTESIAN_POINT('Ctrl Pts',(1.5,-3.80398856742053,5.7573264624442));
#46659=CARTESIAN_POINT('Ctrl Pts',(0.,-3.70373869194093,5.82232399631334));
#46660=CARTESIAN_POINT('Ctrl Pts',(1.5,-3.70373869194093,5.82232399631334));
#46661=CARTESIAN_POINT('Ctrl Pts',(0.,-3.60237850576421,5.88557610773341));
#46662=CARTESIAN_POINT('Ctrl Pts',(1.5,-3.60237850576421,5.88557610773341));
#46663=CARTESIAN_POINT('Ctrl Pts',(0.,-3.49993839464077,5.9470638347253));
#46664=CARTESIAN_POINT('Ctrl Pts',(1.5,-3.49993839464077,5.9470638347253));
#46665=CARTESIAN_POINT('Ctrl Pts',(0.,-3.39644906805545,6.00676874424307));
#46666=CARTESIAN_POINT('Ctrl Pts',(1.5,-3.39644906805545,6.00676874424307));
#46667=CARTESIAN_POINT('Ctrl Pts',(0.,-3.29194155025599,6.06467293808312));
#46668=CARTESIAN_POINT('Ctrl Pts',(1.5,-3.29194155025599,6.06467293808312));
#46669=CARTESIAN_POINT('Ctrl Pts',(0.,-3.18644717073138,6.12075905785849));
#46670=CARTESIAN_POINT('Ctrl Pts',(1.5,-3.18644717073138,6.12075905785849));
#46671=CARTESIAN_POINT('Ctrl Pts',(0.,-3.0799975547093,6.17501029000708));
#46672=CARTESIAN_POINT('Ctrl Pts',(1.5,-3.0799975547093,6.17501029000708));
#46673=CARTESIAN_POINT('Ctrl Pts',(0.,-2.97262461367203,6.22741037083384));
#46674=CARTESIAN_POINT('Ctrl Pts',(1.5,-2.97262461367203,6.22741037083384));
#46675=CARTESIAN_POINT('Ctrl Pts',(0.,-2.86436053589025,6.27794359158728));
#46676=CARTESIAN_POINT('Ctrl Pts',(1.5,-2.86436053589025,6.27794359158728));
#46677=CARTESIAN_POINT('Ctrl Pts',(0.,-2.75523777697418,6.32659480357071));
#46678=CARTESIAN_POINT('Ctrl Pts',(1.5,-2.75523777697418,6.32659480357071));
#46679=CARTESIAN_POINT('Ctrl Pts',(0.,-2.64528904995749,6.37334942227483));
#46680=CARTESIAN_POINT('Ctrl Pts',(1.5,-2.64528904995749,6.37334942227483));
#46681=CARTESIAN_POINT('Ctrl Pts',(0.,-2.53454731539729,6.41819343154555));
#46682=CARTESIAN_POINT('Ctrl Pts',(1.5,-2.53454731539729,6.41819343154555));
#46683=CARTESIAN_POINT('Ctrl Pts',(0.,-2.42304577148967,6.46111338778736));
#46684=CARTESIAN_POINT('Ctrl Pts',(1.5,-2.42304577148967,6.46111338778736));
#46685=CARTESIAN_POINT('Ctrl Pts',(0.,-2.31081784419995,6.50209642420256));
#46686=CARTESIAN_POINT('Ctrl Pts',(1.5,-2.31081784419995,6.50209642420256));
#46687=CARTESIAN_POINT('Ctrl Pts',(0.,-2.19789717740723,6.54113025506642));
#46688=CARTESIAN_POINT('Ctrl Pts',(1.5,-2.19789717740723,6.54113025506642));
#46689=CARTESIAN_POINT('Ctrl Pts',(0.,-2.08431762266816,6.57820317898663));
#46690=CARTESIAN_POINT('Ctrl Pts',(1.5,-2.08431762266816,6.57820317898663));
#46691=CARTESIAN_POINT('Ctrl Pts',(0.,-1.97011322899363,6.61330408219934));
#46692=CARTESIAN_POINT('Ctrl Pts',(1.5,-1.97011322899363,6.61330408219934));
#46693=CARTESIAN_POINT('Ctrl Pts',(0.,-1.85531823263787,6.6464224419019));
#46694=CARTESIAN_POINT('Ctrl Pts',(1.5,-1.85531823263787,6.6464224419019));
#46695=CARTESIAN_POINT('Ctrl Pts',(0.,-1.73996704689912,6.67754832962256));
#46696=CARTESIAN_POINT('Ctrl Pts',(1.5,-1.73996704689912,6.67754832962256));
#46697=CARTESIAN_POINT('Ctrl Pts',(0.,-1.62409425193149,6.70667241462728));
#46698=CARTESIAN_POINT('Ctrl Pts',(1.5,-1.62409425193149,6.70667241462728));
#46699=CARTESIAN_POINT('Ctrl Pts',(0.,-1.50773458426516,6.73378596628245));
#46700=CARTESIAN_POINT('Ctrl Pts',(1.5,-1.50773458426516,6.73378596628245));
#46701=CARTESIAN_POINT('Ctrl Pts',(0.,-1.39092292633645,6.75888085645522));
#46702=CARTESIAN_POINT('Ctrl Pts',(1.5,-1.39092292633645,6.75888085645522));
#46703=CARTESIAN_POINT('Ctrl Pts',(0.,-1.2736942960269,6.78194956195135));
#46704=CARTESIAN_POINT('Ctrl Pts',(1.5,-1.2736942960269,6.78194956195135));
#46705=CARTESIAN_POINT('Ctrl Pts',(0.,-1.156083836211,6.802985166991));
#46706=CARTESIAN_POINT('Ctrl Pts',(1.5,-1.156083836211,6.802985166991));
#46707=CARTESIAN_POINT('Ctrl Pts',(0.,-1.0381268043115,6.82198136572236));
#46708=CARTESIAN_POINT('Ctrl Pts',(1.5,-1.0381268043115,6.82198136572236));
#46709=CARTESIAN_POINT('Ctrl Pts',(0.,-0.919858561654649,6.83893246366822));
#46710=CARTESIAN_POINT('Ctrl Pts',(1.5,-0.919858561654649,6.83893246366822));
#46711=CARTESIAN_POINT('Ctrl Pts',(0.,-0.801314562831785,6.85383337921071));
#46712=CARTESIAN_POINT('Ctrl Pts',(1.5,-0.801314562831785,6.85383337921071));
#46713=CARTESIAN_POINT('Ctrl Pts',(0.,-0.682530345066844,6.86667964511437));
#46714=CARTESIAN_POINT('Ctrl Pts',(1.5,-0.682530345066844,6.86667964511437));
#46715=CARTESIAN_POINT('Ctrl Pts',(0.,-0.563541517588961,6.87746741008759));
#46716=CARTESIAN_POINT('Ctrl Pts',(1.5,-0.563541517588961,6.87746741008759));
#46717=CARTESIAN_POINT('Ctrl Pts',(0.,-0.444383751009606,6.88619344038256));
#46718=CARTESIAN_POINT('Ctrl Pts',(1.5,-0.444383751009606,6.88619344038256));
#46719=CARTESIAN_POINT('Ctrl Pts',(0.,-0.325092766592694,6.89285512031881));
#46720=CARTESIAN_POINT('Ctrl Pts',(1.5,-0.325092766592694,6.89285512031881));
#46721=CARTESIAN_POINT('Ctrl Pts',(0.,-0.205704325527824,6.89745045284557));
#46722=CARTESIAN_POINT('Ctrl Pts',(1.5,-0.205704325527824,6.89745045284557));
#46723=CARTESIAN_POINT('Ctrl Pts',(0.,-0.0862542182059904,6.89997806014265));
#46724=CARTESIAN_POINT('Ctrl Pts',(1.5,-0.0862542182059904,6.89997806014265));
#46725=CARTESIAN_POINT('Ctrl Pts',(0.,0.0332217465028425,6.90043718426019));
#46726=CARTESIAN_POINT('Ctrl Pts',(1.5,0.0332217465028425,6.90043718426019));
#46727=CARTESIAN_POINT('Ctrl Pts',(0.,0.152687751971073,6.89882768779694));
#46728=CARTESIAN_POINT('Ctrl Pts',(1.5,0.152687751971073,6.89882768779694));
#46729=CARTESIAN_POINT('Ctrl Pts',(0.,0.272107984548712,6.89515005348743));
#46730=CARTESIAN_POINT('Ctrl Pts',(1.5,0.272107984548712,6.89515005348743));
#46731=CARTESIAN_POINT('Ctrl Pts',(0.,0.39144664429895,6.88940538382782));
#46732=CARTESIAN_POINT('Ctrl Pts',(1.5,0.39144664429895,6.88940538382782));
#46733=CARTESIAN_POINT('Ctrl Pts',(0.,0.510667955734471,6.88159540074063));
#46734=CARTESIAN_POINT('Ctrl Pts',(1.5,0.510667955734471,6.88159540074063));
#46735=CARTESIAN_POINT('Ctrl Pts',(0.,0.629736178555366,6.871722445278));
#46736=CARTESIAN_POINT('Ctrl Pts',(1.5,0.629736178555366,6.871722445278));
#46737=CARTESIAN_POINT('Ctrl Pts',(0.,0.748615618389192,6.85978947736383));
#46738=CARTESIAN_POINT('Ctrl Pts',(1.5,0.748615618389192,6.85978947736383));
#46739=CARTESIAN_POINT('Ctrl Pts',(0.,0.867270637449732,6.84580007446996));
#46740=CARTESIAN_POINT('Ctrl Pts',(1.5,0.867270637449732,6.84580007446996));
#46741=CARTESIAN_POINT('Ctrl Pts',(0.,0.985665665199245,6.82975843033101));
#46742=CARTESIAN_POINT('Ctrl Pts',(1.5,0.985665665199245,6.82975843033101));
#46743=CARTESIAN_POINT('Ctrl Pts',(0.,1.10376520901494,6.81166935369773));
#46744=CARTESIAN_POINT('Ctrl Pts',(1.5,1.10376520901494,6.81166935369773));
#46745=CARTESIAN_POINT('Ctrl Pts',(0.,1.22153386486028,6.7915382671287));
#46746=CARTESIAN_POINT('Ctrl Pts',(1.5,1.22153386486028,6.7915382671287));
#46747=CARTESIAN_POINT('Ctrl Pts',(0.,1.33893632796192,6.76937120582047));
#46748=CARTESIAN_POINT('Ctrl Pts',(1.5,1.33893632796192,6.76937120582047));
#46749=CARTESIAN_POINT('Ctrl Pts',(0.,1.45593740331558,6.74517481533056));
#46750=CARTESIAN_POINT('Ctrl Pts',(1.5,1.45593740331558,6.74517481533056));
#46751=CARTESIAN_POINT('Ctrl Pts',(0.,1.57250201619893,6.71895634933867));
#46752=CARTESIAN_POINT('Ctrl Pts',(1.5,1.57250201619893,6.71895634933867));
#46753=CARTESIAN_POINT('Ctrl Pts',(0.,1.68859522269187,6.69072366744589));
#46754=CARTESIAN_POINT('Ctrl Pts',(1.5,1.68859522269187,6.69072366744589));
#46755=CARTESIAN_POINT('Ctrl Pts',(0.,1.80418222020506,6.66048523301177));
#46756=CARTESIAN_POINT('Ctrl Pts',(1.5,1.80418222020506,6.66048523301177));
#46757=CARTESIAN_POINT('Ctrl Pts',(0.,1.91922835801723,6.62825011102907));
#46758=CARTESIAN_POINT('Ctrl Pts',(1.5,1.91922835801723,6.62825011102907));
#46759=CARTESIAN_POINT('Ctrl Pts',(0.,2.03369914754119,6.59402796503178));
#46760=CARTESIAN_POINT('Ctrl Pts',(1.5,2.03369914754119,6.59402796503178));
#46761=CARTESIAN_POINT('Ctrl Pts',(0.,2.14756027260001,6.55782905404063));
#46762=CARTESIAN_POINT('Ctrl Pts',(1.5,2.14756027260001,6.55782905404063));
#46763=CARTESIAN_POINT('Ctrl Pts',(0.,2.26077759971389,6.51966422954576));
#46764=CARTESIAN_POINT('Ctrl Pts',(1.5,2.26077759971389,6.51966422954576));
#46765=CARTESIAN_POINT('Ctrl Pts',(0.,2.37331718839861,6.47954493252643));
#46766=CARTESIAN_POINT('Ctrl Pts',(1.5,2.37331718839861,6.47954493252643));
#46767=CARTESIAN_POINT('Ctrl Pts',(0.,2.48514530147589,6.4374831905076));
#46768=CARTESIAN_POINT('Ctrl Pts',(1.5,2.48514530147589,6.4374831905076));
#46769=CARTESIAN_POINT('Ctrl Pts',(0.,2.59622841504222,6.39349161339469));
#46770=CARTESIAN_POINT('Ctrl Pts',(1.5,2.59622841504222,6.39349161339469));
#46771=CARTESIAN_POINT('Ctrl Pts',(0.,2.70653322845103,6.34758338934495));
#46772=CARTESIAN_POINT('Ctrl Pts',(1.5,2.70653322845103,6.34758338934495));
#46773=CARTESIAN_POINT('Ctrl Pts',(0.,2.81602667430883,6.29977228067472));
#46774=CARTESIAN_POINT('Ctrl Pts',(1.5,2.81602667430883,6.29977228067472));
#46775=CARTESIAN_POINT('Ctrl Pts',(0.,2.92467592848589,6.25007261980284));
#46776=CARTESIAN_POINT('Ctrl Pts',(1.5,2.92467592848589,6.25007261980284));
#46777=CARTESIAN_POINT('Ctrl Pts',(0.,3.03244842014215,6.19849930522943));
#46778=CARTESIAN_POINT('Ctrl Pts',(1.5,3.03244842014215,6.19849930522943));
#46779=CARTESIAN_POINT('Ctrl Pts',(0.,3.13931184127864,6.14506779698229));
#46780=CARTESIAN_POINT('Ctrl Pts',(1.5,3.13931184127864,6.14506779698229));
#46781=CARTESIAN_POINT('Ctrl Pts',(0.,3.24523415630526,6.08979411209844));
#46782=CARTESIAN_POINT('Ctrl Pts',(1.5,3.24523415630526,6.08979411209844));
#46783=CARTESIAN_POINT('Ctrl Pts',(0.,3.35018361162562,6.03269482014039));
#46784=CARTESIAN_POINT('Ctrl Pts',(1.5,3.35018361162562,6.03269482014039));
#46785=CARTESIAN_POINT('Ctrl Pts',(0.,3.45412874523943,5.97378703874699));
#46786=CARTESIAN_POINT('Ctrl Pts',(1.5,3.45412874523943,5.97378703874699));
#46787=CARTESIAN_POINT('Ctrl Pts',(0.,3.55703839636324,5.91308842921844));
#46788=CARTESIAN_POINT('Ctrl Pts',(1.5,3.55703839636324,5.91308842921844));
#46789=CARTESIAN_POINT('Ctrl Pts',(0.,3.65888171459873,5.85061719009051));
#46790=CARTESIAN_POINT('Ctrl Pts',(1.5,3.65888171459873,5.85061719009051));
#46791=CARTESIAN_POINT('Ctrl Pts',(0.,3.75962816912046,5.78639205074214));
#46792=CARTESIAN_POINT('Ctrl Pts',(1.5,3.75962816912046,5.78639205074214));
#46793=CARTESIAN_POINT('Ctrl Pts',(0.,3.85924755788358,5.72043226503629));
#46794=CARTESIAN_POINT('Ctrl Pts',(1.5,3.85924755788358,5.72043226503629));
#46795=CARTESIAN_POINT('Ctrl Pts',(0.,3.95771001685206,5.65275760499367));
#46796=CARTESIAN_POINT('Ctrl Pts',(1.5,3.95771001685206,5.65275760499367));
#46797=CARTESIAN_POINT('Ctrl Pts',(0.,4.05498602924811,5.58338835449887));
#46798=CARTESIAN_POINT('Ctrl Pts',(1.5,4.05498602924811,5.58338835449887));
#46799=CARTESIAN_POINT('Ctrl Pts',(0.,4.15104643402264,5.51234530457567));
#46800=CARTESIAN_POINT('Ctrl Pts',(1.5,4.15104643402264,5.51234530457567));
#46801=CARTESIAN_POINT('Ctrl Pts',(0.,4.24586243434801,5.43964974869428));
#46802=CARTESIAN_POINT('Ctrl Pts',(1.5,4.24586243434801,5.43964974869428));
#46803=CARTESIAN_POINT('Ctrl Pts',(0.,4.33940560613354,5.36532347810979));
#46804=CARTESIAN_POINT('Ctrl Pts',(1.5,4.33940560613354,5.36532347810979));
#46805=CARTESIAN_POINT('Ctrl Pts',(0.,4.43164790656429,5.28938877723184));
#46806=CARTESIAN_POINT('Ctrl Pts',(1.5,4.43164790656429,5.28938877723184));
#46807=CARTESIAN_POINT('Ctrl Pts',(0.,4.52256168266372,5.2118684190248));
#46808=CARTESIAN_POINT('Ctrl Pts',(1.5,4.52256168266372,5.2118684190248));
#46809=CARTESIAN_POINT('Ctrl Pts',(0.,4.61211967957445,5.13278565383194));
#46810=CARTESIAN_POINT('Ctrl Pts',(1.5,4.61211967957445,5.13278565383194));
#46811=CARTESIAN_POINT('Ctrl Pts',(0.,4.70029504886408,5.05216419822939));
#46812=CARTESIAN_POINT('Ctrl Pts',(1.5,4.70029504886408,5.05216419822939));
#46813=CARTESIAN_POINT('Ctrl Pts',(0.,4.78706135685631,4.97002822390918));
#46814=CARTESIAN_POINT('Ctrl Pts',(1.5,4.78706135685631,4.97002822390918));
#46815=CARTESIAN_POINT('Ctrl Pts',(0.,4.87239259298801,4.88640234659105));
#46816=CARTESIAN_POINT('Ctrl Pts',(1.5,4.87239259298801,4.88640234659105));
#46817=CARTESIAN_POINT('Ctrl Pts',(0.,4.95626317819269,4.80131161496197));
#46818=CARTESIAN_POINT('Ctrl Pts',(1.5,4.95626317819269,4.80131161496197));
#46819=CARTESIAN_POINT('Ctrl Pts',(0.,5.03864797160205,4.71478151214967));
#46820=CARTESIAN_POINT('Ctrl Pts',(1.5,5.03864797160205,4.71478151214967));
#46821=CARTESIAN_POINT('Ctrl Pts',(0.,5.11952227727493,4.62683795722329));
#46822=CARTESIAN_POINT('Ctrl Pts',(1.5,5.11952227727493,4.62683795722329));
#46823=CARTESIAN_POINT('Ctrl Pts',(0.,5.19886185095397,4.53750730672122));
#46824=CARTESIAN_POINT('Ctrl Pts',(1.5,5.19886185095397,4.53750730672122));
#46825=CARTESIAN_POINT('Ctrl Pts',(0.,5.27664290685066,4.44681635620587));
#46826=CARTESIAN_POINT('Ctrl Pts',(1.5,5.27664290685066,4.44681635620587));
#46827=CARTESIAN_POINT('Ctrl Pts',(0.,5.35284212445892,4.35479234184536));
#46828=CARTESIAN_POINT('Ctrl Pts',(1.5,5.35284212445892,4.35479234184536));
#46829=CARTESIAN_POINT('Ctrl Pts',(0.,5.42743665671074,4.2614629103579));
#46830=CARTESIAN_POINT('Ctrl Pts',(1.5,5.42743665671074,4.2614629103579));
#46831=CARTESIAN_POINT('Ctrl Pts',(0.,5.50040413816131,4.16685608898156));
#46832=CARTESIAN_POINT('Ctrl Pts',(1.5,5.50040413816131,4.16685608898156));
#46833=CARTESIAN_POINT('Ctrl Pts',(0.,5.57172269320426,4.07100025546809));
#46834=CARTESIAN_POINT('Ctrl Pts',(1.5,5.57172269320426,4.07100025546809));
#46835=CARTESIAN_POINT('Ctrl Pts',(0.,5.64137094431753,3.97392410809942));
#46836=CARTESIAN_POINT('Ctrl Pts',(1.5,5.64137094431753,3.97392410809942));
#46837=CARTESIAN_POINT('Ctrl Pts',(0.,5.70932802034013,3.87565663572553));
#46838=CARTESIAN_POINT('Ctrl Pts',(1.5,5.70932802034013,3.87565663572553));
#46839=CARTESIAN_POINT('Ctrl Pts',(0.,5.77557355885907,3.7762271589849));
#46840=CARTESIAN_POINT('Ctrl Pts',(1.5,5.77557355885907,3.7762271589849));
#46841=CARTESIAN_POINT('Ctrl Pts',(0.,5.84008770862796,3.67566537154607));
#46842=CARTESIAN_POINT('Ctrl Pts',(1.5,5.84008770862796,3.67566537154607));
#46843=CARTESIAN_POINT('Ctrl Pts',(0.,5.90285113201758,3.57400138137221));
#46844=CARTESIAN_POINT('Ctrl Pts',(1.5,5.90285113201758,3.57400138137221));
#46845=CARTESIAN_POINT('Ctrl Pts',(0.,5.96384500749881,3.47126575200941));
#46846=CARTESIAN_POINT('Ctrl Pts',(1.5,5.96384500749881,3.47126575200941));
#46847=CARTESIAN_POINT('Ctrl Pts',(0.,6.0230510321579,3.36748954390066));
#46848=CARTESIAN_POINT('Ctrl Pts',(1.5,6.0230510321579,3.36748954390066));
#46849=CARTESIAN_POINT('Ctrl Pts',(0.,6.08045143492985,3.26270418832904));
#46850=CARTESIAN_POINT('Ctrl Pts',(1.5,6.08045143492985,3.26270418832904));
#46851=CARTESIAN_POINT('Ctrl Pts',(0.,6.1360289898651,3.15694136138284));
#46852=CARTESIAN_POINT('Ctrl Pts',(1.5,6.1360289898651,3.15694136138284));
#46853=CARTESIAN_POINT('Ctrl Pts',(0.,6.18976702943025,3.05023285793733));
#46854=CARTESIAN_POINT('Ctrl Pts',(1.5,6.18976702943025,3.05023285793733));
#46855=CARTESIAN_POINT('Ctrl Pts',(0.,6.24164945784326,2.94261046564829));
#46856=CARTESIAN_POINT('Ctrl Pts',(1.5,6.24164945784326,2.94261046564829));
#46857=CARTESIAN_POINT('Ctrl Pts',(0.,6.291660764444,2.83410583895225));
#46858=CARTESIAN_POINT('Ctrl Pts',(1.5,6.291660764444,2.83410583895225));
#46859=CARTESIAN_POINT('Ctrl Pts',(0.,6.339786009045,2.72475075998752));
#46860=CARTESIAN_POINT('Ctrl Pts',(1.5,6.339786009045,2.72475075998752));
#46861=CARTESIAN_POINT('Ctrl Pts',(0.,6.38601080731774,2.61457739952658));
#46862=CARTESIAN_POINT('Ctrl Pts',(1.5,6.38601080731774,2.61457739952658));
#46863=CARTESIAN_POINT('Ctrl Pts',(0.,6.43032131621382,2.50361857792934));
#46864=CARTESIAN_POINT('Ctrl Pts',(1.5,6.43032131621382,2.50361857792934));
#46865=CARTESIAN_POINT('Ctrl Pts',(0.,6.47270421942066,2.39190802612696));
#46866=CARTESIAN_POINT('Ctrl Pts',(1.5,6.47270421942066,2.39190802612696));
#46867=CARTESIAN_POINT('Ctrl Pts',(0.,6.51314671285136,2.27948064664619));
#46868=CARTESIAN_POINT('Ctrl Pts',(1.5,6.51314671285136,2.27948064664619));
#46869=CARTESIAN_POINT('Ctrl Pts',(0.,6.55163655192191,2.1663718749224));
#46870=CARTESIAN_POINT('Ctrl Pts',(1.5,6.55163655192191,2.1663718749224));
#46871=CARTESIAN_POINT('Ctrl Pts',(0.,6.58816209886384,2.05261704063847));
#46872=CARTESIAN_POINT('Ctrl Pts',(1.5,6.58816209886384,2.05261704063847));
#46873=CARTESIAN_POINT('Ctrl Pts',(0.,6.62271237007439,1.93825072906452));
#46874=CARTESIAN_POINT('Ctrl Pts',(1.5,6.62271237007439,1.93825072906452));
#46875=CARTESIAN_POINT('Ctrl Pts',(0.,6.65527708350579,1.82330614237472));
#46876=CARTESIAN_POINT('Ctrl Pts',(1.5,6.65527708350579,1.82330614237472));
#46877=CARTESIAN_POINT('Ctrl Pts',(0.,6.6858467060959,1.70781446091566));
#46878=CARTESIAN_POINT('Ctrl Pts',(1.5,6.6858467060959,1.70781446091566));
#46879=CARTESIAN_POINT('Ctrl Pts',(0.,6.71441235475264,1.59180628284183));
#46880=CARTESIAN_POINT('Ctrl Pts',(1.5,6.71441235475264,1.59180628284183));
#46881=CARTESIAN_POINT('Ctrl Pts',(0.,6.74096569737792,1.47531306373213));
#46882=CARTESIAN_POINT('Ctrl Pts',(1.5,6.74096569737792,1.47531306373213));
#46883=CARTESIAN_POINT('Ctrl Pts',(0.,6.76549885392711,1.35836855624325));
#46884=CARTESIAN_POINT('Ctrl Pts',(1.5,6.76549885392711,1.35836855624325));
#46885=CARTESIAN_POINT('Ctrl Pts',(0.,6.78800429750073,1.24101024985218));
#46886=CARTESIAN_POINT('Ctrl Pts',(1.5,6.78800429750073,1.24101024985218));
#46887=CARTESIAN_POINT('Ctrl Pts',(0.,6.80847475546411,1.12328081074528));
#46888=CARTESIAN_POINT('Ctrl Pts',(1.5,6.80847475546411,1.12328081074528));
#46889=CARTESIAN_POINT('Ctrl Pts',(0.,6.82690343687802,1.00522492629014));
#46890=CARTESIAN_POINT('Ctrl Pts',(1.5,6.82690343687802,1.00522492629014));
#46891=CARTESIAN_POINT('Ctrl Pts',(0.,6.84328425996227,0.886886149588873));
#46892=CARTESIAN_POINT('Ctrl Pts',(1.5,6.84328425996227,0.886886149588873));
#46893=CARTESIAN_POINT('Ctrl Pts',(0.,6.85761207960138,0.768303743989806));
#46894=CARTESIAN_POINT('Ctrl Pts',(1.5,6.85761207960138,0.768303743989806));
#46895=CARTESIAN_POINT('Ctrl Pts',(0.,6.8698829149006,0.649509527441057));
#46896=CARTESIAN_POINT('Ctrl Pts',(1.5,6.8698829149006,0.649509527441057));
#46897=CARTESIAN_POINT('Ctrl Pts',(0.,6.88009417680139,0.530524716562488));
#46898=CARTESIAN_POINT('Ctrl Pts',(1.5,6.88009417680139,0.530524716562488));
#46899=CARTESIAN_POINT('Ctrl Pts',(0.,6.88824437408576,0.411362046113686));
#46900=CARTESIAN_POINT('Ctrl Pts',(1.5,6.88824437408576,0.411362046113686));
#46901=CARTESIAN_POINT('Ctrl Pts',(0.,6.89311513036717,0.315894719735552));
#46902=CARTESIAN_POINT('Ctrl Pts',(1.5,6.89311513036717,0.315894719735552));
#46903=CARTESIAN_POINT('Ctrl Pts',(0.,6.89584032942016,0.244218013275557));
#46904=CARTESIAN_POINT('Ctrl Pts',(1.5,6.89584032942016,0.244218013275557));
#46905=CARTESIAN_POINT('Ctrl Pts',(0.,6.89724474811979,0.19639967087135));
#46906=CARTESIAN_POINT('Ctrl Pts',(1.5,6.89724474811979,0.19639967087135));
#46907=CARTESIAN_POINT('Ctrl Pts',(0.,6.89784386230235,0.172482031811515));
#46908=CARTESIAN_POINT('Ctrl Pts',(1.5,6.89784386230235,0.172482031811515));
#46909=CARTESIAN_POINT('',(0.15,6.89784386230235,0.172482031811515));
#46910=CARTESIAN_POINT('Ctrl Pts',(0.15,6.89784386230235,0.172482031811515));
#46911=CARTESIAN_POINT('Ctrl Pts',(0.15,6.89384976775196,0.33193295887695));
#46912=CARTESIAN_POINT('Ctrl Pts',(0.15,6.86721937301695,0.769068553785531));
#46913=CARTESIAN_POINT('Ctrl Pts',(0.15,6.55672403346259,2.80069104006913));
#46914=CARTESIAN_POINT('Ctrl Pts',(0.15,4.55753706787808,5.94536461879026));
#46915=CARTESIAN_POINT('Ctrl Pts',(0.15,0.47740476259414,7.22297137435857));
#46916=CARTESIAN_POINT('Ctrl Pts',(0.15,-1.94905218134993,6.66877212629907));
#46917=CARTESIAN_POINT('Ctrl Pts',(0.15,-3.08518241062154,6.18617418921297));
#46918=CARTESIAN_POINT('Ctrl Pts',(0.15,-3.64702096578107,5.88077380485089));
#46919=CARTESIAN_POINT('Ctrl Pts',(0.15,-5.26204057710086,4.712638335515));
#46920=CARTESIAN_POINT('Ctrl Pts',(0.15,-6.87917153567566,2.33560060230451));
#46921=CARTESIAN_POINT('Ctrl Pts',(0.15,-7.00981900784351,-0.786370144444264));
#46922=CARTESIAN_POINT('Ctrl Pts',(0.15,-6.18684609770483,-3.3390146085407));
#46923=CARTESIAN_POINT('Ctrl Pts',(0.15,-4.52929209771623,-5.56835397775588));
#46924=CARTESIAN_POINT('Ctrl Pts',(0.15,-1.64828395884492,-6.94189872669882));
#46925=CARTESIAN_POINT('Ctrl Pts',(0.15,1.31036395343999,-6.93807076453762));
#46926=CARTESIAN_POINT('Ctrl Pts',(0.15,3.04585995518473,-6.26002474355005));
#46927=CARTESIAN_POINT('Ctrl Pts',(0.15,3.89276415816284,-5.6989278508729));
#46928=CARTESIAN_POINT('Ctrl Pts',(0.15,4.50883595665535,-5.25964112637036));
#46929=CARTESIAN_POINT('Ctrl Pts',(0.15,5.52985079048928,-4.29339059730747));
#46930=CARTESIAN_POINT('Ctrl Pts',(0.15,6.22991610706792,-3.06655667805971));
#46931=CARTESIAN_POINT('Ctrl Pts',(0.15,6.74221885100022,-1.64238122846297));
#46932=CARTESIAN_POINT('Ctrl Pts',(0.15,6.87986895437252,-0.890015525613691));
#46933=CARTESIAN_POINT('Ctrl Pts',(0.15,6.89784369771306,-0.172488601988405));
#46934=CARTESIAN_POINT('',(0.,6.89784386230235,0.172482031811515));
#46935=CARTESIAN_POINT('Ctrl Pts',(0.15,6.89784402687909,-0.172475461633085));
#46936=CARTESIAN_POINT('Ctrl Pts',(0.15,6.87987054647832,-0.890006823484593));
#46937=CARTESIAN_POINT('Ctrl Pts',(0.15,6.74222033236675,-1.64237711033971));
#46938=CARTESIAN_POINT('Ctrl Pts',(0.15,6.22991610706792,-3.06655667805971));
#46939=CARTESIAN_POINT('Ctrl Pts',(0.15,5.52985079048928,-4.29339059730747));
#46940=CARTESIAN_POINT('Ctrl Pts',(0.15,4.50883595665535,-5.25964112637036));
#46941=CARTESIAN_POINT('Ctrl Pts',(0.15,3.89276415816284,-5.6989278508729));
#46942=CARTESIAN_POINT('Ctrl Pts',(0.15,3.04585995518473,-6.26002474355005));
#46943=CARTESIAN_POINT('Ctrl Pts',(0.15,1.31036395343999,-6.93807076453762));
#46944=CARTESIAN_POINT('Ctrl Pts',(0.15,-1.64828395884492,-6.94189872669882));
#46945=CARTESIAN_POINT('Ctrl Pts',(0.15,-4.52929209771623,-5.56835397775588));
#46946=CARTESIAN_POINT('Ctrl Pts',(0.15,-6.18684609770483,-3.3390146085407));
#46947=CARTESIAN_POINT('Ctrl Pts',(0.15,-7.00981900784351,-0.786370144444264));
#46948=CARTESIAN_POINT('Ctrl Pts',(0.15,-6.87917153567566,2.33560060230451));
#46949=CARTESIAN_POINT('Ctrl Pts',(0.15,-5.26204057710086,4.712638335515));
#46950=CARTESIAN_POINT('Ctrl Pts',(0.15,-3.64702096578107,5.88077380485089));
#46951=CARTESIAN_POINT('Ctrl Pts',(0.15,-3.08518241062154,6.18617418921297));
#46952=CARTESIAN_POINT('Ctrl Pts',(0.15,-1.94905218134993,6.66877212629907));
#46953=CARTESIAN_POINT('Ctrl Pts',(0.15,0.47740476259414,7.22297137435857));
#46954=CARTESIAN_POINT('Ctrl Pts',(0.15,4.55753706787808,5.94536461879026));
#46955=CARTESIAN_POINT('Ctrl Pts',(0.15,6.55672403346259,2.80069104006913));
#46956=CARTESIAN_POINT('Ctrl Pts',(0.15,6.86721937301695,0.769068553785531));
#46957=CARTESIAN_POINT('Ctrl Pts',(0.15,6.89384976775196,0.33193295887695));
#46958=CARTESIAN_POINT('Ctrl Pts',(0.15,6.89784386230235,0.172482031811515));
#46959=CARTESIAN_POINT('Ctrl Pts',(0.1,6.94782834788194,-0.173727521489497));
#46960=CARTESIAN_POINT('Ctrl Pts',(0.1,6.9297284773311,-0.89644913748462));
#46961=CARTESIAN_POINT('Ctrl Pts',(0.0999999999999999,6.79107540015654,
-1.65427761636173));
#46962=CARTESIAN_POINT('Ctrl Pts',(0.1,6.27506228900912,-3.08877763008951));
#46963=CARTESIAN_POINT('Ctrl Pts',(0.0999999999999999,5.56992168908083,
-4.32450087751743));
#46964=CARTESIAN_POINT('Ctrl Pts',(0.1,4.54150877965936,-5.29775537284816));
#46965=CARTESIAN_POINT('Ctrl Pts',(0.1,3.92097241788847,-5.74022297978704));
#46966=CARTESIAN_POINT('Ctrl Pts',(0.1,3.06793267773209,-6.30539378926051));
#46967=CARTESIAN_POINT('Ctrl Pts',(0.1,1.3198586472779,-6.98834205805805));
#46968=CARTESIAN_POINT('Ctrl Pts',(0.1,-1.66022698490003,-6.99220544238868));
#46969=CARTESIAN_POINT('Ctrl Pts',(0.1,-4.5621155749862,-5.60870389753307));
#46970=CARTESIAN_POINT('Ctrl Pts',(0.1,-6.23167543831412,-3.36320956230316));
#46971=CARTESIAN_POINT('Ctrl Pts',(0.1,-7.06061739245503,-0.792066536063253));
#46972=CARTESIAN_POINT('Ctrl Pts',(0.1,-6.92901318894491,2.35251318914951));
#46973=CARTESIAN_POINT('Ctrl Pts',(0.1,-5.30018968931025,4.74681443790138));
#46974=CARTESIAN_POINT('Ctrl Pts',(0.1,-3.67344113870542,5.92337668599479));
#46975=CARTESIAN_POINT('Ctrl Pts',(0.1,-3.10753747551775,6.23101823378308));
#46976=CARTESIAN_POINT('Ctrl Pts',(0.1,-1.96317749500257,6.71706621716312));
#46977=CARTESIAN_POINT('Ctrl Pts',(0.1,0.480873909248904,7.27533423073512));
#46978=CARTESIAN_POINT('Ctrl Pts',(0.0999999999999999,4.59054244474249,
5.98843108463992));
#46979=CARTESIAN_POINT('Ctrl Pts',(0.1,6.60427005889709,2.82099242255299));
#46980=CARTESIAN_POINT('Ctrl Pts',(0.1,6.91696548261244,0.77463982747282));
#46981=CARTESIAN_POINT('Ctrl Pts',(0.1,6.94381611987537,0.334338463222424));
#46982=CARTESIAN_POINT('Ctrl Pts',(0.1,6.94782818330531,0.17373409166339));
#46983=CARTESIAN_POINT('Ctrl Pts',(0.05,6.99781266888479,-0.174979581345908));
#46984=CARTESIAN_POINT('Ctrl Pts',(0.0499999999999999,6.9799655786341,-0.887320689053801));
#46985=CARTESIAN_POINT('Ctrl Pts',(0.0500000000000001,6.83996736785432,
-1.6648587174595));
#46986=CARTESIAN_POINT('Ctrl Pts',(0.0499999999999998,6.32027603624419,
-3.10810475947495));
#46987=CARTESIAN_POINT('Ctrl Pts',(0.0500000000000002,5.60999847637134,
-4.35544803176837));
#46988=CARTESIAN_POINT('Ctrl Pts',(0.0499999999999999,4.57419179627318,
-5.33545786922552));
#46989=CARTESIAN_POINT('Ctrl Pts',(0.05,3.9491897409667,-5.78118915940952));
#46990=CARTESIAN_POINT('Ctrl Pts',(0.05,3.09000963553784,-6.35042977939185));
#46991=CARTESIAN_POINT('Ctrl Pts',(0.05,1.32935705385206,-7.03856408743832));
#46992=CARTESIAN_POINT('Ctrl Pts',(0.0500000000000001,-1.6721716011548,
-7.0424409921364));
#46993=CARTESIAN_POINT('Ctrl Pts',(0.0499999999999999,-4.59493164670564,
-5.64906110396198));
#46994=CARTESIAN_POINT('Ctrl Pts',(0.05,-6.27651326142051,-3.38740106795732));
#46995=CARTESIAN_POINT('Ctrl Pts',(0.0499999999999999,-7.1114079969986,
-0.797768849285689));
#46996=CARTESIAN_POINT('Ctrl Pts',(0.05,-6.97887705298601,2.36946336996088));
#46997=CARTESIAN_POINT('Ctrl Pts',(0.0499999999999999,-5.33828367410731,
4.7809108444846));
#46998=CARTESIAN_POINT('Ctrl Pts',(0.05,-3.69988388432588,5.96601397199249));
#46999=CARTESIAN_POINT('Ctrl Pts',(0.05,-3.12989656095608,6.27581229321813));
#47000=CARTESIAN_POINT('Ctrl Pts',(0.05,-1.97729763925328,6.76545163088962));
#47001=CARTESIAN_POINT('Ctrl Pts',(0.05,0.484314506462699,7.3276264869806));
#47002=CARTESIAN_POINT('Ctrl Pts',(0.05,4.62360674015065,6.03155341936274));
#47003=CARTESIAN_POINT('Ctrl Pts',(0.05,6.65171580610762,2.84126752862509));
#47004=CARTESIAN_POINT('Ctrl Pts',(0.05,6.96676043939284,0.780220974861774));
#47005=CARTESIAN_POINT('Ctrl Pts',(0.05,6.99374990469226,0.336735818443863));
#47006=CARTESIAN_POINT('Ctrl Pts',(0.05,6.99781250430828,0.174986151515265));
#47007=CARTESIAN_POINT('Ctrl Pts',(0.,7.04779698988764,-0.176231641202319));
#47008=CARTESIAN_POINT('Ctrl Pts',(0.,7.02982350948688,-0.893763003053827));
#47009=CARTESIAN_POINT('Ctrl Pts',(0.,6.88882243564412,-1.67675922348152));
#47010=CARTESIAN_POINT('Ctrl Pts',(0.,6.3654222181854,-3.13032571150475));
#47011=CARTESIAN_POINT('Ctrl Pts',(0.,5.6500693749629,-4.38655831197832));
#47012=CARTESIAN_POINT('Ctrl Pts',(0.,4.60686461927718,-5.37357211570332));
#47013=CARTESIAN_POINT('Ctrl Pts',(0.,3.97739800069233,-5.82248428832366));
#47014=CARTESIAN_POINT('Ctrl Pts',(0.,3.11208235808519,-6.39579882510231));
#47015=CARTESIAN_POINT('Ctrl Pts',(0.,1.33885174768997,-7.08883538095876));
#47016=CARTESIAN_POINT('Ctrl Pts',(0.,-1.68411462720991,-7.09274770782626));
#47017=CARTESIAN_POINT('Ctrl Pts',(0.,-4.6277551239756,-5.68941102373917));
#47018=CARTESIAN_POINT('Ctrl Pts',(0.,-6.32134260202981,-3.41159602171978));
#47019=CARTESIAN_POINT('Ctrl Pts',(0.,-7.16220638161012,-0.803465240904679));
#47020=CARTESIAN_POINT('Ctrl Pts',(0.,-7.02871870625526,2.38637595680587));
#47021=CARTESIAN_POINT('Ctrl Pts',(0.,-5.37643278631671,4.81508694687098));
#47022=CARTESIAN_POINT('Ctrl Pts',(0.,-3.72630405725022,6.00861685313639));
#47023=CARTESIAN_POINT('Ctrl Pts',(0.,-3.15225162585228,6.32065633778824));
#47024=CARTESIAN_POINT('Ctrl Pts',(0.,-1.99142295290593,6.81374572175368));
#47025=CARTESIAN_POINT('Ctrl Pts',(0.,0.487783653117462,7.37998934335715));
#47026=CARTESIAN_POINT('Ctrl Pts',(0.,4.65661211701506,6.07461988521239));
#47027=CARTESIAN_POINT('Ctrl Pts',(0.,6.69926183154212,2.86156891110894));
#47028=CARTESIAN_POINT('Ctrl Pts',(0.,7.01650654898832,0.785792248549063));
#47029=CARTESIAN_POINT('Ctrl Pts',(0.,7.04371625681567,0.339141322789337));
#47030=CARTESIAN_POINT('Ctrl Pts',(0.,7.04779682531124,0.17623821136714));
#47031=CARTESIAN_POINT('',(0.,7.0477969074555,0.176234926281131));
#47032=CARTESIAN_POINT('Ctrl Pts',(0.,7.04779682531124,0.17623821136714));
#47033=CARTESIAN_POINT('Ctrl Pts',(0.05,6.99781250430828,0.174986151515265));
#47034=CARTESIAN_POINT('Ctrl Pts',(0.1,6.94782818330531,0.17373409166339));
#47035=CARTESIAN_POINT('Ctrl Pts',(0.15,6.89784386230235,0.172482031811515));
#47036=CARTESIAN_POINT('Ctrl Pts',(0.,7.04779698988764,-0.176231641202319));
#47037=CARTESIAN_POINT('Ctrl Pts',(0.,7.02982350948688,-0.893763003053827));
#47038=CARTESIAN_POINT('Ctrl Pts',(0.,6.88882243564412,-1.67675922348152));
#47039=CARTESIAN_POINT('Ctrl Pts',(0.,6.3654222181854,-3.13032571150475));
#47040=CARTESIAN_POINT('Ctrl Pts',(0.,5.6500693749629,-4.38655831197832));
#47041=CARTESIAN_POINT('Ctrl Pts',(0.,4.60686461927718,-5.37357211570332));
#47042=CARTESIAN_POINT('Ctrl Pts',(0.,3.97739800069233,-5.82248428832366));
#47043=CARTESIAN_POINT('Ctrl Pts',(0.,3.11208235808519,-6.39579882510231));
#47044=CARTESIAN_POINT('Ctrl Pts',(0.,1.33885174768997,-7.08883538095876));
#47045=CARTESIAN_POINT('Ctrl Pts',(0.,-1.68411462720991,-7.09274770782626));
#47046=CARTESIAN_POINT('Ctrl Pts',(0.,-4.6277551239756,-5.68941102373917));
#47047=CARTESIAN_POINT('Ctrl Pts',(0.,-6.32134260202981,-3.41159602171978));
#47048=CARTESIAN_POINT('Ctrl Pts',(0.,-7.16220638161012,-0.803465240904679));
#47049=CARTESIAN_POINT('Ctrl Pts',(0.,-7.02871870625526,2.38637595680587));
#47050=CARTESIAN_POINT('Ctrl Pts',(0.,-5.37643278631671,4.81508694687098));
#47051=CARTESIAN_POINT('Ctrl Pts',(0.,-3.72630405725022,6.00861685313639));
#47052=CARTESIAN_POINT('Ctrl Pts',(0.,-3.15225162585228,6.32065633778824));
#47053=CARTESIAN_POINT('Ctrl Pts',(0.,-1.99142295290593,6.81374572175368));
#47054=CARTESIAN_POINT('Ctrl Pts',(0.,0.487783653117462,7.37998934335715));
#47055=CARTESIAN_POINT('Ctrl Pts',(0.,4.65661211701506,6.07461988521239));
#47056=CARTESIAN_POINT('Ctrl Pts',(0.,6.69926183154212,2.86156891110894));
#47057=CARTESIAN_POINT('Ctrl Pts',(0.,7.01650654898832,0.785792248549063));
#47058=CARTESIAN_POINT('Ctrl Pts',(0.,7.04371625681567,0.339141322789337));
#47059=CARTESIAN_POINT('Ctrl Pts',(0.,7.04779682531124,0.17623821136714));
#47060=CARTESIAN_POINT('Origin',(0.,6.89784386230235,0.172482031811515));
#47061=CARTESIAN_POINT('',(1.5,6.89784386230235,0.172482031811515));
#47062=CARTESIAN_POINT('',(0.,6.89784386230235,0.172482031811515));
#47063=CARTESIAN_POINT('Origin',(1.5,-0.0015497354906735,4.21884749357559E-14));
#47064=CARTESIAN_POINT('Origin',(0.,-0.0015497354906735,4.21884749357559E-14));
#47065=CARTESIAN_POINT('',(0.,0.,0.));
#47066=CARTESIAN_POINT('Ctrl Pts',(27.,9.2,0.));
#47067=CARTESIAN_POINT('Ctrl Pts',(27.,9.2,9.2));
#47068=CARTESIAN_POINT('Ctrl Pts',(27.,0.,9.2));
#47069=CARTESIAN_POINT('Ctrl Pts',(27.,-9.2,9.2));
#47070=CARTESIAN_POINT('Ctrl Pts',(27.,-9.2,0.));
#47071=CARTESIAN_POINT('Ctrl Pts',(27.,-9.2,-9.2));
#47072=CARTESIAN_POINT('Ctrl Pts',(27.,0.,-9.2));
#47073=CARTESIAN_POINT('Ctrl Pts',(27.,9.2,-9.2));
#47074=CARTESIAN_POINT('Ctrl Pts',(27.,9.2,0.));
#47075=CARTESIAN_POINT('Ctrl Pts',(26.796570998452,9.22636560737002,0.));
#47076=CARTESIAN_POINT('Ctrl Pts',(26.796570998452,9.22636560737001,9.22636560737001));
#47077=CARTESIAN_POINT('Ctrl Pts',(26.796570998452,0.,9.22636560737002));
#47078=CARTESIAN_POINT('Ctrl Pts',(26.796570998452,-9.22636560737001,9.22636560737001));
#47079=CARTESIAN_POINT('Ctrl Pts',(26.796570998452,-9.22636560737002,0.));
#47080=CARTESIAN_POINT('Ctrl Pts',(26.796570998452,-9.22636560737001,-9.22636560737001));
#47081=CARTESIAN_POINT('Ctrl Pts',(26.796570998452,0.,-9.22636560737002));
#47082=CARTESIAN_POINT('Ctrl Pts',(26.796570998452,9.22636560737001,-9.22636560737001));
#47083=CARTESIAN_POINT('Ctrl Pts',(26.796570998452,9.22636560737002,0.));
#47084=CARTESIAN_POINT('Ctrl Pts',(26.3874085880356,9.28597940593777,0.));
#47085=CARTESIAN_POINT('Ctrl Pts',(26.3874085880356,9.28597940593777,9.28597940593777));
#47086=CARTESIAN_POINT('Ctrl Pts',(26.3874085880356,0.,9.28597940593777));
#47087=CARTESIAN_POINT('Ctrl Pts',(26.3874085880356,-9.28597940593777,9.28597940593777));
#47088=CARTESIAN_POINT('Ctrl Pts',(26.3874085880356,-9.28597940593777,0.));
#47089=CARTESIAN_POINT('Ctrl Pts',(26.3874085880356,-9.28597940593777,-9.28597940593777));
#47090=CARTESIAN_POINT('Ctrl Pts',(26.3874085880356,0.,-9.28597940593777));
#47091=CARTESIAN_POINT('Ctrl Pts',(26.3874085880356,9.28597940593777,-9.28597940593777));
#47092=CARTESIAN_POINT('Ctrl Pts',(26.3874085880356,9.28597940593777,0.));
#47093=CARTESIAN_POINT('Ctrl Pts',(25.7667517823113,9.39604887090672,0.));
#47094=CARTESIAN_POINT('Ctrl Pts',(25.7667517823113,9.39604887090672,9.39604887090672));
#47095=CARTESIAN_POINT('Ctrl Pts',(25.7667517823113,0.,9.39604887090672));
#47096=CARTESIAN_POINT('Ctrl Pts',(25.7667517823113,-9.39604887090672,9.39604887090672));
#47097=CARTESIAN_POINT('Ctrl Pts',(25.7667517823113,-9.39604887090672,0.));
#47098=CARTESIAN_POINT('Ctrl Pts',(25.7667517823113,-9.39604887090672,-9.39604887090672));
#47099=CARTESIAN_POINT('Ctrl Pts',(25.7667517823113,0.,-9.39604887090672));
#47100=CARTESIAN_POINT('Ctrl Pts',(25.7667517823113,9.39604887090672,-9.39604887090672));
#47101=CARTESIAN_POINT('Ctrl Pts',(25.7667517823113,9.39604887090672,0.));
#47102=CARTESIAN_POINT('Ctrl Pts',(24.9253466419639,9.58420457526839,0.));
#47103=CARTESIAN_POINT('Ctrl Pts',(24.9253466419639,9.58420457526839,9.58420457526839));
#47104=CARTESIAN_POINT('Ctrl Pts',(24.9253466419639,0.,9.58420457526839));
#47105=CARTESIAN_POINT('Ctrl Pts',(24.9253466419639,-9.58420457526839,9.58420457526839));
#47106=CARTESIAN_POINT('Ctrl Pts',(24.9253466419639,-9.58420457526839,0.));
#47107=CARTESIAN_POINT('Ctrl Pts',(24.9253466419639,-9.58420457526839,-9.58420457526839));
#47108=CARTESIAN_POINT('Ctrl Pts',(24.9253466419639,0.,-9.58420457526839));
#47109=CARTESIAN_POINT('Ctrl Pts',(24.9253466419639,9.58420457526839,-9.58420457526839));
#47110=CARTESIAN_POINT('Ctrl Pts',(24.9253466419639,9.58420457526839,0.));
#47111=CARTESIAN_POINT('Ctrl Pts',(23.8505404645239,9.89058631634017,0.));
#47112=CARTESIAN_POINT('Ctrl Pts',(23.8505404645239,9.89058631634017,9.89058631634017));
#47113=CARTESIAN_POINT('Ctrl Pts',(23.8505404645239,0.,9.89058631634017));
#47114=CARTESIAN_POINT('Ctrl Pts',(23.8505404645239,-9.89058631634017,9.89058631634017));
#47115=CARTESIAN_POINT('Ctrl Pts',(23.8505404645239,-9.89058631634017,0.));
#47116=CARTESIAN_POINT('Ctrl Pts',(23.8505404645239,-9.89058631634017,-9.89058631634017));
#47117=CARTESIAN_POINT('Ctrl Pts',(23.8505404645239,0.,-9.89058631634017));
#47118=CARTESIAN_POINT('Ctrl Pts',(23.8505404645239,9.89058631634017,-9.89058631634017));
#47119=CARTESIAN_POINT('Ctrl Pts',(23.8505404645239,9.89058631634017,0.));
#47120=CARTESIAN_POINT('Ctrl Pts',(22.7532142104752,10.273481509771,0.));
#47121=CARTESIAN_POINT('Ctrl Pts',(22.7532142104752,10.273481509771,10.273481509771));
#47122=CARTESIAN_POINT('Ctrl Pts',(22.7532142104752,0.,10.273481509771));
#47123=CARTESIAN_POINT('Ctrl Pts',(22.7532142104752,-10.273481509771,10.273481509771));
#47124=CARTESIAN_POINT('Ctrl Pts',(22.7532142104752,-10.273481509771,0.));
#47125=CARTESIAN_POINT('Ctrl Pts',(22.7532142104752,-10.273481509771,-10.273481509771));
#47126=CARTESIAN_POINT('Ctrl Pts',(22.7532142104752,0.,-10.273481509771));
#47127=CARTESIAN_POINT('Ctrl Pts',(22.7532142104752,10.273481509771,-10.273481509771));
#47128=CARTESIAN_POINT('Ctrl Pts',(22.7532142104752,10.273481509771,0.));
#47129=CARTESIAN_POINT('Ctrl Pts',(21.6347255505832,10.7430346646081,0.));
#47130=CARTESIAN_POINT('Ctrl Pts',(21.6347255505832,10.7430346646081,10.7430346646081));
#47131=CARTESIAN_POINT('Ctrl Pts',(21.6347255505832,0.,10.7430346646081));
#47132=CARTESIAN_POINT('Ctrl Pts',(21.6347255505832,-10.7430346646081,10.7430346646081));
#47133=CARTESIAN_POINT('Ctrl Pts',(21.6347255505832,-10.7430346646081,0.));
#47134=CARTESIAN_POINT('Ctrl Pts',(21.6347255505832,-10.7430346646081,-10.7430346646081));
#47135=CARTESIAN_POINT('Ctrl Pts',(21.6347255505832,0.,-10.7430346646081));
#47136=CARTESIAN_POINT('Ctrl Pts',(21.6347255505832,10.7430346646081,-10.7430346646081));
#47137=CARTESIAN_POINT('Ctrl Pts',(21.6347255505832,10.7430346646081,0.));
#47138=CARTESIAN_POINT('Ctrl Pts',(20.4975894383762,11.3145134298179,0.));
#47139=CARTESIAN_POINT('Ctrl Pts',(20.4975894383762,11.3145134298179,11.3145134298179));
#47140=CARTESIAN_POINT('Ctrl Pts',(20.4975894383762,0.,11.3145134298179));
#47141=CARTESIAN_POINT('Ctrl Pts',(20.4975894383762,-11.3145134298179,11.3145134298179));
#47142=CARTESIAN_POINT('Ctrl Pts',(20.4975894383762,-11.3145134298179,0.));
#47143=CARTESIAN_POINT('Ctrl Pts',(20.4975894383762,-11.3145134298179,-11.3145134298179));
#47144=CARTESIAN_POINT('Ctrl Pts',(20.4975894383762,0.,-11.3145134298179));
#47145=CARTESIAN_POINT('Ctrl Pts',(20.4975894383762,11.3145134298179,-11.3145134298179));
#47146=CARTESIAN_POINT('Ctrl Pts',(20.4975894383762,11.3145134298179,0.));
#47147=CARTESIAN_POINT('Ctrl Pts',(19.3456615791409,12.0038530129696,0.));
#47148=CARTESIAN_POINT('Ctrl Pts',(19.3456615791409,12.0038530129696,12.0038530129696));
#47149=CARTESIAN_POINT('Ctrl Pts',(19.3456615791409,0.,12.0038530129696));
#47150=CARTESIAN_POINT('Ctrl Pts',(19.3456615791409,-12.0038530129696,12.0038530129696));
#47151=CARTESIAN_POINT('Ctrl Pts',(19.3456615791409,-12.0038530129696,0.));
#47152=CARTESIAN_POINT('Ctrl Pts',(19.3456615791409,-12.0038530129696,-12.0038530129696));
#47153=CARTESIAN_POINT('Ctrl Pts',(19.3456615791409,0.,-12.0038530129696));
#47154=CARTESIAN_POINT('Ctrl Pts',(19.3456615791409,12.0038530129696,-12.0038530129696));
#47155=CARTESIAN_POINT('Ctrl Pts',(19.3456615791409,12.0038530129696,0.));
#47156=CARTESIAN_POINT('Ctrl Pts',(18.1843885347784,12.8237912132616,0.));
#47157=CARTESIAN_POINT('Ctrl Pts',(18.1843885347784,12.8237912132616,12.8237912132616));
#47158=CARTESIAN_POINT('Ctrl Pts',(18.1843885347784,0.,12.8237912132616));
#47159=CARTESIAN_POINT('Ctrl Pts',(18.1843885347784,-12.8237912132616,12.8237912132616));
#47160=CARTESIAN_POINT('Ctrl Pts',(18.1843885347784,-12.8237912132616,0.));
#47161=CARTESIAN_POINT('Ctrl Pts',(18.1843885347784,-12.8237912132616,-12.8237912132616));
#47162=CARTESIAN_POINT('Ctrl Pts',(18.1843885347784,0.,-12.8237912132616));
#47163=CARTESIAN_POINT('Ctrl Pts',(18.1843885347784,12.8237912132616,-12.8237912132616));
#47164=CARTESIAN_POINT('Ctrl Pts',(18.1843885347784,12.8237912132616,0.));
#47165=CARTESIAN_POINT('Ctrl Pts',(17.0210036637821,13.7799946040807,0.));
#47166=CARTESIAN_POINT('Ctrl Pts',(17.0210036637821,13.7799946040807,13.7799946040807));
#47167=CARTESIAN_POINT('Ctrl Pts',(17.0210036637821,0.,13.7799946040807));
#47168=CARTESIAN_POINT('Ctrl Pts',(17.0210036637821,-13.7799946040807,13.7799946040807));
#47169=CARTESIAN_POINT('Ctrl Pts',(17.0210036637821,-13.7799946040807,0.));
#47170=CARTESIAN_POINT('Ctrl Pts',(17.0210036637821,-13.7799946040807,-13.7799946040807));
#47171=CARTESIAN_POINT('Ctrl Pts',(17.0210036637821,0.,-13.7799946040807));
#47172=CARTESIAN_POINT('Ctrl Pts',(17.0210036637821,13.7799946040807,-13.7799946040807));
#47173=CARTESIAN_POINT('Ctrl Pts',(17.0210036637821,13.7799946040807,0.));
#47174=CARTESIAN_POINT('Ctrl Pts',(15.8649034353727,14.8662985491428,0.));
#47175=CARTESIAN_POINT('Ctrl Pts',(15.8649034353727,14.8662985491428,14.8662985491428));
#47176=CARTESIAN_POINT('Ctrl Pts',(15.8649034353727,0.,14.8662985491428));
#47177=CARTESIAN_POINT('Ctrl Pts',(15.8649034353727,-14.8662985491428,14.8662985491428));
#47178=CARTESIAN_POINT('Ctrl Pts',(15.8649034353727,-14.8662985491428,0.));
#47179=CARTESIAN_POINT('Ctrl Pts',(15.8649034353727,-14.8662985491428,-14.8662985491428));
#47180=CARTESIAN_POINT('Ctrl Pts',(15.8649034353727,0.,-14.8662985491428));
#47181=CARTESIAN_POINT('Ctrl Pts',(15.8649034353727,14.8662985491428,-14.8662985491428));
#47182=CARTESIAN_POINT('Ctrl Pts',(15.8649034353727,14.8662985491428,0.));
#47183=CARTESIAN_POINT('Ctrl Pts',(14.7267277676362,16.0674034956045,0.));
#47184=CARTESIAN_POINT('Ctrl Pts',(14.7267277676362,16.0674034956045,16.0674034956045));
#47185=CARTESIAN_POINT('Ctrl Pts',(14.7267277676362,0.,16.0674034956045));
#47186=CARTESIAN_POINT('Ctrl Pts',(14.7267277676362,-16.0674034956045,16.0674034956045));
#47187=CARTESIAN_POINT('Ctrl Pts',(14.7267277676362,-16.0674034956045,0.));
#47188=CARTESIAN_POINT('Ctrl Pts',(14.7267277676362,-16.0674034956045,-16.0674034956045));
#47189=CARTESIAN_POINT('Ctrl Pts',(14.7267277676362,0.,-16.0674034956045));
#47190=CARTESIAN_POINT('Ctrl Pts',(14.7267277676362,16.0674034956045,-16.0674034956045));
#47191=CARTESIAN_POINT('Ctrl Pts',(14.7267277676362,16.0674034956045,0.));
#47192=CARTESIAN_POINT('Ctrl Pts',(13.6172459538847,17.362757468191,0.));
#47193=CARTESIAN_POINT('Ctrl Pts',(13.6172459538847,17.362757468191,17.362757468191));
#47194=CARTESIAN_POINT('Ctrl Pts',(13.6172459538847,0.,17.362757468191));
#47195=CARTESIAN_POINT('Ctrl Pts',(13.6172459538847,-17.362757468191,17.362757468191));
#47196=CARTESIAN_POINT('Ctrl Pts',(13.6172459538847,-17.362757468191,0.));
#47197=CARTESIAN_POINT('Ctrl Pts',(13.6172459538847,-17.362757468191,-17.362757468191));
#47198=CARTESIAN_POINT('Ctrl Pts',(13.6172459538847,0.,-17.362757468191));
#47199=CARTESIAN_POINT('Ctrl Pts',(13.6172459538847,17.362757468191,-17.362757468191));
#47200=CARTESIAN_POINT('Ctrl Pts',(13.6172459538847,17.362757468191,0.));
#47201=CARTESIAN_POINT('Ctrl Pts',(12.5462580187496,18.7300247619529,0.));
#47202=CARTESIAN_POINT('Ctrl Pts',(12.5462580187496,18.7300247619529,18.7300247619529));
#47203=CARTESIAN_POINT('Ctrl Pts',(12.5462580187496,0.,18.7300247619529));
#47204=CARTESIAN_POINT('Ctrl Pts',(12.5462580187496,-18.7300247619529,18.7300247619529));
#47205=CARTESIAN_POINT('Ctrl Pts',(12.5462580187496,-18.7300247619529,0.));
#47206=CARTESIAN_POINT('Ctrl Pts',(12.5462580187496,-18.7300247619529,-18.7300247619529));
#47207=CARTESIAN_POINT('Ctrl Pts',(12.5462580187496,0.,-18.7300247619529));
#47208=CARTESIAN_POINT('Ctrl Pts',(12.5462580187496,18.7300247619529,-18.7300247619529));
#47209=CARTESIAN_POINT('Ctrl Pts',(12.5462580187496,18.7300247619529,0.));
#47210=CARTESIAN_POINT('Ctrl Pts',(11.5215838208076,20.1483844597128,0.));
#47211=CARTESIAN_POINT('Ctrl Pts',(11.5215838208076,20.1483844597128,20.1483844597128));
#47212=CARTESIAN_POINT('Ctrl Pts',(11.5215838208076,0.,20.1483844597128));
#47213=CARTESIAN_POINT('Ctrl Pts',(11.5215838208076,-20.1483844597128,20.1483844597128));
#47214=CARTESIAN_POINT('Ctrl Pts',(11.5215838208076,-20.1483844597128,0.));
#47215=CARTESIAN_POINT('Ctrl Pts',(11.5215838208076,-20.1483844597128,-20.1483844597128));
#47216=CARTESIAN_POINT('Ctrl Pts',(11.5215838208076,0.,-20.1483844597128));
#47217=CARTESIAN_POINT('Ctrl Pts',(11.5215838208076,20.1483844597128,-20.1483844597128));
#47218=CARTESIAN_POINT('Ctrl Pts',(11.5215838208076,20.1483844597128,0.));
#47219=CARTESIAN_POINT('Ctrl Pts',(10.5477031262524,21.602527086122,0.));
#47220=CARTESIAN_POINT('Ctrl Pts',(10.5477031262524,21.602527086122,21.602527086122));
#47221=CARTESIAN_POINT('Ctrl Pts',(10.5477031262524,0.,21.602527086122));
#47222=CARTESIAN_POINT('Ctrl Pts',(10.5477031262524,-21.602527086122,21.602527086122));
#47223=CARTESIAN_POINT('Ctrl Pts',(10.5477031262524,-21.602527086122,0.));
#47224=CARTESIAN_POINT('Ctrl Pts',(10.5477031262524,-21.602527086122,-21.602527086122));
#47225=CARTESIAN_POINT('Ctrl Pts',(10.5477031262524,0.,-21.602527086122));
#47226=CARTESIAN_POINT('Ctrl Pts',(10.5477031262524,21.602527086122,-21.602527086122));
#47227=CARTESIAN_POINT('Ctrl Pts',(10.5477031262524,21.602527086122,0.));
#47228=CARTESIAN_POINT('Ctrl Pts',(9.62553662153839,23.0838998256659,0.));
#47229=CARTESIAN_POINT('Ctrl Pts',(9.62553662153839,23.0838998256659,23.0838998256659));
#47230=CARTESIAN_POINT('Ctrl Pts',(9.62553662153839,0.,23.0838998256659));
#47231=CARTESIAN_POINT('Ctrl Pts',(9.62553662153839,-23.0838998256659,23.0838998256659));
#47232=CARTESIAN_POINT('Ctrl Pts',(9.62553662153839,-23.0838998256659,0.));
#47233=CARTESIAN_POINT('Ctrl Pts',(9.62553662153839,-23.0838998256659,-23.0838998256659));
#47234=CARTESIAN_POINT('Ctrl Pts',(9.62553662153839,0.,-23.0838998256659));
#47235=CARTESIAN_POINT('Ctrl Pts',(9.62553662153839,23.0838998256659,-23.0838998256659));
#47236=CARTESIAN_POINT('Ctrl Pts',(9.62553662153839,23.0838998256659,0.));
#47237=CARTESIAN_POINT('Ctrl Pts',(8.75359166551105,24.5886478127263,0.));
#47238=CARTESIAN_POINT('Ctrl Pts',(8.75359166551105,24.5886478127262,24.5886478127262));
#47239=CARTESIAN_POINT('Ctrl Pts',(8.75359166551105,0.,24.5886478127263));
#47240=CARTESIAN_POINT('Ctrl Pts',(8.75359166551105,-24.5886478127262,24.5886478127262));
#47241=CARTESIAN_POINT('Ctrl Pts',(8.75359166551105,-24.5886478127263,0.));
#47242=CARTESIAN_POINT('Ctrl Pts',(8.75359166551105,-24.5886478127262,-24.5886478127262));
#47243=CARTESIAN_POINT('Ctrl Pts',(8.75359166551105,0.,-24.5886478127263));
#47244=CARTESIAN_POINT('Ctrl Pts',(8.75359166551105,24.5886478127262,-24.5886478127262));
#47245=CARTESIAN_POINT('Ctrl Pts',(8.75359166551105,24.5886478127263,0.));
#47246=CARTESIAN_POINT('Ctrl Pts',(7.92870053877921,26.1164647205758,0.));
#47247=CARTESIAN_POINT('Ctrl Pts',(7.92870053877921,26.1164647205758,26.1164647205758));
#47248=CARTESIAN_POINT('Ctrl Pts',(7.92870053877921,0.,26.1164647205758));
#47249=CARTESIAN_POINT('Ctrl Pts',(7.92870053877921,-26.1164647205758,26.1164647205758));
#47250=CARTESIAN_POINT('Ctrl Pts',(7.92870053877921,-26.1164647205758,0.));
#47251=CARTESIAN_POINT('Ctrl Pts',(7.92870053877921,-26.1164647205758,-26.1164647205758));
#47252=CARTESIAN_POINT('Ctrl Pts',(7.92870053877921,0.,-26.1164647205758));
#47253=CARTESIAN_POINT('Ctrl Pts',(7.92870053877921,26.1164647205758,-26.1164647205758));
#47254=CARTESIAN_POINT('Ctrl Pts',(7.92870053877921,26.1164647205758,0.));
#47255=CARTESIAN_POINT('Ctrl Pts',(7.14689760675259,27.6690738550248,0.));
#47256=CARTESIAN_POINT('Ctrl Pts',(7.14689760675259,27.6690738550248,27.6690738550248));
#47257=CARTESIAN_POINT('Ctrl Pts',(7.1468976067526,0.,27.6690738550248));
#47258=CARTESIAN_POINT('Ctrl Pts',(7.1468976067526,-27.6690738550248,27.6690738550248));
#47259=CARTESIAN_POINT('Ctrl Pts',(7.1468976067526,-27.6690738550248,0.));
#47260=CARTESIAN_POINT('Ctrl Pts',(7.1468976067526,-27.6690738550248,-27.6690738550248));
#47261=CARTESIAN_POINT('Ctrl Pts',(7.1468976067526,0.,-27.6690738550248));
#47262=CARTESIAN_POINT('Ctrl Pts',(7.14689760675259,27.6690738550248,-27.6690738550248));
#47263=CARTESIAN_POINT('Ctrl Pts',(7.14689760675259,27.6690738550248,0.));
#47264=CARTESIAN_POINT('Ctrl Pts',(6.40416480933221,29.248955946805,0.));
#47265=CARTESIAN_POINT('Ctrl Pts',(6.40416480933221,29.248955946805,29.248955946805));
#47266=CARTESIAN_POINT('Ctrl Pts',(6.40416480933221,0.,29.248955946805));
#47267=CARTESIAN_POINT('Ctrl Pts',(6.40416480933221,-29.248955946805,29.248955946805));
#47268=CARTESIAN_POINT('Ctrl Pts',(6.40416480933221,-29.248955946805,0.));
#47269=CARTESIAN_POINT('Ctrl Pts',(6.40416480933221,-29.248955946805,-29.248955946805));
#47270=CARTESIAN_POINT('Ctrl Pts',(6.40416480933221,0.,-29.248955946805));
#47271=CARTESIAN_POINT('Ctrl Pts',(6.40416480933221,29.248955946805,-29.248955946805));
#47272=CARTESIAN_POINT('Ctrl Pts',(6.40416480933221,29.248955946805,0.));
#47273=CARTESIAN_POINT('Ctrl Pts',(5.69731071687183,30.8577859595634,0.));
#47274=CARTESIAN_POINT('Ctrl Pts',(5.69731071687183,30.8577859595634,30.8577859595634));
#47275=CARTESIAN_POINT('Ctrl Pts',(5.69731071687183,0.,30.8577859595634));
#47276=CARTESIAN_POINT('Ctrl Pts',(5.69731071687183,-30.8577859595634,30.8577859595634));
#47277=CARTESIAN_POINT('Ctrl Pts',(5.69731071687183,-30.8577859595634,0.));
#47278=CARTESIAN_POINT('Ctrl Pts',(5.69731071687183,-30.8577859595634,-30.8577859595634));
#47279=CARTESIAN_POINT('Ctrl Pts',(5.69731071687183,0.,-30.8577859595634));
#47280=CARTESIAN_POINT('Ctrl Pts',(5.69731071687183,30.8577859595634,-30.8577859595634));
#47281=CARTESIAN_POINT('Ctrl Pts',(5.69731071687183,30.8577859595634,0.));
#47282=CARTESIAN_POINT('Ctrl Pts',(5.02401496259691,32.4964011792533,0.));
#47283=CARTESIAN_POINT('Ctrl Pts',(5.02401496259691,32.4964011792533,32.4964011792533));
#47284=CARTESIAN_POINT('Ctrl Pts',(5.02401496259691,0.,32.4964011792533));
#47285=CARTESIAN_POINT('Ctrl Pts',(5.02401496259691,-32.4964011792533,32.4964011792533));
#47286=CARTESIAN_POINT('Ctrl Pts',(5.02401496259691,-32.4964011792533,0.));
#47287=CARTESIAN_POINT('Ctrl Pts',(5.02401496259691,-32.4964011792533,-32.4964011792533));
#47288=CARTESIAN_POINT('Ctrl Pts',(5.02401496259691,0.,-32.4964011792533));
#47289=CARTESIAN_POINT('Ctrl Pts',(5.02401496259691,32.4964011792533,-32.4964011792533));
#47290=CARTESIAN_POINT('Ctrl Pts',(5.02401496259691,32.4964011792533,0.));
#47291=CARTESIAN_POINT('Ctrl Pts',(4.38267277981043,34.1651137045816,0.));
#47292=CARTESIAN_POINT('Ctrl Pts',(4.38267277981043,34.1651137045815,34.1651137045815));
#47293=CARTESIAN_POINT('Ctrl Pts',(4.38267277981043,0.,34.1651137045816));
#47294=CARTESIAN_POINT('Ctrl Pts',(4.38267277981043,-34.1651137045815,34.1651137045815));
#47295=CARTESIAN_POINT('Ctrl Pts',(4.38267277981043,-34.1651137045816,0.));
#47296=CARTESIAN_POINT('Ctrl Pts',(4.38267277981043,-34.1651137045815,-34.1651137045815));
#47297=CARTESIAN_POINT('Ctrl Pts',(4.38267277981043,0.,-34.1651137045816));
#47298=CARTESIAN_POINT('Ctrl Pts',(4.38267277981043,34.1651137045815,-34.1651137045815));
#47299=CARTESIAN_POINT('Ctrl Pts',(4.38267277981043,34.1651137045816,0.));
#47300=CARTESIAN_POINT('Ctrl Pts',(3.89437496746067,35.5241326822989,0.));
#47301=CARTESIAN_POINT('Ctrl Pts',(3.89437496746067,35.5241326822989,35.5241326822989));
#47302=CARTESIAN_POINT('Ctrl Pts',(3.89437496746067,0.,35.5241326822989));
#47303=CARTESIAN_POINT('Ctrl Pts',(3.89437496746066,-35.5241326822989,35.5241326822989));
#47304=CARTESIAN_POINT('Ctrl Pts',(3.89437496746066,-35.5241326822989,0.));
#47305=CARTESIAN_POINT('Ctrl Pts',(3.89437496746066,-35.5241326822989,-35.5241326822989));
#47306=CARTESIAN_POINT('Ctrl Pts',(3.89437496746067,0.,-35.5241326822989));
#47307=CARTESIAN_POINT('Ctrl Pts',(3.89437496746067,35.5241326822989,-35.5241326822989));
#47308=CARTESIAN_POINT('Ctrl Pts',(3.89437496746067,35.5241326822989,0.));
#47309=CARTESIAN_POINT('Ctrl Pts',(3.5418673953418,36.5568488026925,0.));
#47310=CARTESIAN_POINT('Ctrl Pts',(3.5418673953418,36.5568488026925,36.5568488026925));
#47311=CARTESIAN_POINT('Ctrl Pts',(3.5418673953418,0.,36.5568488026925));
#47312=CARTESIAN_POINT('Ctrl Pts',(3.5418673953418,-36.5568488026925,36.5568488026925));
#47313=CARTESIAN_POINT('Ctrl Pts',(3.5418673953418,-36.5568488026925,0.));
#47314=CARTESIAN_POINT('Ctrl Pts',(3.5418673953418,-36.5568488026925,-36.5568488026925));
#47315=CARTESIAN_POINT('Ctrl Pts',(3.5418673953418,0.,-36.5568488026925));
#47316=CARTESIAN_POINT('Ctrl Pts',(3.5418673953418,36.5568488026925,-36.5568488026925));
#47317=CARTESIAN_POINT('Ctrl Pts',(3.5418673953418,36.5568488026925,0.));
#47318=CARTESIAN_POINT('Ctrl Pts',(3.31294245015623,37.2512891119684,0.));
#47319=CARTESIAN_POINT('Ctrl Pts',(3.31294245015623,37.2512891119684,37.2512891119684));
#47320=CARTESIAN_POINT('Ctrl Pts',(3.31294245015623,0.,37.2512891119684));
#47321=CARTESIAN_POINT('Ctrl Pts',(3.31294245015623,-37.2512891119684,37.2512891119684));
#47322=CARTESIAN_POINT('Ctrl Pts',(3.31294245015623,-37.2512891119684,0.));
#47323=CARTESIAN_POINT('Ctrl Pts',(3.31294245015623,-37.2512891119684,-37.2512891119684));
#47324=CARTESIAN_POINT('Ctrl Pts',(3.31294245015623,0.,-37.2512891119684));
#47325=CARTESIAN_POINT('Ctrl Pts',(3.31294245015623,37.2512891119684,-37.2512891119684));
#47326=CARTESIAN_POINT('Ctrl Pts',(3.31294245015623,37.2512891119684,0.));
#47327=CARTESIAN_POINT('Ctrl Pts',(3.2,37.6,0.));
#47328=CARTESIAN_POINT('Ctrl Pts',(3.2,37.6,37.6));
#47329=CARTESIAN_POINT('Ctrl Pts',(3.2,0.,37.6));
#47330=CARTESIAN_POINT('Ctrl Pts',(3.2,-37.6,37.6));
#47331=CARTESIAN_POINT('Ctrl Pts',(3.2,-37.6,0.));
#47332=CARTESIAN_POINT('Ctrl Pts',(3.2,-37.6,-37.6));
#47333=CARTESIAN_POINT('Ctrl Pts',(3.2,0.,-37.6));
#47334=CARTESIAN_POINT('Ctrl Pts',(3.2,37.6,-37.6));
#47335=CARTESIAN_POINT('Ctrl Pts',(3.2,37.6,0.));
#47336=CARTESIAN_POINT('',(11.1111871729018,20.775057671175,0.));
#47337=CARTESIAN_POINT('',(23.5150942984749,10.0178765673373,0.));
#47338=CARTESIAN_POINT('Ctrl Pts',(11.1111871729018,20.775057671175,0.));
#47339=CARTESIAN_POINT('Ctrl Pts',(11.1948689745378,20.6509039312648,0.));
#47340=CARTESIAN_POINT('Ctrl Pts',(11.4755829737079,20.2377304421578,0.));
#47341=CARTESIAN_POINT('Ctrl Pts',(11.9616798526703,19.5410850083761,0.));
#47342=CARTESIAN_POINT('Ctrl Pts',(12.6687572718921,18.5736371717314,0.));
#47343=CARTESIAN_POINT('Ctrl Pts',(13.6172459538847,17.362757468191,0.));
#47344=CARTESIAN_POINT('Ctrl Pts',(14.7267277676362,16.0674034956045,0.));
#47345=CARTESIAN_POINT('Ctrl Pts',(15.8649034353727,14.8662985491428,0.));
#47346=CARTESIAN_POINT('Ctrl Pts',(17.0210036637821,13.7799946040807,0.));
#47347=CARTESIAN_POINT('Ctrl Pts',(18.1843885347784,12.8237912132616,0.));
#47348=CARTESIAN_POINT('Ctrl Pts',(19.3456615791409,12.0038530129696,0.));
#47349=CARTESIAN_POINT('Ctrl Pts',(20.4975894383762,11.3145134298179,0.));
#47350=CARTESIAN_POINT('Ctrl Pts',(21.5658679574808,10.7776397148383,0.));
#47351=CARTESIAN_POINT('Ctrl Pts',(22.3939741610711,10.4247254993888,0.));
#47352=CARTESIAN_POINT('Ctrl Pts',(22.9904947752284,10.1993474973472,0.));
#47353=CARTESIAN_POINT('Ctrl Pts',(23.3627187655144,10.0693419338606,0.));
#47354=CARTESIAN_POINT('Ctrl Pts',(23.5150942984749,10.0178765673373,0.));
#47355=CARTESIAN_POINT('',(3.2,37.5892271801377,0.899999999999997));
#47356=CARTESIAN_POINT('Ctrl Pts',(11.1111871729018,20.775057671175,4.68375338513738E-16));
#47357=CARTESIAN_POINT('Ctrl Pts',(10.8408519694691,21.1761380241238,0.104779981433169));
#47358=CARTESIAN_POINT('Ctrl Pts',(10.5713373596261,21.5873718624941,0.200619231177909));
#47359=CARTESIAN_POINT('Ctrl Pts',(10.2958331164458,22.0215373473783,0.285388879148048));
#47360=CARTESIAN_POINT('Ctrl Pts',(9.71429910913615,22.9379733025773,0.464320544639868));
#47361=CARTESIAN_POINT('Ctrl Pts',(9.09451803370737,23.9735296287181,0.601171200169489));
#47362=CARTESIAN_POINT('Ctrl Pts',(8.43051482342505,25.1910871092345,0.711313606025344));
#47363=CARTESIAN_POINT('Ctrl Pts',(7.97885593463559,26.019276868217,0.786233118261289));
#47364=CARTESIAN_POINT('Ctrl Pts',(7.52255926008875,26.9071640425416,0.845450887989925));
#47365=CARTESIAN_POINT('Ctrl Pts',(7.10363554125515,27.7707039763416,0.894013240723397));
#47366=CARTESIAN_POINT('Ctrl Pts',(6.56327799557425,28.8845590727416,0.956652409994373));
#47367=CARTESIAN_POINT('Ctrl Pts',(6.08559840027184,29.9474764438374,0.961734555176139));
#47368=CARTESIAN_POINT('Ctrl Pts',(5.6170867083501,31.0600288611027,0.951686011835693));
#47369=CARTESIAN_POINT('Ctrl Pts',(5.04102956507642,32.4279643433598,0.939330855559837));
#47370=CARTESIAN_POINT('Ctrl Pts',(4.5010282050509,33.8266980954716,0.9));
#47371=CARTESIAN_POINT('Ctrl Pts',(4.,35.2340925362767,0.9));
#47372=CARTESIAN_POINT('Ctrl Pts',(3.72183418896969,36.0154637487543,0.9));
#47373=CARTESIAN_POINT('Ctrl Pts',(3.45538353518196,36.8005021100802,0.9));
#47374=CARTESIAN_POINT('Ctrl Pts',(3.2,37.5892271801377,0.9));
#47375=CARTESIAN_POINT('',(3.2,34.2572188230213,15.4984824583453));
#47376=CARTESIAN_POINT('Origin',(3.2,0.,0.));
#47377=CARTESIAN_POINT('',(15.,15.4997804972258,3.06084967694561));
#47378=CARTESIAN_POINT('Ctrl Pts',(3.2,34.2572188230213,15.4984824583453));
#47379=CARTESIAN_POINT('Ctrl Pts',(3.56152274835418,33.2512647221728,15.0140404956913));
#47380=CARTESIAN_POINT('Ctrl Pts',(3.95224584525374,32.2350723867225,14.5182294335367));
#47381=CARTESIAN_POINT('Ctrl Pts',(4.78767430123722,30.1964778916196,13.5611205349435));
#47382=CARTESIAN_POINT('Ctrl Pts',(5.21513946232063,29.2140021162723,13.1170571755916));
#47383=CARTESIAN_POINT('Ctrl Pts',(6.79548775402531,25.836168792914,11.5276347803711));
#47384=CARTESIAN_POINT('Ctrl Pts',(7.94016295939284,23.9218153262741,10.3912034265391));
#47385=CARTESIAN_POINT('Ctrl Pts',(9.46271935275732,21.5720888915642,8.90666589894935));
#47386=CARTESIAN_POINT('Ctrl Pts',(10.1385443659094,20.6585071274117,8.21538544795477));
#47387=CARTESIAN_POINT('Ctrl Pts',(11.5967860400733,18.9239680936141,6.63484019277982));
#47388=CARTESIAN_POINT('Ctrl Pts',(12.3997356677083,18.0341377754366,5.78619942648488));
#47389=CARTESIAN_POINT('Ctrl Pts',(13.6850585208097,16.7156528118604,4.43617268008764));
#47390=CARTESIAN_POINT('Ctrl Pts',(14.3457395898608,16.0917172728797,3.72217451879281));
#47391=CARTESIAN_POINT('Ctrl Pts',(15.,15.4997804972258,3.06084967694561));
#47392=CARTESIAN_POINT('',(15.,14.914658515121,5.2120013031819));
#47393=CARTESIAN_POINT('Ctrl Pts',(15.,15.4997804972258,3.06084967694561));
#47394=CARTESIAN_POINT('Ctrl Pts',(15.,15.3557790740222,3.79005584076192));
#47395=CARTESIAN_POINT('Ctrl Pts',(15.,15.1603519478033,4.50892518429681));
#47396=CARTESIAN_POINT('Ctrl Pts',(15.,14.914658515121,5.2120013031819));
#47397=CARTESIAN_POINT('',(3.2,33.4762280926097,17.1202264205697));
#47398=CARTESIAN_POINT('Ctrl Pts',(15.,14.914658515121,5.2120013031819));
#47399=CARTESIAN_POINT('Ctrl Pts',(14.4897165779508,15.3292352555695,5.70151627419433));
#47400=CARTESIAN_POINT('Ctrl Pts',(13.9833803026607,15.7672104557508,6.19304081265193));
#47401=CARTESIAN_POINT('Ctrl Pts',(13.4460287676664,16.2769406731723,6.70286203098642));
#47402=CARTESIAN_POINT('Ctrl Pts',(12.8282655681005,16.8629491788207,7.28897515532747));
#47403=CARTESIAN_POINT('Ctrl Pts',(12.1555414089416,17.5447613593883,7.96966355059842));
#47404=CARTESIAN_POINT('Ctrl Pts',(11.5904908073494,18.1719403594245,8.53563819264853));
#47405=CARTESIAN_POINT('Ctrl Pts',(11.1143368259575,18.7004483852033,9.01257083977716));
#47406=CARTESIAN_POINT('Ctrl Pts',(10.6953158949575,19.2030248825086,9.42802203261975));
#47407=CARTESIAN_POINT('Ctrl Pts',(10.2957959918397,19.7169417339605,9.81194913646659));
#47408=CARTESIAN_POINT('Ctrl Pts',(10.0450888109627,20.0394354170716,10.0528715063325));
#47409=CARTESIAN_POINT('Ctrl Pts',(9.80235305585738,20.365996759971,10.2821249831681));
#47410=CARTESIAN_POINT('Ctrl Pts',(9.5601010623963,20.7052519349419,10.5098647441811));
#47411=CARTESIAN_POINT('Ctrl Pts',(9.36613602949014,20.9768849573855,10.6922102002816));
#47412=CARTESIAN_POINT('Ctrl Pts',(9.15248571309183,21.2835959554689,10.8921233525791));
#47413=CARTESIAN_POINT('Ctrl Pts',(8.89022359845111,21.6785168619804,11.1382095281044));
#47414=CARTESIAN_POINT('Ctrl Pts',(8.39222406123487,22.4284171247353,11.605493190843));
#47415=CARTESIAN_POINT('Ctrl Pts',(7.76643777383336,23.4350262792015,12.1927153023679));
#47416=CARTESIAN_POINT('Ctrl Pts',(7.10363554123529,24.6326419147479,12.8547349765861));
#47417=CARTESIAN_POINT('Ctrl Pts',(6.23550018249919,26.2012734435196,13.7218453439034));
#47418=CARTESIAN_POINT('Ctrl Pts',(5.31040885825212,28.1564047394871,14.6002024056743));
#47419=CARTESIAN_POINT('Ctrl Pts',(4.46416616907914,30.2050861982221,15.5549203579907));
#47420=CARTESIAN_POINT('Ctrl Pts',(4.30741751126835,30.5845613453012,15.7317617765674));
#47421=CARTESIAN_POINT('Ctrl Pts',(4.15262292090198,30.9680620164154,15.9123572985204));
#47422=CARTESIAN_POINT('Ctrl Pts',(4.,31.3543250987725,16.098371795166));
#47423=CARTESIAN_POINT('Ctrl Pts',(3.7243497328338,32.0519498147649,16.4343301518407));
#47424=CARTESIAN_POINT('Ctrl Pts',(3.45587123478804,32.7642543119943,16.7773579185688));
#47425=CARTESIAN_POINT('Ctrl Pts',(3.2,33.4762280926097,17.1202264205697));
#47426=CARTESIAN_POINT('',(3.2,24.1401481407882,28.8273003894017));
#47427=CARTESIAN_POINT('Origin',(3.2,0.,0.));
#47428=CARTESIAN_POINT('Ctrl Pts',(3.2,24.1401481407882,28.8273003894017));
#47429=CARTESIAN_POINT('Ctrl Pts',(3.4517402012824,23.6554016427293,28.219447507015));
#47430=CARTESIAN_POINT('Ctrl Pts',(3.71840125357238,23.1649351015154,27.6044219173822));
#47431=CARTESIAN_POINT('Ctrl Pts',(4.,22.6717457083367,26.9859819793801));
#47432=CARTESIAN_POINT('Ctrl Pts',(4.62816481487921,21.5715837658681,25.6064225385185));
#47433=CARTESIAN_POINT('Ctrl Pts',(5.32582967773128,20.4257443465207,24.2662709294862));
#47434=CARTESIAN_POINT('Ctrl Pts',(6.03866109153771,19.4167181280198,22.9927130590511));
#47435=CARTESIAN_POINT('Ctrl Pts',(6.32798218739597,19.0071786974727,22.4758066046264));
#47436=CARTESIAN_POINT('Ctrl Pts',(6.6160411706376,18.6257941155792,21.9750548900751));
#47437=CARTESIAN_POINT('Ctrl Pts',(6.89476148100327,18.2850710138973,21.4951682830474));
#47438=CARTESIAN_POINT('Ctrl Pts',(7.65522892714578,17.3554336055655,20.185833695964));
#47439=CARTESIAN_POINT('Ctrl Pts',(8.3522670912656,16.6384040964243,19.1007390031585));
#47440=CARTESIAN_POINT('Ctrl Pts',(8.78926323660369,16.2240019202544,18.4274271814668));
#47441=CARTESIAN_POINT('Ctrl Pts',(8.99031958013673,16.0333407732816,18.1176450143445));
#47442=CARTESIAN_POINT('Ctrl Pts',(9.1827552232782,15.859968720011,17.8244630669136));
#47443=CARTESIAN_POINT('Ctrl Pts',(9.37496046323339,15.6959599143301,17.5328830843302));
#47444=CARTESIAN_POINT('Ctrl Pts',(9.48075233467205,15.6056876694659,17.3723942649893));
#47445=CARTESIAN_POINT('Ctrl Pts',(9.58626090989787,15.5184988415833,17.2127346999996));
#47446=CARTESIAN_POINT('Ctrl Pts',(9.69257910363365,15.433779824459,17.0518540733511));
#47447=CARTESIAN_POINT('Ctrl Pts',(10.0319880473342,15.1633238366068,16.5382606644157));
#47448=CARTESIAN_POINT('Ctrl Pts',(10.3788056747491,14.9187807821475,16.0114307331727));
#47449=CARTESIAN_POINT('Ctrl Pts',(10.7756849089348,14.6687048722873,15.4154473578682));
#47450=CARTESIAN_POINT('Ctrl Pts',(10.8890930409408,14.5972457498288,15.2451452723016));
#47451=CARTESIAN_POINT('Ctrl Pts',(11.057620352753,14.4933604902702,14.9923498534867));
#47452=CARTESIAN_POINT('Ctrl Pts',(11.2725125499177,14.3686609268079,14.6736882151435));
#47453=CARTESIAN_POINT('Ctrl Pts',(11.5968279597855,14.180464284174,14.1927639135076));
#47454=CARTESIAN_POINT('Ctrl Pts',(12.0255678846111,13.9481586925854,13.5614890403409));
#47455=CARTESIAN_POINT('Ctrl Pts',(12.532035905153,13.6869042147774,12.8549105632904));
#47456=CARTESIAN_POINT('Ctrl Pts',(13.0988763176265,13.3945074790411,12.0641059732044));
#47457=CARTESIAN_POINT('Ctrl Pts',(13.7495416915397,13.1167044041393,11.1526887031812));
#47458=CARTESIAN_POINT('Ctrl Pts',(14.4398764939332,12.8499149844562,10.2249013726919));
#47459=CARTESIAN_POINT('Ctrl Pts',(14.7901814035672,12.714534813517,9.75410306462509));
#47460=CARTESIAN_POINT('Ctrl Pts',(15.1459546150644,12.5820394706047,9.28856386081903));
#47461=CARTESIAN_POINT('Ctrl Pts',(15.4570717747561,12.4649063243577,8.89690991431743));
#47462=CARTESIAN_POINT('Ctrl Pts',(15.799823141116,12.3358631498765,8.46543282884673));
#47463=CARTESIAN_POINT('Ctrl Pts',(16.0676294503676,12.2436583506951,8.13029753852379));
#47464=CARTESIAN_POINT('Ctrl Pts',(16.3615307987862,12.1462490787105,7.7659519476552));
#47465=CARTESIAN_POINT('Ctrl Pts',(17.0296616033239,11.9248069668907,6.93767907967872));
#47466=CARTESIAN_POINT('Ctrl Pts',(17.7084691879561,11.7252415447452,6.11143371863158));
#47467=CARTESIAN_POINT('Ctrl Pts',(18.4207032016838,11.5097253054852,5.31931102580207));
#47468=CARTESIAN_POINT('Ctrl Pts',(18.8298642042877,11.3859165027133,4.8642559330424));
#47469=CARTESIAN_POINT('Ctrl Pts',(19.2113759273418,11.2794672006796,4.44103900795681));
#47470=CARTESIAN_POINT('Ctrl Pts',(19.5701113608397,11.1806982910754,4.04710221245386));
#47471=CARTESIAN_POINT('Ctrl Pts',(20.1215476022134,11.0288739905159,3.44155560187016));
#47472=CARTESIAN_POINT('Ctrl Pts',(20.6514912601619,10.888905473324,2.85828734179492));
#47473=CARTESIAN_POINT('Ctrl Pts',(21.3979544325339,10.6719534577984,2.10691159324049));
#47474=CARTESIAN_POINT('Ctrl Pts',(21.8015299361149,10.5546582955463,1.70068010409967));
#47475=CARTESIAN_POINT('Ctrl Pts',(22.2842895882516,10.4128463661915,1.22286894239258));
#47476=CARTESIAN_POINT('Ctrl Pts',(22.8110928915501,10.2470312028678,0.700625669077338));
#47477=CARTESIAN_POINT('Ctrl Pts',(23.0435286867255,10.1738703492856,0.470201847229612));
#47478=CARTESIAN_POINT('Ctrl Pts',(23.2793380077566,10.0975040749578,0.235994067598351));
#47479=CARTESIAN_POINT('Ctrl Pts',(23.5150942984749,10.0178765673373,2.74086309204336E-15));
#47480=CARTESIAN_POINT('Origin',(2.44847982464479,0.,-1.17996027893162E-15));
#47481=CARTESIAN_POINT('',(2.79695964929223,35.1047516110625,-15.9066327376731));
#47482=CARTESIAN_POINT('',(2.1,35.5189237522517,-16.106087528687));
#47483=CARTESIAN_POINT('Ctrl Pts',(2.09999999999999,35.5189237522517,-16.106087528687));
#47484=CARTESIAN_POINT('Ctrl Pts',(2.33231184614132,35.3808715864332,-16.0396051095574));
#47485=CARTESIAN_POINT('Ctrl Pts',(2.56464811456314,35.2428044741992,-15.9731154926135));
#47486=CARTESIAN_POINT('Ctrl Pts',(2.79695964929243,35.1047516110636,-15.9066327376736));
#47487=CARTESIAN_POINT('',(2.1,38.98961400168,-0.9));
#47488=CARTESIAN_POINT('Origin',(2.1,0.,0.));
#47489=CARTESIAN_POINT('',(2.79695964929243,38.5299176060057,-0.900000000000078));
#47490=CARTESIAN_POINT('Ctrl Pts',(2.79695964929245,38.5299176060072,-0.9));
#47491=CARTESIAN_POINT('Ctrl Pts',(2.56464811234863,38.6831447255779,-0.9));
#47492=CARTESIAN_POINT('Ctrl Pts',(2.33231184158428,38.8363876605392,-0.9));
#47493=CARTESIAN_POINT('Ctrl Pts',(2.09999999999999,38.98961400168,-0.9));
#47494=CARTESIAN_POINT('Origin',(2.79695964928958,0.,-2.35992055786324E-15));
#47495=CARTESIAN_POINT('Origin',(1.55,0.,0.));
#47496=CARTESIAN_POINT('',(2.6,38.98961400168,-0.899999999999993));
#47497=CARTESIAN_POINT('Ctrl Pts',(2.1,38.98961400168,-0.9));
#47498=CARTESIAN_POINT('Ctrl Pts',(2.26666666666667,38.98961400168,-0.9));
#47499=CARTESIAN_POINT('Ctrl Pts',(2.43346002867001,38.9896159908677,-0.899989754761565));
#47500=CARTESIAN_POINT('Ctrl Pts',(2.60034430332035,38.9896190555114,-0.899974049656302));
#47501=CARTESIAN_POINT('',(2.6,35.5189237522517,-16.106087528687));
#47502=CARTESIAN_POINT('Ctrl Pts',(2.59962081372057,35.5189106691499,-16.1061069197962));
#47503=CARTESIAN_POINT('Ctrl Pts',(2.43319306186644,35.5189185929367,-16.1060951831224));
#47504=CARTESIAN_POINT('Ctrl Pts',(2.26666666666667,35.5189237522517,-16.106087528687));
#47505=CARTESIAN_POINT('Ctrl Pts',(2.1,35.5189237522517,-16.106087528687));
#47506=CARTESIAN_POINT('',(6.,35.548403009865,-16.0409177869666));
#47507=CARTESIAN_POINT('Ctrl Pts',(2.6,35.5189237522517,-16.106087528687));
#47508=CARTESIAN_POINT('Ctrl Pts',(3.15786519714955,35.5189237522517,-16.106087528687));
#47509=CARTESIAN_POINT('Ctrl Pts',(3.71593098901213,35.5143077475111,-16.1162704800869));
#47510=CARTESIAN_POINT('Ctrl Pts',(4.82421019263741,35.5267242579696,-16.0888808412897));
#47511=CARTESIAN_POINT('Ctrl Pts',(5.40687161376251,35.548282527766,-16.0411847882857));
#47512=CARTESIAN_POINT('Ctrl Pts',(6.,35.548403009865,-16.0409177869666));
#47513=CARTESIAN_POINT('',(6.,34.7703877941326,-17.6640916167698));
#47514=CARTESIAN_POINT('Origin',(6.,0.,0.));
#47515=CARTESIAN_POINT('',(2.6,34.7379330218401,-17.7278314909114));
#47516=CARTESIAN_POINT('Ctrl Pts',(6.,34.7703877941326,-17.6640916167698));
#47517=CARTESIAN_POINT('Ctrl Pts',(5.46151291267476,34.7702417512009,-17.6643790908997));
#47518=CARTESIAN_POINT('Ctrl Pts',(4.90416494331291,34.7471941155784,-17.709679558335));
#47519=CARTESIAN_POINT('Ctrl Pts',(3.74812575287323,34.7329579415584,-17.7375836670634));
#47520=CARTESIAN_POINT('Ctrl Pts',(3.17396064416408,34.7379330218401,-17.7278314909114));
#47521=CARTESIAN_POINT('Ctrl Pts',(2.6,34.7379330218401,-17.7278314909114));
#47522=CARTESIAN_POINT('',(2.1,34.7379330218401,-17.7278314909114));
#47523=CARTESIAN_POINT('Ctrl Pts',(2.1,34.7379330218401,-17.7278314909114));
#47524=CARTESIAN_POINT('Ctrl Pts',(2.26666666666667,34.7379330218401,-17.7278314909114));
#47525=CARTESIAN_POINT('Ctrl Pts',(2.4335782958255,34.7379353669068,-17.727828473026));
#47526=CARTESIAN_POINT('Ctrl Pts',(2.60065276820886,34.7379392432415,-17.7278233384529));
#47527=CARTESIAN_POINT('',(2.1,25.0132750426772,-29.9221668941169));
#47528=CARTESIAN_POINT('Origin',(2.1,0.,0.));
#47529=CARTESIAN_POINT('',(2.6,25.0132750426772,-29.9221668941169));
#47530=CARTESIAN_POINT('Ctrl Pts',(2.59963671643924,25.0132558670369,-29.9221762868835));
#47531=CARTESIAN_POINT('Ctrl Pts',(2.43319919569241,25.013267470382,-29.9221706110259));
#47532=CARTESIAN_POINT('Ctrl Pts',(2.26666666666667,25.0132750426772,-29.9221668941169));
#47533=CARTESIAN_POINT('Ctrl Pts',(2.1,25.0132750426772,-29.9221668941169));
#47534=CARTESIAN_POINT('',(6.,25.0681110272506,-29.8762415562171));
#47535=CARTESIAN_POINT('Ctrl Pts',(2.6,25.0132750426772,-29.9221668941169));
#47536=CARTESIAN_POINT('Ctrl Pts',(3.15786555369928,25.0132750426772,-29.9221668941169));
#47537=CARTESIAN_POINT('Ctrl Pts',(3.71593170347639,25.0046979272054,-29.9293386252219));
#47538=CARTESIAN_POINT('Ctrl Pts',(4.82421093519821,25.027768809093,-29.9100486737611));
#47539=CARTESIAN_POINT('Ctrl Pts',(5.40687201153467,25.0678866292501,-29.8764298407435));
#47540=CARTESIAN_POINT('Ctrl Pts',(6.,25.0681110272506,-29.8762415562171));
#47541=CARTESIAN_POINT('',(6.,23.6628748086085,-31.0011024931715));
#47542=CARTESIAN_POINT('Origin',(6.,0.,0.));
#47543=CARTESIAN_POINT('',(2.6,23.6059783742347,-31.0444485374626));
#47544=CARTESIAN_POINT('Ctrl Pts',(6.,23.6628748086085,-31.0011024931715));
#47545=CARTESIAN_POINT('Ctrl Pts',(5.46151292711359,23.6626184981302,-31.0012981327543));
#47546=CARTESIAN_POINT('Ctrl Pts',(4.90416497508538,23.6221981620287,-31.0321124475678));
#47547=CARTESIAN_POINT('Ctrl Pts',(3.7481257854858,23.5972646702696,-31.0510763387916));
#47548=CARTESIAN_POINT('Ctrl Pts',(3.17396066044241,23.6059783742347,-31.0444485374626));
#47549=CARTESIAN_POINT('Ctrl Pts',(2.6,23.6059783742347,-31.0444485374626));
#47550=CARTESIAN_POINT('',(2.1,23.6059783742347,-31.0444485374626));
#47551=CARTESIAN_POINT('Ctrl Pts',(2.1,23.6059783742347,-31.0444485374626));
#47552=CARTESIAN_POINT('Ctrl Pts',(2.26666666666667,23.6059783742347,-31.0444485374626));
#47553=CARTESIAN_POINT('Ctrl Pts',(2.43346490340496,23.6059860909079,-31.0444445811933));
#47554=CARTESIAN_POINT('Ctrl Pts',(2.60035670167875,23.6059979144327,-31.0444385373999));
#47555=CARTESIAN_POINT('',(2.1,9.55344044321366,-37.8117941348724));
#47556=CARTESIAN_POINT('Origin',(2.1,0.,0.));
#47557=CARTESIAN_POINT('',(2.6,9.55344044321365,-37.8117941348724));
#47558=CARTESIAN_POINT('Ctrl Pts',(2.59961800914399,9.55341844221435,-37.8117958094788));
#47559=CARTESIAN_POINT('Ctrl Pts',(2.43319197104145,9.5534317600474,-37.8117948001723));
#47560=CARTESIAN_POINT('Ctrl Pts',(2.26666666666667,9.55344044321366,-37.8117941348724));
#47561=CARTESIAN_POINT('Ctrl Pts',(2.1,9.55344044321366,-37.8117941348724));
#47562=CARTESIAN_POINT('',(6.,9.62277221548328,-37.7942092772018));
#47563=CARTESIAN_POINT('Ctrl Pts',(2.6,9.55344044321366,-37.8117941348724));
#47564=CARTESIAN_POINT('Ctrl Pts',(3.15786519714955,9.55344044321366,-37.8117941348724));
#47565=CARTESIAN_POINT('Ctrl Pts',(3.71593098901213,9.54260105934372,-37.8145341633936));
#47566=CARTESIAN_POINT('Ctrl Pts',(4.82421019263741,9.57175670889429,-37.8071646217058));
#47567=CARTESIAN_POINT('Ctrl Pts',(5.40687161376251,9.62248834608612,-37.7942815531033));
#47568=CARTESIAN_POINT('Ctrl Pts',(6.,9.62277221548328,-37.7942092772018));
#47569=CARTESIAN_POINT('',(6.,7.86863926112478,-38.1979648172293));
#47570=CARTESIAN_POINT('Origin',(6.,0.,0.));
#47571=CARTESIAN_POINT('',(2.6,7.79857020128637,-38.2123318159938));
#47572=CARTESIAN_POINT('Ctrl Pts',(6.,7.86863926112478,-38.1979648172293));
#47573=CARTESIAN_POINT('Ctrl Pts',(5.46151291267476,7.86832344852115,-38.1980298734558));
#47574=CARTESIAN_POINT('Ctrl Pts',(4.90416494331291,7.81853615114211,-38.2082548857951));
#47575=CARTESIAN_POINT('Ctrl Pts',(3.74812575287323,7.78784373112913,-38.2145225239784));
#47576=CARTESIAN_POINT('Ctrl Pts',(3.17396064416408,7.79857020128638,-38.2123318159938));
#47577=CARTESIAN_POINT('Ctrl Pts',(2.6,7.79857020128638,-38.2123318159938));
#47578=CARTESIAN_POINT('',(2.1,7.79857020128638,-38.2123318159937));
#47579=CARTESIAN_POINT('Ctrl Pts',(2.1,7.79857020128638,-38.2123318159937));
#47580=CARTESIAN_POINT('Ctrl Pts',(2.26666666666667,7.79857020128638,-38.2123318159937));
#47581=CARTESIAN_POINT('Ctrl Pts',(2.43357876469311,7.7985739143114,-38.2123317838051));
#47582=CARTESIAN_POINT('Ctrl Pts',(2.60065399305178,7.79858017606306,-38.2123316380654));
#47583=CARTESIAN_POINT('',(2.1,-7.79857020128639,-38.2123318159937));
#47584=CARTESIAN_POINT('Origin',(2.1,0.,0.));
#47585=CARTESIAN_POINT('',(2.6,-7.79857020128639,-38.2123318159937));
#47586=CARTESIAN_POINT('Ctrl Pts',(2.59964466174317,-7.79859228682692,-38.2123216610868));
#47587=CARTESIAN_POINT('Ctrl Pts',(2.43320229863994,-7.79857892554184,-38.2123278118252));
#47588=CARTESIAN_POINT('Ctrl Pts',(2.26666666666667,-7.79857020128639,-38.2123318159937));
#47589=CARTESIAN_POINT('Ctrl Pts',(2.1,-7.79857020128639,-38.2123318159937));
#47590=CARTESIAN_POINT('',(6.,-7.72847464911698,-38.226570335278));
#47591=CARTESIAN_POINT('Ctrl Pts',(2.6,-7.79857020128639,-38.2123318159937));
#47592=CARTESIAN_POINT('Ctrl Pts',(3.15786555369928,-7.79857020128639,-38.2123318159937));
#47593=CARTESIAN_POINT('Ctrl Pts',(3.71593170347639,-7.80952503047415,-38.2100974582948));
#47594=CARTESIAN_POINT('Ctrl Pts',(4.82421093519821,-7.78005907955,-38.2161079120687));
#47595=CARTESIAN_POINT('Ctrl Pts',(5.40687201153467,-7.72876176575221,-38.2265122873386));
#47596=CARTESIAN_POINT('Ctrl Pts',(6.,-7.72847464911697,-38.226570335278));
#47597=CARTESIAN_POINT('',(6.,-9.48407679455226,-37.8292517419395));
#47598=CARTESIAN_POINT('Origin',(6.,0.,0.));
#47599=CARTESIAN_POINT('',(2.6,-9.55344044321367,-37.8117941348724));
#47600=CARTESIAN_POINT('Ctrl Pts',(6.,-9.48407679455225,-37.8292517419395));
#47601=CARTESIAN_POINT('Ctrl Pts',(5.46151292711359,-9.48438955870664,-37.8291733296231));
#47602=CARTESIAN_POINT('Ctrl Pts',(4.90416497508538,-9.53368282748551,-37.8167838493645));
#47603=CARTESIAN_POINT('Ctrl Pts',(3.7481257854858,-9.56405517251088,-37.8091138533209));
#47604=CARTESIAN_POINT('Ctrl Pts',(3.17396066044241,-9.55344044321367,-37.8117941348724));
#47605=CARTESIAN_POINT('Ctrl Pts',(2.6,-9.55344044321367,-37.8117941348724));
#47606=CARTESIAN_POINT('',(2.1,-9.55344044321367,-37.8117941348724));
#47607=CARTESIAN_POINT('Ctrl Pts',(2.1,-9.55344044321367,-37.8117941348724));
#47608=CARTESIAN_POINT('Ctrl Pts',(2.26666666666667,-9.55344044321367,-37.8117941348724));
#47609=CARTESIAN_POINT('Ctrl Pts',(2.43346068603049,-9.55343112836961,-37.8117982691431));
#47610=CARTESIAN_POINT('Ctrl Pts',(2.60034598551963,-9.55341685439516,-37.8118046211416));
#47611=CARTESIAN_POINT('',(2.1,-23.6059783742347,-31.0444485374626));
#47612=CARTESIAN_POINT('Origin',(2.1,0.,0.));
#47613=CARTESIAN_POINT('',(2.6,-23.6059783742347,-31.0444485374626));
#47614=CARTESIAN_POINT('Ctrl Pts',(2.59962088519067,-23.6059943926253,-31.0444314441149));
#47615=CARTESIAN_POINT('Ctrl Pts',(2.43319308967147,-23.6059846984282,-31.0444417950463));
#47616=CARTESIAN_POINT('Ctrl Pts',(2.26666666666667,-23.6059783742347,-31.0444485374626));
#47617=CARTESIAN_POINT('Ctrl Pts',(2.1,-23.6059783742347,-31.0444485374626));
#47618=CARTESIAN_POINT('',(6.,-23.5490023259382,-31.0876903203335));
#47619=CARTESIAN_POINT('Ctrl Pts',(2.6,-23.6059783742347,-31.0444485374626));
#47620=CARTESIAN_POINT('Ctrl Pts',(3.15786519714955,-23.6059783742347,-31.0444485374626));
#47621=CARTESIAN_POINT('Ctrl Pts',(3.71593098901213,-23.6148788600968,-31.0376823457423));
#47622=CARTESIAN_POINT('Ctrl Pts',(4.82421019263741,-23.5909388702326,-31.055882316366));
#47623=CARTESIAN_POINT('Ctrl Pts',(5.40687161376251,-23.5492358231876,-31.0875134455894));
#47624=CARTESIAN_POINT('Ctrl Pts',(6.,-23.5490023259382,-31.0876903203335));
#47625=CARTESIAN_POINT('',(6.,-24.9583551264995,-29.9679914138325));
#47626=CARTESIAN_POINT('Origin',(6.,0.,0.));
#47627=CARTESIAN_POINT('',(2.6,-25.0132750426772,-29.9221668941168));
#47628=CARTESIAN_POINT('Ctrl Pts',(6.,-24.9583551264995,-29.9679914138325));
#47629=CARTESIAN_POINT('Ctrl Pts',(5.46151291267476,-24.9586028954432,-29.9677850634902));
#47630=CARTESIAN_POINT('Ctrl Pts',(4.90416494331291,-24.9976390041765,-29.9352349778897));
#47631=CARTESIAN_POINT('Ctrl Pts',(3.74812575287323,-25.0216756519015,-29.9151464861394));
#47632=CARTESIAN_POINT('Ctrl Pts',(3.17396064416408,-25.0132750426772,-29.9221668941168));
#47633=CARTESIAN_POINT('Ctrl Pts',(2.6,-25.0132750426772,-29.9221668941168));
#47634=CARTESIAN_POINT('',(2.1,-25.0132750426772,-29.9221668941168));
#47635=CARTESIAN_POINT('Ctrl Pts',(2.1,-25.0132750426772,-29.9221668941168));
#47636=CARTESIAN_POINT('Ctrl Pts',(2.26666666666667,-25.0132750426772,-29.9221668941168));
#47637=CARTESIAN_POINT('Ctrl Pts',(2.43357825612586,-25.0132726154855,-29.9221698582808));
#47638=CARTESIAN_POINT('Ctrl Pts',(2.60065266451408,-25.0132684616017,-29.9221747898881));
#47639=CARTESIAN_POINT('',(2.1,-34.7379330218401,-17.7278314909114));
#47640=CARTESIAN_POINT('Origin',(2.1,0.,0.));
#47641=CARTESIAN_POINT('',(2.6,-34.7379330218401,-17.7278314909114));
#47642=CARTESIAN_POINT('Ctrl Pts',(2.59964387481778,-34.7379384978419,-17.727810026438));
#47643=CARTESIAN_POINT('Ctrl Pts',(2.43320198848801,-34.7379351912261,-17.7278230129461));
#47644=CARTESIAN_POINT('Ctrl Pts',(2.26666666666667,-34.7379330218401,-17.7278314909114));
#47645=CARTESIAN_POINT('Ctrl Pts',(2.1,-34.7379330218401,-17.7278314909114));
#47646=CARTESIAN_POINT('',(6.,-34.705361282547,-17.7915119719457));
#47647=CARTESIAN_POINT('Ctrl Pts',(2.6,-34.7379330218401,-17.7278314909114));
#47648=CARTESIAN_POINT('Ctrl Pts',(3.15786555369928,-34.7379330218401,-17.7278314909114));
#47649=CARTESIAN_POINT('Ctrl Pts',(3.71593170347639,-34.7430163549277,-17.7178735613284));
#47650=CARTESIAN_POINT('Ctrl Pts',(4.82421093519821,-34.7293437970088,-17.7446584260543));
#47651=CARTESIAN_POINT('Ctrl Pts',(5.40687201153467,-34.7054949131345,-17.7912513028229));
#47652=CARTESIAN_POINT('Ctrl Pts',(6.,-34.705361282547,-17.7915119719457));
#47653=CARTESIAN_POINT('',(6.,-35.4893251315053,-16.1712028529206));
#47654=CARTESIAN_POINT('Origin',(6.,0.,0.));
#47655=CARTESIAN_POINT('',(2.6,-35.5189237522517,-16.106087528687));
#47656=CARTESIAN_POINT('Ctrl Pts',(6.,-35.4893251315053,-16.1712028529206));
#47657=CARTESIAN_POINT('Ctrl Pts',(5.46151292711359,-35.4894588315483,-16.1709094347785));
#47658=CARTESIAN_POINT('Ctrl Pts',(4.90416497508538,-35.5105061962146,-16.1246456907818));
#47659=CARTESIAN_POINT('Ctrl Pts',(3.7481257854858,-35.5234463992192,-16.0961174709311));
#47660=CARTESIAN_POINT('Ctrl Pts',(3.17396066044241,-35.5189237522517,-16.106087528687));
#47661=CARTESIAN_POINT('Ctrl Pts',(2.6,-35.5189237522517,-16.106087528687));
#47662=CARTESIAN_POINT('',(2.1,-35.5189237522517,-16.106087528687));
#47663=CARTESIAN_POINT('Ctrl Pts',(2.1,-35.5189237522517,-16.106087528687));
#47664=CARTESIAN_POINT('Ctrl Pts',(2.26666666666667,-35.5189237522517,-16.106087528687));
#47665=CARTESIAN_POINT('Ctrl Pts',(2.43346396189077,-35.5189213983861,-16.1060969924349));
#47666=CARTESIAN_POINT('Ctrl Pts',(2.60035429878701,-35.5189178073564,-16.1061114988275));
#47667=CARTESIAN_POINT('',(2.1,-38.98961400168,-0.899999999999995));
#47668=CARTESIAN_POINT('Origin',(2.1,0.,0.));
#47669=CARTESIAN_POINT('',(2.6,-38.98961400168,-0.89999999999999));
#47670=CARTESIAN_POINT('Ctrl Pts',(2.59961881382767,-38.9896107068492,-0.899977798557519));
#47671=CARTESIAN_POINT('Ctrl Pts',(2.43319228396236,-38.9896127056027,-0.899991237216741));
#47672=CARTESIAN_POINT('Ctrl Pts',(2.26666666666667,-38.98961400168,-0.899999999999995));
#47673=CARTESIAN_POINT('Ctrl Pts',(2.1,-38.98961400168,-0.899999999999995));
#47674=CARTESIAN_POINT('',(6.,-38.9878978038234,-0.971506478939042));
#47675=CARTESIAN_POINT('Ctrl Pts',(2.6,-38.98961400168,-0.899999999999995));
#47676=CARTESIAN_POINT('Ctrl Pts',(3.15786519714955,-38.98961400168,-0.899999999999995));
#47677=CARTESIAN_POINT('Ctrl Pts',(3.71593098901213,-38.9898733421432,-0.888822668408729));
#47678=CARTESIAN_POINT('Ctrl Pts',(4.82421019263741,-38.9891763126199,-0.918887202252576));
#47679=CARTESIAN_POINT('Ctrl Pts',(5.40687161376251,-38.9879051007338,-0.971213643839228));
#47680=CARTESIAN_POINT('Ctrl Pts',(6.,-38.9878978038234,-0.971506478939041));
#47681=CARTESIAN_POINT('',(6.,-39.,-4.77612251667468E-15));
#47682=CARTESIAN_POINT('Origin',(6.,0.,0.));
#47683=CARTESIAN_POINT('',(0.499999999999998,-39.,-4.77612251667468E-15));
#47684=CARTESIAN_POINT('',(1.55,-39.,-4.77612251667468E-15));
#47685=CARTESIAN_POINT('Origin',(0.499999999999998,0.,0.));
#47686=CARTESIAN_POINT('',(6.,-38.9911990462069,0.828490759799985));
#47687=CARTESIAN_POINT('Origin',(6.,0.,0.));
#47688=CARTESIAN_POINT('',(2.6,-38.98961400168,0.90000000000001));
#47689=CARTESIAN_POINT('Ctrl Pts',(6.,-38.9911990462069,0.828490759799983));
#47690=CARTESIAN_POINT('Ctrl Pts',(5.46151291267476,-38.9911921964225,0.82881313069457));
#47691=CARTESIAN_POINT('Ctrl Pts',(4.90416494331291,-38.9900821304425,0.879627435876937));
#47692=CARTESIAN_POINT('Ctrl Pts',(3.74812575287323,-38.9893629198842,0.910945013542259));
#47693=CARTESIAN_POINT('Ctrl Pts',(3.17396064416408,-38.98961400168,0.900000000000005));
#47694=CARTESIAN_POINT('Ctrl Pts',(2.6,-38.98961400168,0.900000000000005));
#47695=CARTESIAN_POINT('',(2.1,-38.98961400168,0.900000000000005));
#47696=CARTESIAN_POINT('Ctrl Pts',(2.1,-38.98961400168,0.900000000000005));
#47697=CARTESIAN_POINT('Ctrl Pts',(2.26666666666667,-38.98961400168,0.900000000000005));
#47698=CARTESIAN_POINT('Ctrl Pts',(2.43357901978584,-38.9896147918638,0.899996432344951));
#47699=CARTESIAN_POINT('Ctrl Pts',(2.60065465957353,-38.9896160358867,0.899990387940704));
#47700=CARTESIAN_POINT('',(2.1,-35.5189237522517,16.106087528687));
#47701=CARTESIAN_POINT('Origin',(2.1,0.,0.));
#47702=CARTESIAN_POINT('',(2.6,-35.5189237522517,16.106087528687));
#47703=CARTESIAN_POINT('Ctrl Pts',(2.59964104784901,-35.5189096730421,16.1061056668086));
#47704=CARTESIAN_POINT('Ctrl Pts',(2.43320088693784,-35.5189181968381,16.1060946966857));
#47705=CARTESIAN_POINT('Ctrl Pts',(2.26666666666667,-35.5189237522517,16.106087528687));
#47706=CARTESIAN_POINT('Ctrl Pts',(2.1,-35.5189237522517,16.106087528687));
#47707=CARTESIAN_POINT('',(6.,-35.548403009865,16.0409177869666));
#47708=CARTESIAN_POINT('Ctrl Pts',(2.6,-35.5189237522517,16.106087528687));
#47709=CARTESIAN_POINT('Ctrl Pts',(3.15786555369928,-35.5189237522517,16.106087528687));
#47710=CARTESIAN_POINT('Ctrl Pts',(3.71593170347639,-35.5143077357431,16.1162705060734));
#47711=CARTESIAN_POINT('Ctrl Pts',(4.82421093519821,-35.5267242858117,16.0888807798457));
#47712=CARTESIAN_POINT('Ctrl Pts',(5.40687201153467,-35.5482825278469,16.0411847881066));
#47713=CARTESIAN_POINT('Ctrl Pts',(6.,-35.548403009865,16.0409177869666));
#47714=CARTESIAN_POINT('',(6.,-34.7703877941326,17.6640916167698));
#47715=CARTESIAN_POINT('Origin',(6.,0.,0.));
#47716=CARTESIAN_POINT('',(2.6,-34.7379330218401,17.7278314909114));
#47717=CARTESIAN_POINT('Ctrl Pts',(6.,-34.7703877941326,17.6640916167698));
#47718=CARTESIAN_POINT('Ctrl Pts',(5.46151292711359,-34.7702417512048,17.664379090892));
#47719=CARTESIAN_POINT('Ctrl Pts',(4.90416497508538,-34.7471941168769,17.7096795557888));
#47720=CARTESIAN_POINT('Ctrl Pts',(3.7481257854858,-34.7329579410662,17.7375836680294));
#47721=CARTESIAN_POINT('Ctrl Pts',(3.17396066044241,-34.7379330218401,17.7278314909114));
#47722=CARTESIAN_POINT('Ctrl Pts',(2.6,-34.7379330218401,17.7278314909114));
#47723=CARTESIAN_POINT('',(2.10000000000001,-34.7379330218401,17.7278314909114));
#47724=CARTESIAN_POINT('Ctrl Pts',(2.10000000000001,-34.7379330218401,17.7278314909114));
#47725=CARTESIAN_POINT('Ctrl Pts',(2.26666666666667,-34.7379330218401,17.7278314909114));
#47726=CARTESIAN_POINT('Ctrl Pts',(2.4334616795417,-34.7379389230122,17.7278236408502));
#47727=CARTESIAN_POINT('Ctrl Pts',(2.6003485284748,-34.7379479808194,17.7278116174341));
#47728=CARTESIAN_POINT('',(2.10000000000001,-25.0132750426772,29.9221668941169));
#47729=CARTESIAN_POINT('Origin',(2.10000000000001,0.,0.));
#47730=CARTESIAN_POINT('',(2.6,-25.0132750426772,29.9221668941169));
#47731=CARTESIAN_POINT('Ctrl Pts',(2.59962040969903,-25.0132550013658,29.9221785815268));
#47732=CARTESIAN_POINT('Ctrl Pts',(2.43319290469077,-25.0132671359778,29.9221715099518));
#47733=CARTESIAN_POINT('Ctrl Pts',(2.26666666666667,-25.0132750426772,29.9221668941169));
#47734=CARTESIAN_POINT('Ctrl Pts',(2.10000000000001,-25.0132750426772,29.9221668941169));
#47735=CARTESIAN_POINT('',(6.,-25.0681110272506,29.8762415562171));
#47736=CARTESIAN_POINT('Ctrl Pts',(2.6,-25.0132750426772,29.9221668941169));
#47737=CARTESIAN_POINT('Ctrl Pts',(3.15786519714955,-25.0132750426772,29.9221668941169));
#47738=CARTESIAN_POINT('Ctrl Pts',(3.71593098901213,-25.0046979490832,29.9293386069149));
#47739=CARTESIAN_POINT('Ctrl Pts',(4.82421019263741,-25.0277687573486,29.91004871704));
#47740=CARTESIAN_POINT('Ctrl Pts',(5.40687161376251,-25.0678866290996,29.8764298408698));
#47741=CARTESIAN_POINT('Ctrl Pts',(6.,-25.0681110272506,29.8762415562171));
#47742=CARTESIAN_POINT('',(6.,-23.6628748086085,31.0011024931715));
#47743=CARTESIAN_POINT('Origin',(6.,0.,0.));
#47744=CARTESIAN_POINT('',(2.6,-23.6059783742347,31.0444485374626));
#47745=CARTESIAN_POINT('Ctrl Pts',(6.,-23.6628748086085,31.0011024931715));
#47746=CARTESIAN_POINT('Ctrl Pts',(5.46151291267476,-23.6626184981234,31.0012981327595));
#47747=CARTESIAN_POINT('Ctrl Pts',(4.90416494331291,-23.6221981597541,31.0321124492985));
#47748=CARTESIAN_POINT('Ctrl Pts',(3.74812575287323,-23.5972646711323,31.0510763381348));
#47749=CARTESIAN_POINT('Ctrl Pts',(3.17396064416408,-23.6059783742347,31.0444485374626));
#47750=CARTESIAN_POINT('Ctrl Pts',(2.6,-23.6059783742347,31.0444485374626));
#47751=CARTESIAN_POINT('',(2.1,-23.6059783742347,31.0444485374626));
#47752=CARTESIAN_POINT('Ctrl Pts',(2.1,-23.6059783742347,31.0444485374626));
#47753=CARTESIAN_POINT('Ctrl Pts',(2.26666666666667,-23.6059783742347,31.0444485374626));
#47754=CARTESIAN_POINT('Ctrl Pts',(2.43357841627175,-23.6059817731134,31.0444468517412));
#47755=CARTESIAN_POINT('Ctrl Pts',(2.60065308282599,-23.6059874569122,31.0444439322163));
#47756=CARTESIAN_POINT('',(2.1,-9.55344044321367,37.8117941348724));
#47757=CARTESIAN_POINT('Origin',(2.1,0.,0.));
#47758=CARTESIAN_POINT('',(2.6,-9.55344044321366,37.8117941348724));
#47759=CARTESIAN_POINT('Ctrl Pts',(2.59964755923549,-9.55341505766335,37.8117946735604));
#47760=CARTESIAN_POINT('Ctrl Pts',(2.43320343087526,-9.5534304198444,37.8117943540172));
#47761=CARTESIAN_POINT('Ctrl Pts',(2.26666666666667,-9.55344044321366,37.8117941348724));
#47762=CARTESIAN_POINT('Ctrl Pts',(2.1,-9.55344044321366,37.8117941348724));
#47763=CARTESIAN_POINT('',(6.,-9.62277221548329,37.7942092772018));
#47764=CARTESIAN_POINT('Ctrl Pts',(2.6,-9.55344044321366,37.8117941348724));
#47765=CARTESIAN_POINT('Ctrl Pts',(3.15786555369928,-9.55344044321366,37.8117941348724));
#47766=CARTESIAN_POINT('Ctrl Pts',(3.71593170347639,-9.54260103168937,37.8145341703953));
#47767=CARTESIAN_POINT('Ctrl Pts',(4.82421093519821,-9.57175677429238,37.8071646051639));
#47768=CARTESIAN_POINT('Ctrl Pts',(5.40687201153467,-9.6224883462765,37.7942815530548));
#47769=CARTESIAN_POINT('Ctrl Pts',(6.,-9.62277221548328,37.7942092772018));
#47770=CARTESIAN_POINT('',(6.,-7.86863926112478,38.1979648172293));
#47771=CARTESIAN_POINT('Origin',(6.,0.,0.));
#47772=CARTESIAN_POINT('',(2.6,-7.79857020128639,38.2123318159937));
#47773=CARTESIAN_POINT('Ctrl Pts',(6.,-7.86863926112479,38.1979648172293));
#47774=CARTESIAN_POINT('Ctrl Pts',(5.46151292711359,-7.86832344852962,38.1980298734541));
#47775=CARTESIAN_POINT('Ctrl Pts',(4.90416497508538,-7.81853615394239,38.2082548852227));
#47776=CARTESIAN_POINT('Ctrl Pts',(3.7481257854858,-7.78784373006694,38.2145225241958));
#47777=CARTESIAN_POINT('Ctrl Pts',(3.17396066044241,-7.79857020128638,38.2123318159937));
#47778=CARTESIAN_POINT('Ctrl Pts',(2.6,-7.79857020128638,38.2123318159937));
#47779=CARTESIAN_POINT('',(2.1,-7.79857020128638,38.2123318159937));
#47780=CARTESIAN_POINT('Ctrl Pts',(2.1,-7.79857020128638,38.2123318159937));
#47781=CARTESIAN_POINT('Ctrl Pts',(2.26666666666667,-7.79857020128638,38.2123318159937));
#47782=CARTESIAN_POINT('Ctrl Pts',(2.43346449336972,-7.79857975198003,38.2123316464336));
#47783=CARTESIAN_POINT('Ctrl Pts',(2.60035565904183,-7.79859438653547,38.2123314033356));
#47784=CARTESIAN_POINT('',(2.1,7.79857020128639,38.2123318159937));
#47785=CARTESIAN_POINT('Origin',(2.1,0.,0.));
#47786=CARTESIAN_POINT('',(2.6,7.79857020128639,38.2123318159937));
#47787=CARTESIAN_POINT('Ctrl Pts',(2.59962016861433,7.79859172526737,38.2123234687558));
#47788=CARTESIAN_POINT('Ctrl Pts',(2.4331928109074,7.79857869688915,38.2123285258734));
#47789=CARTESIAN_POINT('Ctrl Pts',(2.26666666666667,7.79857020128638,38.2123318159937));
#47790=CARTESIAN_POINT('Ctrl Pts',(2.1,7.79857020128638,38.2123318159937));
#47791=CARTESIAN_POINT('',(6.,7.72847464911697,38.226570335278));
#47792=CARTESIAN_POINT('Ctrl Pts',(2.6,7.79857020128639,38.2123318159937));
#47793=CARTESIAN_POINT('Ctrl Pts',(3.15786519714955,7.79857020128639,38.2123318159937));
#47794=CARTESIAN_POINT('Ctrl Pts',(3.71593098901213,7.80952500252052,38.2100974639853));
#47795=CARTESIAN_POINT('Ctrl Pts',(4.82421019263741,7.78005914564888,38.2161078985973));
#47796=CARTESIAN_POINT('Ctrl Pts',(5.4068716137625,7.72876176594476,38.2265122872997));
#47797=CARTESIAN_POINT('Ctrl Pts',(6.,7.72847464911697,38.226570335278));
#47798=CARTESIAN_POINT('',(6.,9.48407679455224,37.8292517419395));
#47799=CARTESIAN_POINT('Origin',(6.,0.,0.));
#47800=CARTESIAN_POINT('',(2.6,9.55344044321367,37.8117941348724));
#47801=CARTESIAN_POINT('Ctrl Pts',(6.,9.48407679455224,37.8292517419395));
#47802=CARTESIAN_POINT('Ctrl Pts',(5.46151291267476,9.48438955871503,37.829173329621));
#47803=CARTESIAN_POINT('Ctrl Pts',(4.90416494331291,9.53368283025682,37.8167838486652));
#47804=CARTESIAN_POINT('Ctrl Pts',(3.74812575287323,9.56405517145952,37.8091138535859));
#47805=CARTESIAN_POINT('Ctrl Pts',(3.17396064416408,9.55344044321367,37.8117941348724));
#47806=CARTESIAN_POINT('Ctrl Pts',(2.6,9.55344044321367,37.8117941348724));
#47807=CARTESIAN_POINT('',(2.1,9.55344044321367,37.8117941348724));
#47808=CARTESIAN_POINT('Ctrl Pts',(2.1,9.55344044321367,37.8117941348724));
#47809=CARTESIAN_POINT('Ctrl Pts',(2.26666666666667,9.55344044321367,37.8117941348724));
#47810=CARTESIAN_POINT('Ctrl Pts',(2.43357853708729,9.55343703309769,37.8117957327629));
#47811=CARTESIAN_POINT('Ctrl Pts',(2.60065339842836,9.55343124887636,37.8117983430894));
#47812=CARTESIAN_POINT('',(2.1,23.6059783742347,31.0444485374626));
#47813=CARTESIAN_POINT('Origin',(2.1,0.,0.));
#47814=CARTESIAN_POINT('',(2.6,23.6059783742347,31.0444485374626));
#47815=CARTESIAN_POINT('Ctrl Pts',(2.59963809215921,23.6059921558338,31.0444315655759));
#47816=CARTESIAN_POINT('Ctrl Pts',(2.43319973276619,23.6059838236274,31.0444418375603));
#47817=CARTESIAN_POINT('Ctrl Pts',(2.26666666666667,23.6059783742347,31.0444485374626));
#47818=CARTESIAN_POINT('Ctrl Pts',(2.1,23.6059783742347,31.0444485374626));
#47819=CARTESIAN_POINT('',(6.,23.5490023259382,31.0876903203335));
#47820=CARTESIAN_POINT('Ctrl Pts',(2.6,23.6059783742347,31.0444485374626));
#47821=CARTESIAN_POINT('Ctrl Pts',(3.15786555369928,23.6059783742347,31.0444485374626));
#47822=CARTESIAN_POINT('Ctrl Pts',(3.71593170347639,23.6148788828132,31.0376823284867));
#47823=CARTESIAN_POINT('Ctrl Pts',(4.82421093519821,23.5909388165246,31.0558823571826));
#47824=CARTESIAN_POINT('Ctrl Pts',(5.40687201153467,23.549235823031,31.087513445708));
#47825=CARTESIAN_POINT('Ctrl Pts',(6.,23.5490023259382,31.0876903203335));
#47826=CARTESIAN_POINT('',(6.,24.9583551264995,29.9679914138325));
#47827=CARTESIAN_POINT('Origin',(6.,0.,0.));
#47828=CARTESIAN_POINT('',(2.6,25.0132750426772,29.9221668941169));
#47829=CARTESIAN_POINT('Ctrl Pts',(6.,24.9583551264995,29.9679914138325));
#47830=CARTESIAN_POINT('Ctrl Pts',(5.46151292711359,24.9586028954365,29.9677850634957));
#47831=CARTESIAN_POINT('Ctrl Pts',(4.90416497508538,24.9976390019831,29.9352349797221));
#47832=CARTESIAN_POINT('Ctrl Pts',(3.7481257854858,25.0216756527337,29.9151464854446));
#47833=CARTESIAN_POINT('Ctrl Pts',(3.17396066044241,25.0132750426772,29.9221668941169));
#47834=CARTESIAN_POINT('Ctrl Pts',(2.6,25.0132750426772,29.9221668941169));
#47835=CARTESIAN_POINT('',(2.1,25.0132750426772,29.9221668941169));
#47836=CARTESIAN_POINT('Ctrl Pts',(2.1,25.0132750426772,29.9221668941169));
#47837=CARTESIAN_POINT('Ctrl Pts',(2.26666666666667,25.0132750426772,29.9221668941169));
#47838=CARTESIAN_POINT('Ctrl Pts',(2.43357395784791,25.0132711380509,29.9221719829006));
#47839=CARTESIAN_POINT('Ctrl Pts',(2.60064121585505,25.0132646768699,29.9221802322046));
#47840=CARTESIAN_POINT('',(2.1,34.7379330218401,17.7278314909114));
#47841=CARTESIAN_POINT('Origin',(2.1,0.,0.));
#47842=CARTESIAN_POINT('',(2.6,34.7379330218401,17.7278314909114));
#47843=CARTESIAN_POINT('Ctrl Pts',(2.59961936767386,34.7379397798986,17.7278098133928));
#47844=CARTESIAN_POINT('Ctrl Pts',(2.43319249936566,34.7379356930243,17.7278229371174));
#47845=CARTESIAN_POINT('Ctrl Pts',(2.26666666666667,34.7379330218401,17.7278314909114));
#47846=CARTESIAN_POINT('Ctrl Pts',(2.1,34.7379330218401,17.7278314909114));
#47847=CARTESIAN_POINT('',(6.,34.705361282547,17.7915119719457));
#47848=CARTESIAN_POINT('Ctrl Pts',(2.6,34.7379330218401,17.7278314909114));
#47849=CARTESIAN_POINT('Ctrl Pts',(3.15786519714955,34.7379330218401,17.7278314909114));
#47850=CARTESIAN_POINT('Ctrl Pts',(3.71593098901213,34.7430163419479,17.7178735867313));
#47851=CARTESIAN_POINT('Ctrl Pts',(4.82421019263741,34.7293438276883,17.7446583659768));
#47852=CARTESIAN_POINT('Ctrl Pts',(5.40687161376251,34.7054949132241,17.7912513026481));
#47853=CARTESIAN_POINT('Ctrl Pts',(6.,34.705361282547,17.7915119719457));
#47854=CARTESIAN_POINT('',(6.,35.4893251315053,16.1712028529206));
#47855=CARTESIAN_POINT('Origin',(6.,0.,0.));
#47856=CARTESIAN_POINT('',(2.6,35.5189237522517,16.106087528687));
#47857=CARTESIAN_POINT('Ctrl Pts',(6.,35.4893251315053,16.1712028529206));
#47858=CARTESIAN_POINT('Ctrl Pts',(5.46151291267476,35.4894588315519,16.1709094347706));
#47859=CARTESIAN_POINT('Ctrl Pts',(4.90416494331291,35.5105061973958,16.1246456881791));
#47860=CARTESIAN_POINT('Ctrl Pts',(3.74812575287323,35.5234463987708,16.0961174719183));
#47861=CARTESIAN_POINT('Ctrl Pts',(3.17396064416408,35.5189237522517,16.106087528687));
#47862=CARTESIAN_POINT('Ctrl Pts',(2.6,35.5189237522517,16.106087528687));
#47863=CARTESIAN_POINT('',(2.1,35.5189237522517,16.106087528687));
#47864=CARTESIAN_POINT('Ctrl Pts',(2.1,35.5189237522517,16.106087528687));
#47865=CARTESIAN_POINT('Ctrl Pts',(2.26666666666667,35.5189237522517,16.106087528687));
#47866=CARTESIAN_POINT('Ctrl Pts',(2.43357876746602,35.5189228948792,16.1060911408517));
#47867=CARTESIAN_POINT('Ctrl Pts',(2.60065400029651,35.5189213597892,16.1060972122346));
#47868=CARTESIAN_POINT('',(2.1,38.98961400168,0.9));
#47869=CARTESIAN_POINT('Origin',(2.1,0.,0.));
#47870=CARTESIAN_POINT('',(2.6,38.98961400168,0.899999999999996));
#47871=CARTESIAN_POINT('Ctrl Pts',(2.59964719237566,38.9896088955429,0.899975267580465));
#47872=CARTESIAN_POINT('Ctrl Pts',(2.43320328750148,38.9896119918161,0.899990232939572));
#47873=CARTESIAN_POINT('Ctrl Pts',(2.26666666666667,38.98961400168,0.9));
#47874=CARTESIAN_POINT('Ctrl Pts',(2.1,38.98961400168,0.9));
#47875=CARTESIAN_POINT('',(6.,38.9878978038234,0.971506478939047));
#47876=CARTESIAN_POINT('Ctrl Pts',(2.6,38.98961400168,0.9));
#47877=CARTESIAN_POINT('Ctrl Pts',(3.15786555369928,38.98961400168,0.9));
#47878=CARTESIAN_POINT('Ctrl Pts',(3.71593170347639,38.9898733428157,0.888822639889713));
#47879=CARTESIAN_POINT('Ctrl Pts',(4.82421093519821,38.9891763110452,0.918887269691915));
#47880=CARTESIAN_POINT('Ctrl Pts',(5.40687201153467,38.9879051007289,0.971213644035619));
#47881=CARTESIAN_POINT('Ctrl Pts',(6.,38.9878978038234,0.971506478939046));
#47882=CARTESIAN_POINT('',(6.,38.9911990462069,-0.82849075979999));
#47883=CARTESIAN_POINT('Origin',(6.,0.,0.));
#47884=CARTESIAN_POINT('Ctrl Pts',(6.,38.9911990462069,-0.828490759799977));
#47885=CARTESIAN_POINT('Ctrl Pts',(5.46151292711359,38.9911921964227,-0.828813130685921));
#47886=CARTESIAN_POINT('Ctrl Pts',(4.90416497508538,38.9900821305076,-0.879627433019496));
#47887=CARTESIAN_POINT('Ctrl Pts',(3.7481257854858,38.9893629198599,-0.910945014626199));
#47888=CARTESIAN_POINT('Ctrl Pts',(3.17396066044241,38.98961400168,-0.9));
#47889=CARTESIAN_POINT('Ctrl Pts',(2.6,38.98961400168,-0.9));
#47890=CARTESIAN_POINT('Origin',(2.44847982464479,0.,-1.17996027893162E-15));
#47891=CARTESIAN_POINT('',(2.79695964929223,34.3237608806509,17.5283766998975));
#47892=CARTESIAN_POINT('Ctrl Pts',(2.09999999999999,34.7379330218402,17.7278314909114));
#47893=CARTESIAN_POINT('Ctrl Pts',(2.33231184706804,34.599880855471,17.6613490715166));
#47894=CARTESIAN_POINT('Ctrl Pts',(2.56464811501599,34.4618137435185,17.5948594547083));
#47895=CARTESIAN_POINT('Ctrl Pts',(2.79695964929243,34.323760880652,17.528376699898));
#47896=CARTESIAN_POINT('',(2.79695964929243,24.7266590280231,29.5627617796016));
#47897=CARTESIAN_POINT('Ctrl Pts',(2.79695964929244,24.726659028024,29.5627617796028));
#47898=CARTESIAN_POINT('Ctrl Pts',(2.56464811249614,24.8221945743839,29.6825595655751));
#47899=CARTESIAN_POINT('Ctrl Pts',(2.3323118418722,24.9177399814814,29.8023697165212));
#47900=CARTESIAN_POINT('Ctrl Pts',(2.09999999999999,25.0132750426772,29.9221668941169));
#47901=CARTESIAN_POINT('Origin',(2.79695964928958,0.,-2.35992055786324E-15));
#47902=CARTESIAN_POINT('Origin',(2.44847982464479,0.,-1.17996027893162E-15));
#47903=CARTESIAN_POINT('',(2.79695964929224,7.69627812998458,37.7641609687218));
#47904=CARTESIAN_POINT('Ctrl Pts',(2.1,7.7985702012864,38.2123318159938));
#47905=CARTESIAN_POINT('Ctrl Pts',(2.3323118422578,7.7644741326502,38.0629471787011));
#47906=CARTESIAN_POINT('Ctrl Pts',(2.56464811269316,7.73037437168869,37.9135463642742));
#47907=CARTESIAN_POINT('Ctrl Pts',(2.79695964929243,7.69627812998494,37.764160968723));
#47908=CARTESIAN_POINT('',(2.79695964929243,-7.69627812998452,37.7641609687216));
#47909=CARTESIAN_POINT('Ctrl Pts',(2.79695964929243,-7.69627812998494,37.764160968723));
#47910=CARTESIAN_POINT('Ctrl Pts',(2.56464811432525,-7.73037437144915,37.9135463632247));
#47911=CARTESIAN_POINT('Ctrl Pts',(2.33231184565996,-7.76447413215086,38.0629471765134));
#47912=CARTESIAN_POINT('Ctrl Pts',(2.1,-7.7985702012864,38.2123318159938));
#47913=CARTESIAN_POINT('Origin',(2.79695964928958,0.,-2.35992055786324E-15));
#47914=CARTESIAN_POINT('Origin',(2.4484798246448,0.,-1.17996027893162E-15));
#47915=CARTESIAN_POINT('',(2.79695964929224,-24.7266590280233,29.5627617796018));
#47916=CARTESIAN_POINT('Ctrl Pts',(2.10000000000001,-25.0132750426772,29.9221668941169));
#47917=CARTESIAN_POINT('Ctrl Pts',(2.33231184323714,-24.9177399809201,29.8023697158173));
#47918=CARTESIAN_POINT('Ctrl Pts',(2.5646481131599,-24.8221945741109,29.6825595652328));
#47919=CARTESIAN_POINT('Ctrl Pts',(2.79695964929245,-24.726659028024,29.5627617796028));
#47920=CARTESIAN_POINT('',(2.79695964929243,-34.3237608806506,17.5283766998975));
#47921=CARTESIAN_POINT('Ctrl Pts',(2.79695964929245,-34.323760880652,17.528376699898));
#47922=CARTESIAN_POINT('Ctrl Pts',(2.56464811314235,-34.4618137446319,17.5948594552445));
#47923=CARTESIAN_POINT('Ctrl Pts',(2.33231184320826,-34.5998808577647,17.6613490726212));
#47924=CARTESIAN_POINT('Ctrl Pts',(2.09999999999999,-34.7379330218402,17.7278314909114));
#47925=CARTESIAN_POINT('Origin',(2.79695964928959,0.,-2.35992055786324E-15));
#47926=CARTESIAN_POINT('Origin',(2.44847982464479,0.,-1.17996027893162E-15));
#47927=CARTESIAN_POINT('',(2.79695964929223,-38.529917606006,-0.900000000000067));
#47928=CARTESIAN_POINT('Ctrl Pts',(2.1,-38.98961400168,-0.899999999999995));
#47929=CARTESIAN_POINT('Ctrl Pts',(2.33231184677866,-38.8363876571131,-0.899999999999995));
#47930=CARTESIAN_POINT('Ctrl Pts',(2.56464811488244,-38.6831447239067,-0.899999999999995));
#47931=CARTESIAN_POINT('Ctrl Pts',(2.79695964929244,-38.5299176060072,-0.899999999999995));
#47932=CARTESIAN_POINT('',(2.79695964929243,-35.1047516110623,-15.906632737673));
#47933=CARTESIAN_POINT('Ctrl Pts',(2.79695964929244,-35.1047516110636,-15.9066327376736));
#47934=CARTESIAN_POINT('Ctrl Pts',(2.56464811161146,-35.2428044759532,-15.9731154934582));
#47935=CARTESIAN_POINT('Ctrl Pts',(2.33231184003613,-35.3808715900613,-16.0396051113046));
#47936=CARTESIAN_POINT('Ctrl Pts',(2.09999999999999,-35.5189237522517,-16.106087528687));
#47937=CARTESIAN_POINT('Origin',(2.79695964928958,0.,-2.35992055786324E-15));
#47938=CARTESIAN_POINT('Origin',(2.44847982464479,0.,-1.17996027893162E-15));
#47939=CARTESIAN_POINT('',(2.79695964929223,-23.3193623595807,-30.6850434229476));
#47940=CARTESIAN_POINT('Ctrl Pts',(2.1,-23.6059783742347,-31.0444485374625));
#47941=CARTESIAN_POINT('Ctrl Pts',(2.3323118390093,-23.5104433142162,-30.9246513613431));
#47942=CARTESIAN_POINT('Ctrl Pts',(2.56464811110358,-23.4148979065141,-30.8048412096388));
#47943=CARTESIAN_POINT('Ctrl Pts',(2.79695964929244,-23.3193623595815,-30.6850434229485));
#47944=CARTESIAN_POINT('',(2.79695964929243,-9.45114837191197,-37.3636232876002));
#47945=CARTESIAN_POINT('Ctrl Pts',(2.79695964929244,-9.45114837191219,-37.3636232876015));
#47946=CARTESIAN_POINT('Ctrl Pts',(2.56464811107789,-9.48524461385302,-37.5130086841914));
#47947=CARTESIAN_POINT('Ctrl Pts',(2.33231183894366,-9.51934437506386,-37.6624094997107));
#47948=CARTESIAN_POINT('Ctrl Pts',(2.09999999999998,-9.55344044321365,-37.8117941348723));
#47949=CARTESIAN_POINT('Origin',(2.79695964928958,0.,-2.35992055786324E-15));
#47950=CARTESIAN_POINT('Origin',(2.44847982464479,0.,-1.17996027893162E-15));
#47951=CARTESIAN_POINT('',(2.79695964929223,9.451148371912,-37.3636232876004));
#47952=CARTESIAN_POINT('Ctrl Pts',(2.09999999999999,9.55344044321364,-37.8117941348723));
#47953=CARTESIAN_POINT('Ctrl Pts',(2.33231183759833,9.5193443752613,-37.6624095005758));
#47954=CARTESIAN_POINT('Ctrl Pts',(2.56464811043332,9.48524461394761,-37.5130086846059));
#47955=CARTESIAN_POINT('Ctrl Pts',(2.79695964929243,9.45114837191218,-37.3636232876015));
#47956=CARTESIAN_POINT('',(2.79695964929243,23.3193623595806,-30.6850434229474));
#47957=CARTESIAN_POINT('Ctrl Pts',(2.79695964929244,23.3193623595815,-30.6850434229485));
#47958=CARTESIAN_POINT('Ctrl Pts',(2.56464811252804,23.4148979059282,-30.8048412089043));
#47959=CARTESIAN_POINT('Ctrl Pts',(2.33231184190073,23.5104433130272,-30.9246513598521));
#47960=CARTESIAN_POINT('Ctrl Pts',(2.09999999999999,23.6059783742347,-31.0444485374625));
#47961=CARTESIAN_POINT('Origin',(2.79695964928958,0.,-2.35992055786324E-15));
#47962=CARTESIAN_POINT('Origin',(2.44847982464479,0.,-1.17996027893162E-15));
#47963=CARTESIAN_POINT('',(2.79695964929222,38.529917606006,0.900000000000072));
#47964=CARTESIAN_POINT('Ctrl Pts',(2.09999999999999,38.98961400168,0.9));
#47965=CARTESIAN_POINT('Ctrl Pts',(2.33231184201649,38.8363876602541,0.9));
#47966=CARTESIAN_POINT('Ctrl Pts',(2.56464811257203,38.6831447254306,0.9));
#47967=CARTESIAN_POINT('Ctrl Pts',(2.79695964929222,38.5299176060073,0.9));
#47968=CARTESIAN_POINT('',(2.79695964929053,35.1047516110643,15.906632737674));
#47969=CARTESIAN_POINT('Ctrl Pts',(2.79695964929223,35.1047516110637,15.9066327376737));
#47970=CARTESIAN_POINT('Ctrl Pts',(2.56464811186606,35.242804475802,15.9731154933853));
#47971=CARTESIAN_POINT('Ctrl Pts',(2.33231184056647,35.3808715897462,16.0396051111529));
#47972=CARTESIAN_POINT('Ctrl Pts',(2.09999999999999,35.5189237522518,16.1060875286871));
#47973=CARTESIAN_POINT('Origin',(2.79695964928958,0.,-2.35992055786324E-15));
#47974=CARTESIAN_POINT('Origin',(2.44847982464479,0.,-1.17996027893162E-15));
#47975=CARTESIAN_POINT('',(2.79695964929222,23.3193623595807,30.6850434229476));
#47976=CARTESIAN_POINT('Ctrl Pts',(2.09999999999999,23.6059783742348,31.0444485374626));
#47977=CARTESIAN_POINT('Ctrl Pts',(2.3323118440126,23.5104433121588,30.9246513587632));
#47978=CARTESIAN_POINT('Ctrl Pts',(2.56464811353468,23.4148979055144,30.8048412083852));
#47979=CARTESIAN_POINT('Ctrl Pts',(2.79695964929222,23.3193623595817,30.6850434229487));
#47980=CARTESIAN_POINT('',(2.79695964929053,9.4511483719124,37.3636232876023));
#47981=CARTESIAN_POINT('Ctrl Pts',(2.79695964929223,9.45114837191225,37.3636232876018));
#47982=CARTESIAN_POINT('Ctrl Pts',(2.5646481138253,9.48524461344982,37.5130086824249));
#47983=CARTESIAN_POINT('Ctrl Pts',(2.33231184461174,9.519344374232,37.6624094960661));
#47984=CARTESIAN_POINT('Ctrl Pts',(2.09999999999999,9.55344044321369,37.8117941348725));
#47985=CARTESIAN_POINT('Origin',(2.79695964928958,0.,-2.35992055786324E-15));
#47986=CARTESIAN_POINT('Origin',(2.44847982464479,0.,-1.17996027893162E-15));
#47987=CARTESIAN_POINT('',(2.79695964929222,-9.451148371912,37.3636232876004));
#47988=CARTESIAN_POINT('Ctrl Pts',(2.1,-9.55344044321368,37.8117941348725));
#47989=CARTESIAN_POINT('Ctrl Pts',(2.33231184276064,-9.51934437450368,37.6624094972564));
#47990=CARTESIAN_POINT('Ctrl Pts',(2.56464811294314,-9.48524461357928,37.5130086829921));
#47991=CARTESIAN_POINT('Ctrl Pts',(2.79695964929223,-9.45114837191225,37.3636232876018));
#47992=CARTESIAN_POINT('',(2.79695964929053,-23.319362359582,30.6850434229491));
#47993=CARTESIAN_POINT('Ctrl Pts',(2.79695964929223,-23.3193623595817,30.6850434229487));
#47994=CARTESIAN_POINT('Ctrl Pts',(2.56464811276728,-23.41489790583,30.804841208781));
#47995=CARTESIAN_POINT('Ctrl Pts',(2.33231184241615,-23.5104433128153,30.9246513595864));
#47996=CARTESIAN_POINT('Ctrl Pts',(2.09999999999999,-23.6059783742348,31.0444485374626));
#47997=CARTESIAN_POINT('Origin',(2.79695964928958,0.,-2.35992055786324E-15));
#47998=CARTESIAN_POINT('Origin',(2.44847982464479,0.,-1.17996027893162E-15));
#47999=CARTESIAN_POINT('',(2.79695964929221,-35.1047516110625,15.9066327376731));
#48000=CARTESIAN_POINT('Ctrl Pts',(2.1,-35.5189237522518,16.1060875286871));
#48001=CARTESIAN_POINT('Ctrl Pts',(2.33231184336733,-35.3808715880817,16.0396051103513));
#48002=CARTESIAN_POINT('Ctrl Pts',(2.56464811322855,-35.2428044749923,15.9731154929954));
#48003=CARTESIAN_POINT('Ctrl Pts',(2.79695964929223,-35.1047516110637,15.9066327376737));
#48004=CARTESIAN_POINT('',(2.79695964929053,-38.529917606008,0.900000000000031));
#48005=CARTESIAN_POINT('Ctrl Pts',(2.79695964929223,-38.5299176060073,0.900000000000005));
#48006=CARTESIAN_POINT('Ctrl Pts',(2.56464811248588,-38.6831447254874,0.900000000000005));
#48007=CARTESIAN_POINT('Ctrl Pts',(2.33231184184216,-38.8363876603691,0.900000000000005));
#48008=CARTESIAN_POINT('Ctrl Pts',(2.09999999999999,-38.98961400168,0.900000000000005));
#48009=CARTESIAN_POINT('Origin',(2.79695964928958,0.,-2.35992055786324E-15));
#48010=CARTESIAN_POINT('Origin',(2.4484798246448,0.,-1.17996027893162E-15));
#48011=CARTESIAN_POINT('',(2.79695964929222,-34.3237608806509,-17.5283766998976));
#48012=CARTESIAN_POINT('Ctrl Pts',(2.1,-34.7379330218401,-17.7278314909114));
#48013=CARTESIAN_POINT('Ctrl Pts',(2.33231184115668,-34.5998808589838,-17.6613490732083));
#48014=CARTESIAN_POINT('Ctrl Pts',(2.56464811214891,-34.4618137452222,-17.5948594555287));
#48015=CARTESIAN_POINT('Ctrl Pts',(2.79695964929223,-34.3237608806521,-17.528376699898));
#48016=CARTESIAN_POINT('',(2.79695964929053,-24.7266590280245,-29.5627617796034));
#48017=CARTESIAN_POINT('Ctrl Pts',(2.79695964929223,-24.726659028024,-29.5627617796028));
#48018=CARTESIAN_POINT('Ctrl Pts',(2.56464811356494,-24.8221945739443,-29.6825595650238));
#48019=CARTESIAN_POINT('Ctrl Pts',(2.332311844067,-24.9177399805788,-29.8023697153893));
#48020=CARTESIAN_POINT('Ctrl Pts',(2.09999999999999,-25.0132750426772,-29.9221668941168));
#48021=CARTESIAN_POINT('Origin',(2.79695964928959,0.,-2.35992055786324E-15));
#48022=CARTESIAN_POINT('Origin',(2.44847982464479,0.,-1.17996027893162E-15));
#48023=CARTESIAN_POINT('',(2.79695964929221,-7.69627812998459,-37.7641609687218));
#48024=CARTESIAN_POINT('Ctrl Pts',(2.1,-7.79857020128637,-38.2123318159937));
#48025=CARTESIAN_POINT('Ctrl Pts',(2.33231183932665,-7.76447413308037,-38.0629471805858));
#48026=CARTESIAN_POINT('Ctrl Pts',(2.56464811125653,-7.73037437189952,-37.9135463651979));
#48027=CARTESIAN_POINT('Ctrl Pts',(2.79695964929222,-7.69627812998494,-37.764160968723));
#48028=CARTESIAN_POINT('',(2.79695964929052,7.69627812998506,-37.7641609687237));
#48029=CARTESIAN_POINT('Ctrl Pts',(2.79695964929222,7.69627812998493,-37.764160968723));
#48030=CARTESIAN_POINT('Ctrl Pts',(2.56464811136644,7.73037437188337,-37.9135463651272));
#48031=CARTESIAN_POINT('Ctrl Pts',(2.33231183953305,7.76447413305006,-38.062947180453));
#48032=CARTESIAN_POINT('Ctrl Pts',(2.1,7.79857020128636,-38.2123318159937));
#48033=CARTESIAN_POINT('Origin',(2.79695964928958,0.,-2.35992055786324E-15));
#48034=CARTESIAN_POINT('Origin',(2.44847982464479,0.,-1.17996027893162E-15));
#48035=CARTESIAN_POINT('',(2.79695964929221,24.7266590280233,-29.5627617796018));
#48036=CARTESIAN_POINT('Ctrl Pts',(2.09999999999998,25.0132750426771,-29.9221668941168));
#48037=CARTESIAN_POINT('Ctrl Pts',(2.33231183679977,24.9177399835673,-29.8023697191368));
#48038=CARTESIAN_POINT('Ctrl Pts',(2.56464811003171,24.8221945753973,-29.6825595668458));
#48039=CARTESIAN_POINT('Ctrl Pts',(2.79695964929221,24.726659028024,-29.5627617796029));
#48040=CARTESIAN_POINT('',(2.79695964929052,34.3237608806527,-17.5283766998984));
#48041=CARTESIAN_POINT('Ctrl Pts',(2.79695964929223,34.3237608806521,-17.5283766998981));
#48042=CARTESIAN_POINT('Ctrl Pts',(2.56464811211474,34.4618137452426,-17.5948594555385));
#48043=CARTESIAN_POINT('Ctrl Pts',(2.33231184104411,34.5998808590507,-17.6613490732405));
#48044=CARTESIAN_POINT('Ctrl Pts',(2.09999999999998,34.7379330218401,-17.7278314909114));
#48045=CARTESIAN_POINT('Origin',(2.79695964928958,0.,-2.35992055786324E-15));
#48046=CARTESIAN_POINT('Origin',(0.15,0.,0.));
#48047=CARTESIAN_POINT('',(0.,3.825,-4.68427400673863E-16));
#48048=CARTESIAN_POINT('Origin',(0.,0.,0.));
#48049=CARTESIAN_POINT('',(0.3,3.525,4.31687996699442E-16));
#48050=CARTESIAN_POINT('',(0.15,3.675,-4.50057698686652E-16));
#48051=CARTESIAN_POINT('',(0.3,-3.525,-4.31687996699442E-16));
#48052=CARTESIAN_POINT('Origin',(0.3,0.,0.));
#48053=CARTESIAN_POINT('Origin',(0.3,0.,0.));
#48054=CARTESIAN_POINT('Origin',(15.5,0.,0.));
#48055=CARTESIAN_POINT('',(30.7,3.525,-4.31687996699442E-16));
#48056=CARTESIAN_POINT('',(30.7,-3.525,-4.31687996699442E-16));
#48057=CARTESIAN_POINT('Origin',(30.7,0.,0.));
#48058=CARTESIAN_POINT('Origin',(30.7,0.,0.));
#48059=CARTESIAN_POINT('',(15.5,-3.525,-4.31687996699442E-16));
#48060=CARTESIAN_POINT('Origin',(0.,38.5,0.));
#48061=CARTESIAN_POINT('',(-1.76941794549634E-15,-38.5,-4.71489017671731E-15));
#48062=CARTESIAN_POINT('Origin',(0.,0.,0.));
#48063=CARTESIAN_POINT('Origin',(30.85,0.,0.));
#48064=CARTESIAN_POINT('',(31.,3.825,4.68427400673863E-16));
#48065=CARTESIAN_POINT('',(30.85,3.675,-4.50057698686652E-16));
#48066=CARTESIAN_POINT('Origin',(31.,0.,0.));
#48067=CARTESIAN_POINT('Origin',(31.,3.525,0.));
#48068=CARTESIAN_POINT('',(31.,-8.1,-9.91963907309356E-16));
#48069=CARTESIAN_POINT('Origin',(31.,0.,0.));
#48070=CARTESIAN_POINT('Ctrl Pts',(2.09999999999999,14.6112236547299,-6.03746982408084));
#48071=CARTESIAN_POINT('Ctrl Pts',(2.73333333333332,14.6112236547299,-6.03746982408084));
#48072=CARTESIAN_POINT('Ctrl Pts',(3.36597343453743,14.6111769235222,-6.03754613131406));
#48073=CARTESIAN_POINT('Ctrl Pts',(4.12348633489348,14.6111625044228,-6.03756948056199));
#48074=CARTESIAN_POINT('Ctrl Pts',(4.36308027105789,14.6119257809318,-6.03577528532447));
#48075=CARTESIAN_POINT('Ctrl Pts',(4.85756641340223,14.6154583824993,-6.02750324329286));
#48076=CARTESIAN_POINT('Ctrl Pts',(5.73898730352466,14.6238809423774,-6.00782933213849));
#48077=CARTESIAN_POINT('Ctrl Pts',(6.52605696873204,14.624130981059,-6.00728042336119));
#48078=CARTESIAN_POINT('Ctrl Pts',(7.12756844447777,14.6083641562831,-6.04373935409524));
#48079=CARTESIAN_POINT('Ctrl Pts',(7.25506380614844,14.6049954548641,-6.05175896636988));
#48080=CARTESIAN_POINT('Ctrl Pts',(7.51732261094449,14.5977124647127,-6.06955193187746));
#48081=CARTESIAN_POINT('Ctrl Pts',(7.84589041574969,14.587687697552,-6.09468228112985));
#48082=CARTESIAN_POINT('Ctrl Pts',(8.24416928267873,14.5733864041206,-6.13057543333643));
#48083=CARTESIAN_POINT('Ctrl Pts',(8.77646956832262,14.5502471322405,-6.18743923585914));
#48084=CARTESIAN_POINT('Ctrl Pts',(9.44114040292177,14.5118316236054,-6.2778654600114));
#48085=CARTESIAN_POINT('Ctrl Pts',(9.96389116987696,14.4664252137994,-6.37698251721559));
#48086=CARTESIAN_POINT('Ctrl Pts',(11.1189200235608,14.3421195663292,-6.63780334583202));
#48087=CARTESIAN_POINT('Ctrl Pts',(12.080462017836,14.1753483064828,-7.00505140121598));
#48088=CARTESIAN_POINT('Ctrl Pts',(13.000848435547,13.9645576242428,-7.40476609777859));
#48089=CARTESIAN_POINT('Ctrl Pts',(13.2108249725339,13.9139023822834,-7.49752063559415));
#48090=CARTESIAN_POINT('Ctrl Pts',(13.3144480846626,13.8882765069648,-7.54353000870038));
#48091=CARTESIAN_POINT('Ctrl Pts',(13.3733279376354,13.8735399120439,-7.56972314538053));
#48092=CARTESIAN_POINT('Ctrl Pts',(13.4026071886664,13.866154080108,-7.58276112712036));
#48093=CARTESIAN_POINT('Ctrl Pts',(13.6877972600753,13.7939115032282,-7.70979028654145));
#48094=CARTESIAN_POINT('Ctrl Pts',(14.2465878522009,13.6358858928993,-7.98289947471341));
#48095=CARTESIAN_POINT('Ctrl Pts',(14.7537307590314,13.4638747656086,-8.2672884323285));
#48096=CARTESIAN_POINT('Ctrl Pts',(14.9999999999997,13.3740441878645,-8.41111991756525));
#48097=CARTESIAN_POINT('Ctrl Pts',(2.09999999999999,21.5804981880614,-9.39369555083498));
#48098=CARTESIAN_POINT('Ctrl Pts',(2.73333333333332,21.5804981880614,-9.39369555083498));
#48099=CARTESIAN_POINT('Ctrl Pts',(3.36558891350101,21.5804658214384,-9.39375443622592));
#48100=CARTESIAN_POINT('Ctrl Pts',(4.12268626532888,21.5804565789739,-9.39377109990644));
#48101=CARTESIAN_POINT('Ctrl Pts',(4.35700014090232,21.5816310465459,-9.39115328711438));
#48102=CARTESIAN_POINT('Ctrl Pts',(4.84800441917692,21.5871007298261,-9.37899529561417));
#48103=CARTESIAN_POINT('Ctrl Pts',(5.73069087778663,21.6002069847704,-9.34990650206829));
#48104=CARTESIAN_POINT('Ctrl Pts',(6.53595444290035,21.600798556951,-9.34867422602377));
#48105=CARTESIAN_POINT('Ctrl Pts',(7.15870824265195,21.5757953532485,-9.40377866208819));
#48106=CARTESIAN_POINT('Ctrl Pts',(7.28653324723265,21.57054842124,-9.41564402172901));
#48107=CARTESIAN_POINT('Ctrl Pts',(7.55249732957637,21.559112869562,-9.44216595644569));
#48108=CARTESIAN_POINT('Ctrl Pts',(7.88542376807474,21.5433748133556,-9.47959115917565));
#48109=CARTESIAN_POINT('Ctrl Pts',(8.29077837198509,21.5208373497423,-9.53321806687483));
#48110=CARTESIAN_POINT('Ctrl Pts',(8.83404956052536,21.4843659597635,-9.61829685598639));
#48111=CARTESIAN_POINT('Ctrl Pts',(9.5159951101198,21.4237193349165,-9.75404701204542));
#48112=CARTESIAN_POINT('Ctrl Pts',(10.0563165509726,21.3519772919284,-9.90350937303449));
#48113=CARTESIAN_POINT('Ctrl Pts',(11.2545453599662,21.1552727776615,-10.2981908568203));
#48114=CARTESIAN_POINT('Ctrl Pts',(12.2342091233032,20.8928382426908,-10.8482812877152));
#48115=CARTESIAN_POINT('Ctrl Pts',(13.1608025627428,20.5657221228123,-11.4401088273015));
#48116=CARTESIAN_POINT('Ctrl Pts',(13.3719027697888,20.4872597464373,-11.5772900925882));
#48117=CARTESIAN_POINT('Ctrl Pts',(13.4759508814436,20.4476142846892,-11.645264020493));
#48118=CARTESIAN_POINT('Ctrl Pts',(13.5350545696212,20.4248270188077,-11.6839493266396));
#48119=CARTESIAN_POINT('Ctrl Pts',(13.5644244680613,20.4134100716287,-11.7031984428001));
#48120=CARTESIAN_POINT('Ctrl Pts',(13.8509114235667,20.3017947915021,-11.8907413232488));
#48121=CARTESIAN_POINT('Ctrl Pts',(14.415914571976,20.056573473436,-12.2967435659359));
#48122=CARTESIAN_POINT('Ctrl Pts',(14.9236315787721,19.7920103236355,-12.7155432366557));
#48123=CARTESIAN_POINT('Ctrl Pts',(15.169681381964,19.6539784037027,-12.9272062682979));
#48124=CARTESIAN_POINT('Ctrl Pts',(2.09999999999999,28.5497727213929,-12.7499212775891));
#48125=CARTESIAN_POINT('Ctrl Pts',(2.73333333333333,28.5497727213929,-12.7499212775891));
#48126=CARTESIAN_POINT('Ctrl Pts',(3.36511943232413,28.5497117328892,-12.7500211136887));
#48127=CARTESIAN_POINT('Ctrl Pts',(4.12177605163342,28.5496942241346,-12.7500491269374));
#48128=CARTESIAN_POINT('Ctrl Pts',(4.35079752926905,28.5512513366179,-12.7466643375223));
#48129=CARTESIAN_POINT('Ctrl Pts',(4.83833431769655,28.5586001656638,-12.7307346947286));
#48130=CARTESIAN_POINT('Ctrl Pts',(5.72217414447527,28.5763905635329,-12.6922206715534));
#48131=CARTESIAN_POINT('Ctrl Pts',(6.54572412381037,28.5774814580578,-12.6899292527909));
#48132=CARTESIAN_POINT('Ctrl Pts',(7.18904210034709,28.5423219642133,-12.7655627019458));
#48133=CARTESIAN_POINT('Ctrl Pts',(7.31718028521341,28.5351786226866,-12.7813084572508));
#48134=CARTESIAN_POINT('Ctrl Pts',(7.58671228378742,28.5194164265744,-12.8169133627186));
#48135=CARTESIAN_POINT('Ctrl Pts',(7.92374360970041,28.4977092314406,-12.8671381009231));
#48136=CARTESIAN_POINT('Ctrl Pts',(8.33571576942014,28.4664978281724,-12.9393795360026));
#48137=CARTESIAN_POINT('Ctrl Pts',(8.88882961906569,28.4158479121591,-13.0543369931349));
#48138=CARTESIAN_POINT('Ctrl Pts',(9.58537985183176,28.3313660942903,-13.2385440053529));
#48139=CARTESIAN_POINT('Ctrl Pts',(10.1375678596739,28.2311944046601,-13.4422863994001));
#48140=CARTESIAN_POINT('Ctrl Pts',(11.3565453181114,27.957090325248,-13.9798088000628));
#48141=CARTESIAN_POINT('Ctrl Pts',(12.3228303493508,27.6006442853792,-14.7079674952598));
#48142=CARTESIAN_POINT('Ctrl Pts',(13.2438483912537,27.1599995484332,-15.4865968272217));
#48143=CARTESIAN_POINT('Ctrl Pts',(13.4536944920046,27.0542012023204,-15.6672854112189));
#48144=CARTESIAN_POINT('Ctrl Pts',(13.5572580689388,27.0007587325336,-15.7568001585971));
#48145=CARTESIAN_POINT('Ctrl Pts',(13.6160973314722,26.9700347789253,-15.8077582507674));
#48146=CARTESIAN_POINT('Ctrl Pts',(13.6453544897111,26.9546407543076,-15.8331157119274));
#48147=CARTESIAN_POINT('Ctrl Pts',(13.9304416541416,26.8041428578028,-16.0801826875383));
#48148=CARTESIAN_POINT('Ctrl Pts',(14.483478725475,26.4781781617783,-16.6086828302805));
#48149=CARTESIAN_POINT('Ctrl Pts',(14.98335392639,26.1263733010219,-17.1544773738691));
#48150=CARTESIAN_POINT('Ctrl Pts',(15.2260186760796,25.9428548705627,-17.4304534957912));
#48151=CARTESIAN_POINT('Ctrl Pts',(2.09999999999999,35.5190472547244,-16.1061470043432));
#48152=CARTESIAN_POINT('Ctrl Pts',(2.73333333333332,35.5190472547244,-16.1061470043432));
#48153=CARTESIAN_POINT('Ctrl Pts',(3.36464113820893,35.5189727539756,-16.1062575345791));
#48154=CARTESIAN_POINT('Ctrl Pts',(4.12085892726248,35.5189516907951,-16.1062875245081));
#48155=CARTESIAN_POINT('Ctrl Pts',(4.34457524717165,35.5208691650184,-16.1021819509952));
#48156=CARTESIAN_POINT('Ctrl Pts',(4.82871845463999,35.5300474198351,-16.0825848866187));
#48157=CARTESIAN_POINT('Ctrl Pts',(5.71350765111191,35.5525576262045,-16.0345705772587));
#48158=CARTESIAN_POINT('Ctrl Pts',(6.55584676521418,35.554338196091,-16.0308300205147));
#48159=CARTESIAN_POINT('Ctrl Pts',(7.21833787782939,35.5083038396895,-16.1284788337185));
#48160=CARTESIAN_POINT('Ctrl Pts',(7.346759957141,35.4992519242509,-16.1481285109658));
#48161=CARTESIAN_POINT('Ctrl Pts',(7.61957159600264,35.4790301677304,-16.1930875893086));
#48162=CARTESIAN_POINT('Ctrl Pts',(7.96026026202707,35.4511934320212,-16.2564362933882));
#48163=CARTESIAN_POINT('Ctrl Pts',(8.37794277256449,35.4110314107648,-16.3478471230923));
#48164=CARTESIAN_POINT('Ctrl Pts',(8.9389782770839,35.3458167429133,-16.4934464019928));
#48165=CARTESIAN_POINT('Ctrl Pts',(9.64589477564363,35.2370478008634,-16.7269630290823));
#48166=CARTESIAN_POINT('Ctrl Pts',(10.2035813464951,35.108934215722,-16.9839479337664));
#48167=CARTESIAN_POINT('Ctrl Pts',(11.4269751522422,34.7615504456458,-17.6561879421533));
#48168=CARTESIAN_POINT('Ctrl Pts',(12.379460225573,34.3187345767276,-18.5489901686144));
#48169=CARTESIAN_POINT('Ctrl Pts',(13.2972790827102,33.7671525002472,-19.5115445485323));
#48170=CARTESIAN_POINT('Ctrl Pts',(13.5062482901107,33.6346179543458,-19.7350483549094));
#48171=CARTESIAN_POINT('Ctrl Pts',(13.609520849881,33.5676140087591,-19.8458826806856));
#48172=CARTESIAN_POINT('Ctrl Pts',(13.6681938694708,33.5290848496294,-19.9089910815554));
#48173=CARTESIAN_POINT('Ctrl Pts',(13.6973863580761,33.5097717745622,-19.9404093800206));
#48174=CARTESIAN_POINT('Ctrl Pts',(13.9814817294285,33.3210758935383,-20.246334342403));
#48175=CARTESIAN_POINT('Ctrl Pts',(14.5280929602068,32.9176301874376,-20.8932115622066));
#48176=CARTESIAN_POINT('Ctrl Pts',(15.0243070371674,32.4796582872443,-21.5656339098325));
#48177=CARTESIAN_POINT('Ctrl Pts',(15.2656150130537,32.2510375008716,-21.9059812809209));
#48178=CARTESIAN_POINT('',(3.2,34.2572188230213,-15.4984824583453));
#48179=CARTESIAN_POINT('Ctrl Pts',(3.19847278576198,34.2571711264119,-15.4985541028447));
#48180=CARTESIAN_POINT('Ctrl Pts',(3.06436527352304,34.5398342174301,-15.634660914804));
#48181=CARTESIAN_POINT('Ctrl Pts',(2.93026063537424,34.8224448608797,-15.7707419629102));
#48182=CARTESIAN_POINT('Ctrl Pts',(2.79626448778338,35.1047282825352,-15.9066674709291));
#48183=CARTESIAN_POINT('',(15.,13.3740441878754,-8.41111991757311));
#48184=CARTESIAN_POINT('Ctrl Pts',(15.,13.3740441878754,-8.4111199175731));
#48185=CARTESIAN_POINT('Ctrl Pts',(14.489716577952,14.0152467731085,-8.4300414728713));
#48186=CARTESIAN_POINT('Ctrl Pts',(13.9833803026617,14.6726092024603,-8.46600373582148));
#48187=CARTESIAN_POINT('Ctrl Pts',(13.4460287676664,15.3890150736474,-8.54665853696435));
#48188=CARTESIAN_POINT('Ctrl Pts',(12.8282655681106,16.2126270936056,-8.63938287991053));
#48189=CARTESIAN_POINT('Ctrl Pts',(12.15554140896,17.1699136521334,-8.74804283511199));
#48190=CARTESIAN_POINT('Ctrl Pts',(11.5904908073768,18.0034501560149,-8.88551170505054));
#48191=CARTESIAN_POINT('Ctrl Pts',(11.1143368259707,18.7058504788506,-9.00135327668543));
#48192=CARTESIAN_POINT('Ctrl Pts',(10.6953158949628,19.3440146215797,-9.13525382272217));
#48193=CARTESIAN_POINT('Ctrl Pts',(10.2957959918397,19.9646028342318,-9.29767556265455));
#48194=CARTESIAN_POINT('Ctrl Pts',(10.0450888109117,20.3540350504866,-9.39959863637766));
#48195=CARTESIAN_POINT('Ctrl Pts',(9.80235305575949,20.7368803031962,-9.51197737039024));
#48196=CARTESIAN_POINT('Ctrl Pts',(9.56010106225058,21.126456560068,-9.63522432833226));
#48197=CARTESIAN_POINT('Ctrl Pts',(9.36613602928155,21.4383803977775,-9.73390504469829));
#48198=CARTESIAN_POINT('Ctrl Pts',(9.15248571275793,21.7859099736338,-9.84905754737758));
#48199=CARTESIAN_POINT('Ctrl Pts',(8.89022359798878,22.224537051038,-10.0043869244452));
#48200=CARTESIAN_POINT('Ctrl Pts',(8.39222406084267,23.0574292959559,-10.2993359602714));
#48201=CARTESIAN_POINT('Ctrl Pts',(7.76643777362598,24.1441485719301,-10.7202076897158));
#48202=CARTESIAN_POINT('Ctrl Pts',(7.10363554123529,25.4084375301613,-11.2437787818133));
#48203=CARTESIAN_POINT('Ctrl Pts',(6.23550018248562,27.0643974751934,-11.9295498243014));
#48204=CARTESIAN_POINT('Ctrl Pts',(5.31040885822318,28.970129103298,-12.9104863534632));
#48205=CARTESIAN_POINT('Ctrl Pts',(4.4641661690363,30.9938896521179,-13.9169531085495));
#48206=CARTESIAN_POINT('Ctrl Pts',(4.30741751124025,31.3687487247947,-14.1033799043044));
#48207=CARTESIAN_POINT('Ctrl Pts',(4.15262292088818,31.7490527468619,-14.2906133363129));
#48208=CARTESIAN_POINT('Ctrl Pts',(4.,32.1353158291841,-14.4766278329416));
#48209=CARTESIAN_POINT('Ctrl Pts',(3.72434973283399,32.832940545176,-14.8125861896161));
#48210=CARTESIAN_POINT('Ctrl Pts',(3.45587123478805,33.5452450424059,-15.1556139563445));
#48211=CARTESIAN_POINT('Ctrl Pts',(3.2,34.2572188230213,-15.4984824583453));
#48212=CARTESIAN_POINT('',(15.,25.5672208319352,-16.8130074326712));
#48213=CARTESIAN_POINT('Ctrl Pts',(15.,25.5672208319352,-16.8130074326712));
#48214=CARTESIAN_POINT('Ctrl Pts',(15.,21.9230552541059,-14.3215404573318));
#48215=CARTESIAN_POINT('Ctrl Pts',(15.,17.6025615780812,-11.3562169657429));
#48216=CARTESIAN_POINT('Ctrl Pts',(15.,13.3740441878754,-8.4111199175731));
#48217=CARTESIAN_POINT('Ctrl Pts',(6.,35.548403009865,-16.0409177869666));
#48218=CARTESIAN_POINT('Ctrl Pts',(6.38595465246567,35.0644728080463,-15.8087503789144));
#48219=CARTESIAN_POINT('Ctrl Pts',(6.7702364866826,34.6013428262183,-15.6121364414844));
#48220=CARTESIAN_POINT('Ctrl Pts',(7.13915213286206,34.1637499212586,-15.4654822405443));
#48221=CARTESIAN_POINT('Ctrl Pts',(8.10667920093238,33.0161082185314,-15.0808633973879));
#48222=CARTESIAN_POINT('Ctrl Pts',(8.9801988874737,32.1046384518045,-14.8985993430622));
#48223=CARTESIAN_POINT('Ctrl Pts',(9.46656009721077,31.5983922040242,-14.8470136927622));
#48224=CARTESIAN_POINT('Ctrl Pts',(9.65648624874913,31.4007008593061,-14.8268692736762));
#48225=CARTESIAN_POINT('Ctrl Pts',(9.79228848853731,31.2605649744979,-14.8192547892488));
#48226=CARTESIAN_POINT('Ctrl Pts',(9.9459382572782,31.1021220893961,-14.8158457576554));
#48227=CARTESIAN_POINT('Ctrl Pts',(10.1065740866009,30.9364752130151,-14.812281726146));
#48228=CARTESIAN_POINT('Ctrl Pts',(10.2660951669675,30.7723740544135,-14.8158872980242));
#48229=CARTESIAN_POINT('Ctrl Pts',(10.4261869573616,30.6070683865717,-14.8277509886845));
#48230=CARTESIAN_POINT('Ctrl Pts',(10.8065549509411,30.2143125491269,-14.855938369198));
#48231=CARTESIAN_POINT('Ctrl Pts',(11.1894211925257,29.814522907984,-14.9318211767803));
#48232=CARTESIAN_POINT('Ctrl Pts',(11.6023503255242,29.3751640250925,-15.0597901114669));
#48233=CARTESIAN_POINT('Ctrl Pts',(11.7531893954247,29.2146704198904,-15.1065359415422));
#48234=CARTESIAN_POINT('Ctrl Pts',(11.9080270687775,29.0488883179913,-15.160381650937));
#48235=CARTESIAN_POINT('Ctrl Pts',(12.0681766131679,28.8762440451095,-15.2218090966442));
#48236=CARTESIAN_POINT('Ctrl Pts',(12.1838435903474,28.7515528307349,-15.2661746737544));
#48237=CARTESIAN_POINT('Ctrl Pts',(12.3100865410161,28.615150802675,-15.3162188040206));
#48238=CARTESIAN_POINT('Ctrl Pts',(12.5127093730712,28.3942307654713,-15.40558106561));
#48239=CARTESIAN_POINT('Ctrl Pts',(12.7975492664042,28.0836693188959,-15.5312033205206));
#48240=CARTESIAN_POINT('Ctrl Pts',(13.1874566943566,27.6537578160352,-15.7216404803685));
#48241=CARTESIAN_POINT('Ctrl Pts',(13.6431584568239,27.1503653567254,-15.9585907359883));
#48242=CARTESIAN_POINT('Ctrl Pts',(14.069523646534,26.6793796395533,-16.1802869175923));
#48243=CARTESIAN_POINT('Ctrl Pts',(14.53311408767,26.1415317826733,-16.4743245564268));
#48244=CARTESIAN_POINT('Ctrl Pts',(15.,25.5672208319352,-16.8130074326712));
#48245=CARTESIAN_POINT('Origin',(15.,5.29966331579923,-6.64556760097826));
#48246=CARTESIAN_POINT('',(15.,12.0570237116074,-10.2098078054769));
#48247=CARTESIAN_POINT('Ctrl Pts',(15.,12.0570237116074,-10.2098078054769));
#48248=CARTESIAN_POINT('Ctrl Pts',(15.,12.5369574853615,-9.64304171150107));
#48249=CARTESIAN_POINT('Ctrl Pts',(15.,12.9772113127979,-9.04210133960708));
#48250=CARTESIAN_POINT('Ctrl Pts',(15.,13.3740441878754,-8.41111991757311));
#48251=CARTESIAN_POINT('',(15.,23.7252887774277,-19.3253893215031));
#48252=CARTESIAN_POINT('Ctrl Pts',(15.,12.0570237116074,-10.2098078054769));
#48253=CARTESIAN_POINT('Ctrl Pts',(15.,16.2510705543726,-13.4474144076022));
#48254=CARTESIAN_POINT('Ctrl Pts',(15.,20.4525997527948,-16.7472443383594));
#48255=CARTESIAN_POINT('Ctrl Pts',(15.,23.7252887774277,-19.325389321503));
#48256=CARTESIAN_POINT('Origin',(15.,0.,0.));
#48257=CARTESIAN_POINT('Ctrl Pts',(15.,19.0787879368772,-23.9240433635217));
#48258=CARTESIAN_POINT('Ctrl Pts',(15.,43.0028313003989,-4.84525542664447));
#48259=CARTESIAN_POINT('Ctrl Pts',(15.,23.9240433635217,19.0787879368772));
#48260=CARTESIAN_POINT('Ctrl Pts',(15.,4.84525542664447,43.0028313003989));
#48261=CARTESIAN_POINT('Ctrl Pts',(15.,-19.0787879368772,23.9240433635217));
#48262=CARTESIAN_POINT('Ctrl Pts',(15.,-43.0028313003989,4.84525542664447));
#48263=CARTESIAN_POINT('Ctrl Pts',(15.,-23.9240433635217,-19.0787879368772));
#48264=CARTESIAN_POINT('Ctrl Pts',(15.,-4.84525542664447,-43.0028313003989));
#48265=CARTESIAN_POINT('Ctrl Pts',(15.,19.0787879368772,-23.9240433635217));
#48266=CARTESIAN_POINT('Ctrl Pts',(14.7843073131059,19.1634046954076,-24.0301494226203));
#48267=CARTESIAN_POINT('Ctrl Pts',(14.7843073131059,43.1935541180279,-4.86674472721276));
#48268=CARTESIAN_POINT('Ctrl Pts',(14.7843073131059,24.0301494226203,19.1634046954076));
#48269=CARTESIAN_POINT('Ctrl Pts',(14.7843073131059,4.86674472721276,43.1935541180279));
#48270=CARTESIAN_POINT('Ctrl Pts',(14.7843073131059,-19.1634046954076,24.0301494226203));
#48271=CARTESIAN_POINT('Ctrl Pts',(14.7843073131059,-43.1935541180279,4.86674472721276));
#48272=CARTESIAN_POINT('Ctrl Pts',(14.7843073131059,-24.0301494226203,-19.1634046954076));
#48273=CARTESIAN_POINT('Ctrl Pts',(14.7843073131059,-4.86674472721276,-43.1935541180279));
#48274=CARTESIAN_POINT('Ctrl Pts',(14.7843073131059,19.1634046954076,-24.0301494226203));
#48275=CARTESIAN_POINT('Ctrl Pts',(14.3560298066371,19.3343909497437,-24.2445594038433));
#48276=CARTESIAN_POINT('Ctrl Pts',(14.3560298066371,43.578950353587,-4.91016845409964));
#48277=CARTESIAN_POINT('Ctrl Pts',(14.3560298066371,24.2445594038433,19.3343909497437));
#48278=CARTESIAN_POINT('Ctrl Pts',(14.3560298066371,4.91016845409964,43.578950353587));
#48279=CARTESIAN_POINT('Ctrl Pts',(14.3560298066371,-19.3343909497437,24.2445594038433));
#48280=CARTESIAN_POINT('Ctrl Pts',(14.3560298066371,-43.578950353587,4.91016845409964));
#48281=CARTESIAN_POINT('Ctrl Pts',(14.3560298066371,-24.2445594038433,-19.3343909497437));
#48282=CARTESIAN_POINT('Ctrl Pts',(14.3560298066371,-4.91016845409964,-43.578950353587));
#48283=CARTESIAN_POINT('Ctrl Pts',(14.3560298066371,19.3343909497437,-24.2445594038433));
#48284=CARTESIAN_POINT('Ctrl Pts',(13.722936818686,19.5961283568486,-24.5727677312355));
#48285=CARTESIAN_POINT('Ctrl Pts',(13.722936818686,44.1688960880841,-4.97663937438695));
#48286=CARTESIAN_POINT('Ctrl Pts',(13.722936818686,24.5727677312355,19.5961283568486));
#48287=CARTESIAN_POINT('Ctrl Pts',(13.722936818686,4.97663937438695,44.1688960880841));
#48288=CARTESIAN_POINT('Ctrl Pts',(13.722936818686,-19.5961283568486,24.5727677312355));
#48289=CARTESIAN_POINT('Ctrl Pts',(13.722936818686,-44.1688960880841,4.97663937438695));
#48290=CARTESIAN_POINT('Ctrl Pts',(13.722936818686,-24.5727677312355,-19.5961283568486));
#48291=CARTESIAN_POINT('Ctrl Pts',(13.722936818686,-4.97663937438695,-44.1688960880841));
#48292=CARTESIAN_POINT('Ctrl Pts',(13.722936818686,19.5961283568486,-24.5727677312355));
#48293=CARTESIAN_POINT('Ctrl Pts',(12.8977690042853,19.9558022366521,-25.0237845110024));
#48294=CARTESIAN_POINT('Ctrl Pts',(12.8977690042853,44.9795867476544,-5.06798227435031));
#48295=CARTESIAN_POINT('Ctrl Pts',(12.8977690042853,25.0237845110024,19.9558022366521));
#48296=CARTESIAN_POINT('Ctrl Pts',(12.8977690042853,5.06798227435031,44.9795867476544));
#48297=CARTESIAN_POINT('Ctrl Pts',(12.8977690042853,-19.9558022366521,25.0237845110024));
#48298=CARTESIAN_POINT('Ctrl Pts',(12.8977690042853,-44.9795867476544,5.06798227435031));
#48299=CARTESIAN_POINT('Ctrl Pts',(12.8977690042853,-25.0237845110024,-19.9558022366521));
#48300=CARTESIAN_POINT('Ctrl Pts',(12.8977690042853,-5.06798227435031,-44.9795867476544));
#48301=CARTESIAN_POINT('Ctrl Pts',(12.8977690042853,19.9558022366521,-25.0237845110024));
#48302=CARTESIAN_POINT('Ctrl Pts',(11.9000549946031,20.4244261094473,-25.6114202607695));
#48303=CARTESIAN_POINT('Ctrl Pts',(11.9000549946031,46.0358463702168,-5.18699415132219));
#48304=CARTESIAN_POINT('Ctrl Pts',(11.9000549946031,25.6114202607695,20.4244261094473));
#48305=CARTESIAN_POINT('Ctrl Pts',(11.9000549946031,5.18699415132219,46.0358463702168));
#48306=CARTESIAN_POINT('Ctrl Pts',(11.9000549946031,-20.4244261094473,25.6114202607695));
#48307=CARTESIAN_POINT('Ctrl Pts',(11.9000549946031,-46.0358463702168,5.18699415132219));
#48308=CARTESIAN_POINT('Ctrl Pts',(11.9000549946031,-25.6114202607695,-20.4244261094473));
#48309=CARTESIAN_POINT('Ctrl Pts',(11.9000549946031,-5.18699415132219,-46.0358463702168));
#48310=CARTESIAN_POINT('Ctrl Pts',(11.9000549946031,20.4244261094473,-25.6114202607695));
#48311=CARTESIAN_POINT('Ctrl Pts',(10.9391333834985,20.9137997124663,-26.2250753492544));
#48312=CARTESIAN_POINT('Ctrl Pts',(10.9391333834985,47.1388750617207,-5.3112756367881));
#48313=CARTESIAN_POINT('Ctrl Pts',(10.9391333834985,26.2250753492544,20.9137997124663));
#48314=CARTESIAN_POINT('Ctrl Pts',(10.9391333834985,5.3112756367881,47.1388750617207));
#48315=CARTESIAN_POINT('Ctrl Pts',(10.9391333834985,-20.9137997124663,26.2250753492544));
#48316=CARTESIAN_POINT('Ctrl Pts',(10.9391333834985,-47.1388750617207,5.3112756367881));
#48317=CARTESIAN_POINT('Ctrl Pts',(10.9391333834985,-26.2250753492544,-20.9137997124663));
#48318=CARTESIAN_POINT('Ctrl Pts',(10.9391333834985,-5.3112756367881,-47.1388750617207));
#48319=CARTESIAN_POINT('Ctrl Pts',(10.9391333834985,20.9137997124663,-26.2250753492544));
#48320=CARTESIAN_POINT('Ctrl Pts',(10.0180552497783,21.4256437560905,-26.8669074790281));
#48321=CARTESIAN_POINT('Ctrl Pts',(10.0180552497783,48.2925512351186,-5.44126372293756));
#48322=CARTESIAN_POINT('Ctrl Pts',(10.0180552497783,26.8669074790281,21.4256437560905));
#48323=CARTESIAN_POINT('Ctrl Pts',(10.0180552497783,5.44126372293756,48.2925512351186));
#48324=CARTESIAN_POINT('Ctrl Pts',(10.0180552497783,-21.4256437560905,26.8669074790281));
#48325=CARTESIAN_POINT('Ctrl Pts',(10.0180552497783,-48.2925512351186,5.44126372293756));
#48326=CARTESIAN_POINT('Ctrl Pts',(10.0180552497783,-26.8669074790281,-21.4256437560905));
#48327=CARTESIAN_POINT('Ctrl Pts',(10.0180552497783,-5.44126372293756,-48.2925512351186));
#48328=CARTESIAN_POINT('Ctrl Pts',(10.0180552497783,21.4256437560905,-26.8669074790281));
#48329=CARTESIAN_POINT('Ctrl Pts',(9.13857394886632,21.9609470764246,-27.5381566113461));
#48330=CARTESIAN_POINT('Ctrl Pts',(9.13857394886632,49.4991036877707,-5.57720953492157));
#48331=CARTESIAN_POINT('Ctrl Pts',(9.13857394886632,27.5381566113461,21.9609470764246));
#48332=CARTESIAN_POINT('Ctrl Pts',(9.13857394886632,5.57720953492157,49.4991036877707));
#48333=CARTESIAN_POINT('Ctrl Pts',(9.13857394886632,-21.9609470764246,27.5381566113461));
#48334=CARTESIAN_POINT('Ctrl Pts',(9.13857394886632,-49.4991036877707,5.57720953492157));
#48335=CARTESIAN_POINT('Ctrl Pts',(9.13857394886632,-27.5381566113461,-21.9609470764246));
#48336=CARTESIAN_POINT('Ctrl Pts',(9.13857394886632,-5.57720953492157,-49.4991036877707));
#48337=CARTESIAN_POINT('Ctrl Pts',(9.13857394886632,21.9609470764246,-27.5381566113461));
#48338=CARTESIAN_POINT('Ctrl Pts',(8.29915429043693,22.5188438754702,-28.2377370698584));
#48339=CARTESIAN_POINT('Ctrl Pts',(8.29915429043693,50.7565809453286,-5.71889319438814));
#48340=CARTESIAN_POINT('Ctrl Pts',(8.29915429043693,28.2377370698584,22.5188438754702));
#48341=CARTESIAN_POINT('Ctrl Pts',(8.29915429043693,5.71889319438814,50.7565809453286));
#48342=CARTESIAN_POINT('Ctrl Pts',(8.29915429043693,-22.5188438754702,28.2377370698584));
#48343=CARTESIAN_POINT('Ctrl Pts',(8.29915429043693,-50.7565809453286,5.71889319438814));
#48344=CARTESIAN_POINT('Ctrl Pts',(8.29915429043693,-28.2377370698584,-22.5188438754702));
#48345=CARTESIAN_POINT('Ctrl Pts',(8.29915429043693,-5.71889319438814,-50.7565809453286));
#48346=CARTESIAN_POINT('Ctrl Pts',(8.29915429043693,22.5188438754702,-28.2377370698584));
#48347=CARTESIAN_POINT('Ctrl Pts',(7.4968190344241,23.0976550855257,-28.9635433702624));
#48348=CARTESIAN_POINT('Ctrl Pts',(7.4968190344241,52.0611984557881,-5.86588828473677));
#48349=CARTESIAN_POINT('Ctrl Pts',(7.4968190344241,28.9635433702624,23.0976550855257));
#48350=CARTESIAN_POINT('Ctrl Pts',(7.4968190344241,5.86588828473677,52.0611984557881));
#48351=CARTESIAN_POINT('Ctrl Pts',(7.4968190344241,-23.0976550855257,28.9635433702624));
#48352=CARTESIAN_POINT('Ctrl Pts',(7.4968190344241,-52.0611984557881,5.86588828473677));
#48353=CARTESIAN_POINT('Ctrl Pts',(7.4968190344241,-28.9635433702624,-23.0976550855257));
#48354=CARTESIAN_POINT('Ctrl Pts',(7.4968190344241,-5.86588828473677,-52.0611984557881));
#48355=CARTESIAN_POINT('Ctrl Pts',(7.4968190344241,23.0976550855257,-28.9635433702624));
#48356=CARTESIAN_POINT('Ctrl Pts',(6.88220761950379,23.5760760069919,-29.5634642304892));
#48357=CARTESIAN_POINT('Ctrl Pts',(6.88220761950379,53.1395402374811,-5.98738822349725));
#48358=CARTESIAN_POINT('Ctrl Pts',(6.88220761950379,29.5634642304892,23.5760760069919));
#48359=CARTESIAN_POINT('Ctrl Pts',(6.88220761950379,5.98738822349725,53.1395402374811));
#48360=CARTESIAN_POINT('Ctrl Pts',(6.88220761950379,-23.5760760069919,29.5634642304892));
#48361=CARTESIAN_POINT('Ctrl Pts',(6.88220761950379,-53.1395402374811,5.98738822349725));
#48362=CARTESIAN_POINT('Ctrl Pts',(6.88220761950379,-29.5634642304892,-23.5760760069919));
#48363=CARTESIAN_POINT('Ctrl Pts',(6.88220761950379,-5.98738822349725,-53.1395402374811));
#48364=CARTESIAN_POINT('Ctrl Pts',(6.88220761950379,23.5760760069919,-29.5634642304892));
#48365=CARTESIAN_POINT('Ctrl Pts',(6.43560997955544,23.9429907960904,-30.0235608233205));
#48366=CARTESIAN_POINT('Ctrl Pts',(6.43560997955544,53.9665516194108,-6.08057002723013));
#48367=CARTESIAN_POINT('Ctrl Pts',(6.43560997955544,30.0235608233205,23.9429907960904));
#48368=CARTESIAN_POINT('Ctrl Pts',(6.43560997955544,6.08057002723013,53.9665516194108));
#48369=CARTESIAN_POINT('Ctrl Pts',(6.43560997955544,-23.9429907960904,30.0235608233205));
#48370=CARTESIAN_POINT('Ctrl Pts',(6.43560997955544,-53.9665516194108,6.08057002723013));
#48371=CARTESIAN_POINT('Ctrl Pts',(6.43560997955544,-30.0235608233205,-23.9429907960904));
#48372=CARTESIAN_POINT('Ctrl Pts',(6.43560997955544,-6.08057002723013,-53.9665516194108));
#48373=CARTESIAN_POINT('Ctrl Pts',(6.43560997955544,23.9429907960904,-30.0235608233205));
#48374=CARTESIAN_POINT('Ctrl Pts',(6.14415685965718,24.1911416066824,-30.3347320975618));
#48375=CARTESIAN_POINT('Ctrl Pts',(6.14415685965718,54.5258737042442,-6.14359049087936));
#48376=CARTESIAN_POINT('Ctrl Pts',(6.14415685965718,30.3347320975618,24.1911416066824));
#48377=CARTESIAN_POINT('Ctrl Pts',(6.14415685965718,6.14359049087936,54.5258737042442));
#48378=CARTESIAN_POINT('Ctrl Pts',(6.14415685965718,-24.1911416066824,30.3347320975618));
#48379=CARTESIAN_POINT('Ctrl Pts',(6.14415685965718,-54.5258737042442,6.14359049087936));
#48380=CARTESIAN_POINT('Ctrl Pts',(6.14415685965718,-30.3347320975618,-24.1911416066824));
#48381=CARTESIAN_POINT('Ctrl Pts',(6.14415685965718,-6.14359049087936,-54.5258737042442));
#48382=CARTESIAN_POINT('Ctrl Pts',(6.14415685965718,24.1911416066824,-30.3347320975618));
#48383=CARTESIAN_POINT('Ctrl Pts',(6.,24.3161022724906,-30.4914278162532));
#48384=CARTESIAN_POINT('Ctrl Pts',(6.,54.8075300887437,-6.17532554376256));
#48385=CARTESIAN_POINT('Ctrl Pts',(6.,30.4914278162532,24.3161022724906));
#48386=CARTESIAN_POINT('Ctrl Pts',(6.,6.17532554376256,54.8075300887437));
#48387=CARTESIAN_POINT('Ctrl Pts',(6.,-24.3161022724906,30.4914278162532));
#48388=CARTESIAN_POINT('Ctrl Pts',(6.,-54.8075300887437,6.17532554376256));
#48389=CARTESIAN_POINT('Ctrl Pts',(6.,-30.4914278162532,-24.3161022724906));
#48390=CARTESIAN_POINT('Ctrl Pts',(6.,-6.17532554376256,-54.8075300887437));
#48391=CARTESIAN_POINT('Ctrl Pts',(6.,24.3161022724906,-30.4914278162532));
#48392=CARTESIAN_POINT('Ctrl Pts',(15.,23.7252887774277,-19.325389321503));
#48393=CARTESIAN_POINT('Ctrl Pts',(14.0108432136945,25.1521740518353,-18.5591233494113));
#48394=CARTESIAN_POINT('Ctrl Pts',(13.3692319443824,26.0528643724611,-18.0122505544342));
#48395=CARTESIAN_POINT('Ctrl Pts',(12.3476991724842,27.2927306683407,-17.513207272874));
#48396=CARTESIAN_POINT('Ctrl Pts',(12.0250187050191,27.6843780505438,-17.3555701183851));
#48397=CARTESIAN_POINT('Ctrl Pts',(11.6666317570709,28.1212453396965,-17.1859329169356));
#48398=CARTESIAN_POINT('Ctrl Pts',(11.3593868751765,28.4924330909458,-17.0579748855819));
#48399=CARTESIAN_POINT('Ctrl Pts',(10.6767716809131,29.3171120810883,-16.7736866790818));
#48400=CARTESIAN_POINT('Ctrl Pts',(10.1321636914397,29.9604578402936,-16.6234350371559));
#48401=CARTESIAN_POINT('Ctrl Pts',(9.56604173138329,30.6013476901181,-16.6023045952485));
#48402=CARTESIAN_POINT('Ctrl Pts',(9.34563078589195,30.8508683724488,-16.5940777801661));
#48403=CARTESIAN_POINT('Ctrl Pts',(9.1222295109871,31.1000191408333,-16.6060902380637));
#48404=CARTESIAN_POINT('Ctrl Pts',(8.88860711505303,31.3611956288477,-16.6356564204087));
#48405=CARTESIAN_POINT('Ctrl Pts',(8.75830600700764,31.506864821425,-16.6521467329269));
#48406=CARTESIAN_POINT('Ctrl Pts',(8.62340343546576,31.6574103159489,-16.6721496821304));
#48407=CARTESIAN_POINT('Ctrl Pts',(8.40819516300444,31.9000796698313,-16.7185585110703));
#48408=CARTESIAN_POINT('Ctrl Pts',(8.02443006829152,32.3328140926836,-16.8013159647219));
#48409=CARTESIAN_POINT('Ctrl Pts',(7.46417034513354,32.9699846210684,-16.9702026704623));
#48410=CARTESIAN_POINT('Ctrl Pts',(6.85957019142019,33.7100854539055,-17.2206111851372));
#48411=CARTESIAN_POINT('Ctrl Pts',(6.58024553736739,34.0520112834421,-17.3362996633883));
#48412=CARTESIAN_POINT('Ctrl Pts',(6.28976782192772,34.4070814189946,-17.4897602383325));
#48413=CARTESIAN_POINT('Ctrl Pts',(6.,34.7703877941326,-17.6640916167698));
#48414=CARTESIAN_POINT('Ctrl Pts',(2.09999999999998,13.8279757475969,-7.65812678728599));
#48415=CARTESIAN_POINT('Ctrl Pts',(2.73333333333332,13.8279757475969,-7.65812678728599));
#48416=CARTESIAN_POINT('Ctrl Pts',(3.36803303381851,13.8280015254532,-7.6580866539697));
#48417=CARTESIAN_POINT('Ctrl Pts',(4.25276872116174,13.8280168460333,-7.65806146044593));
#48418=CARTESIAN_POINT('Ctrl Pts',(4.77266573001516,13.8321785569649,-7.65073620619348));
#48419=CARTESIAN_POINT('Ctrl Pts',(5.76856597158111,13.844291616205,-7.62951788897893));
#48420=CARTESIAN_POINT('Ctrl Pts',(6.48508033865307,13.8440136699914,-7.630113273714));
#48421=CARTESIAN_POINT('Ctrl Pts',(6.99865791044875,13.827042724761,-7.65945876128045));
#48422=CARTESIAN_POINT('Ctrl Pts',(7.1247971738976,13.8228379227586,-7.66695269622797));
#48423=CARTESIAN_POINT('Ctrl Pts',(7.37169992327966,13.8141335684726,-7.68281784902541));
#48424=CARTESIAN_POINT('Ctrl Pts',(7.68210776228461,13.8021317972921,-7.70522099931852));
#48425=CARTESIAN_POINT('Ctrl Pts',(8.05073533832202,13.7852894828728,-7.73671249396138));
#48426=CARTESIAN_POINT('Ctrl Pts',(8.41503452625175,13.7653021081082,-7.77346916765258));
#48427=CARTESIAN_POINT('Ctrl Pts',(9.01074252234631,13.7255238371934,-7.84464976675126));
#48428=CARTESIAN_POINT('Ctrl Pts',(9.4630926264689,13.6818268405885,-7.91857147136531));
#48429=CARTESIAN_POINT('Ctrl Pts',(10.2678436967056,13.5747717426652,-8.08902421601531));
#48430=CARTESIAN_POINT('Ctrl Pts',(10.9804887503285,13.44484280776,-8.3071906299572));
#48431=CARTESIAN_POINT('Ctrl Pts',(11.7910213121199,13.2470722117918,-8.62018274307134));
#48432=CARTESIAN_POINT('Ctrl Pts',(12.2471503020159,13.1229490575071,-8.80658382774348));
#48433=CARTESIAN_POINT('Ctrl Pts',(12.4732466492024,13.0574621913427,-8.90089570339079));
#48434=CARTESIAN_POINT('Ctrl Pts',(12.8351179681746,12.9496826084397,-9.0521331140034));
#48435=CARTESIAN_POINT('Ctrl Pts',(13.2802512961797,12.802233799643,-9.25581954461894));
#48436=CARTESIAN_POINT('Ctrl Pts',(14.1612564878,12.4620169214753,-9.71481371470994));
#48437=CARTESIAN_POINT('Ctrl Pts',(14.7820737708942,12.1693147416513,-10.0825472947651));
#48438=CARTESIAN_POINT('Ctrl Pts',(15.1979896574214,11.9574529826808,-10.325659137886));
#48439=CARTESIAN_POINT('Ctrl Pts',(2.09999999999998,20.7979970457138,-11.014712137007));
#48440=CARTESIAN_POINT('Ctrl Pts',(2.73333333333332,20.7979970457138,-11.014712137007));
#48441=CARTESIAN_POINT('Ctrl Pts',(3.36871863447842,20.7979957888325,-11.0147100539278));
#48442=CARTESIAN_POINT('Ctrl Pts',(4.25415249655759,20.7980011101394,-11.014697259023));
#48443=CARTESIAN_POINT('Ctrl Pts',(4.78309467008275,20.8040276778098,-11.0036065611137));
#48444=CARTESIAN_POINT('Ctrl Pts',(5.77493400902691,20.821446583213,-10.9717244397128));
#48445=CARTESIAN_POINT('Ctrl Pts',(6.47496358572727,20.820810958958,-10.973026983233));
#48446=CARTESIAN_POINT('Ctrl Pts',(6.96726482620541,20.7970302031018,-11.0159800673788));
#48447=CARTESIAN_POINT('Ctrl Pts',(7.09308276047564,20.7909913536982,-11.0272323285292));
#48448=CARTESIAN_POINT('Ctrl Pts',(7.33628215808622,20.7786039277912,-11.0508651505887));
#48449=CARTESIAN_POINT('Ctrl Pts',(7.64235751563798,20.7615171715808,-11.0842742543889));
#48450=CARTESIAN_POINT('Ctrl Pts',(8.00391288520119,20.7376501778544,-11.1310547409347));
#48451=CARTESIAN_POINT('Ctrl Pts',(8.36000598692249,20.7093493502994,-11.1855823927471));
#48452=CARTESIAN_POINT('Ctrl Pts',(8.93967288853338,20.6532251446613,-11.2907675094849));
#48453=CARTESIAN_POINT('Ctrl Pts',(9.37528826459676,20.5916420820299,-11.3996398370039));
#48454=CARTESIAN_POINT('Ctrl Pts',(10.1433953963723,20.4417998065261,-11.6486751197096));
#48455=CARTESIAN_POINT('Ctrl Pts',(10.8342881133699,20.2594568751716,-11.969903308493));
#48456=CARTESIAN_POINT('Ctrl Pts',(11.6346763171622,19.9775507429201,-12.4374585345057));
#48457=CARTESIAN_POINT('Ctrl Pts',(12.087250380503,19.799601122098,-12.717071440536));
#48458=CARTESIAN_POINT('Ctrl Pts',(12.3122423823028,19.7053497381101,-12.8589426681667));
#48459=CARTESIAN_POINT('Ctrl Pts',(12.6725822269122,19.5499991694726,-13.0866433320915));
#48460=CARTESIAN_POINT('Ctrl Pts',(13.111012820426,19.339646719064,-13.3910169222338));
#48461=CARTESIAN_POINT('Ctrl Pts',(13.9921323132802,18.8489891102053,-14.0840049748908));
#48462=CARTESIAN_POINT('Ctrl Pts',(14.6125773377935,18.4239412983855,-14.6419209794113));
#48463=CARTESIAN_POINT('Ctrl Pts',(15.0291266285127,18.1158843190329,-15.0106560867984));
#48464=CARTESIAN_POINT('Ctrl Pts',(2.09999999999998,27.7680183438307,-14.371297486728));
#48465=CARTESIAN_POINT('Ctrl Pts',(2.73333333333332,27.7680183438307,-14.371297486728));
#48466=CARTESIAN_POINT('Ctrl Pts',(3.36945332065348,27.7680378208204,-14.3712683196438));
#48467=CARTESIAN_POINT('Ctrl Pts',(4.25561608029733,27.7680578943104,-14.3712329142362));
#48468=CARTESIAN_POINT('Ctrl Pts',(4.79358528048294,27.776050427636,-14.3561843266613));
#48469=CARTESIAN_POINT('Ctrl Pts',(5.78145895202477,27.798760568176,-14.3136731881339));
#48470=CARTESIAN_POINT('Ctrl Pts',(6.46486442188066,27.7976233124563,-14.3160366570693));
#48471=CARTESIAN_POINT('Ctrl Pts',(6.93654415129333,27.7679543062191,-14.370711304283));
#48472=CARTESIAN_POINT('Ctrl Pts',(7.06205598783357,27.7600999969903,-14.3856866007946));
#48473=CARTESIAN_POINT('Ctrl Pts',(7.30168699668564,27.7442029155811,-14.4167341707392));
#48474=CARTESIAN_POINT('Ctrl Pts',(7.6036656947927,27.7222916772868,-14.4606373100959));
#48475=CARTESIAN_POINT('Ctrl Pts',(7.95860291280678,27.6918305255677,-14.5218376687646));
#48476=CARTESIAN_POINT('Ctrl Pts',(8.307311571412,27.655870116953,-14.5928583523582));
#48477=CARTESIAN_POINT('Ctrl Pts',(8.87310312231183,27.5847261494896,-14.7294164513786));
#48478=CARTESIAN_POINT('Ctrl Pts',(9.29618304531655,27.5073149978084,-14.8693720517901));
#48479=CARTESIAN_POINT('Ctrl Pts',(10.0462726890403,27.3189544476347,-15.1893221911421));
#48480=CARTESIAN_POINT('Ctrl Pts',(10.740516903946,27.0847770091748,-15.6137212401067));
#48481=CARTESIAN_POINT('Ctrl Pts',(11.5482246043898,26.7159679112832,-16.241552115041));
#48482=CARTESIAN_POINT('Ctrl Pts',(12.0041796923629,26.4828720940238,-16.6169595466783));
#48483=CARTESIAN_POINT('Ctrl Pts',(12.2304128422418,26.3593556717716,-16.8073766296154));
#48484=CARTESIAN_POINT('Ctrl Pts',(12.5924521142123,26.1558011511038,-17.1128169167779));
#48485=CARTESIAN_POINT('Ctrl Pts',(13.0427789525575,25.8764554795404,-17.5278403254683));
#48486=CARTESIAN_POINT('Ctrl Pts',(13.9385896269168,25.2244859115221,-18.4699929405824));
#48487=CARTESIAN_POINT('Ctrl Pts',(14.5670688438605,24.6610742418818,-19.2247640399616));
#48488=CARTESIAN_POINT('Ctrl Pts',(14.9853697475044,24.254629587972,-19.7206424669413));
#48489=CARTESIAN_POINT('Ctrl Pts',(2.09999999999998,34.7380396419475,-17.727882836449));
#48490=CARTESIAN_POINT('Ctrl Pts',(2.73333333333332,34.7380396419475,-17.727882836449));
#48491=CARTESIAN_POINT('Ctrl Pts',(3.37020393653566,34.7380735049305,-17.7278392579628));
#48492=CARTESIAN_POINT('Ctrl Pts',(4.25711961877983,34.7381056827597,-17.7277866677452));
#48493=CARTESIAN_POINT('Ctrl Pts',(4.80402220532588,34.7481429814137,-17.7086154435085));
#48494=CARTESIAN_POINT('Ctrl Pts',(5.78813454502387,34.7761040328012,-17.6555601576571));
#48495=CARTESIAN_POINT('Ctrl Pts',(6.45445182277513,34.7742910555487,-17.6593420657212));
#48496=CARTESIAN_POINT('Ctrl Pts',(6.90690766682582,34.7394581505422,-17.7242403373792));
#48497=CARTESIAN_POINT('Ctrl Pts',(7.03214349859616,34.7298009507745,-17.7429143633733));
#48498=CARTESIAN_POINT('Ctrl Pts',(7.26849387006162,34.7105274847739,-17.781104666533));
#48499=CARTESIAN_POINT('Ctrl Pts',(7.56683268339157,34.683957518025,-17.8351670693613));
#48500=CARTESIAN_POINT('Ctrl Pts',(7.91604911717842,34.6471776150214,-17.9102341213459));
#48501=CARTESIAN_POINT('Ctrl Pts',(8.25884519308195,34.6038583650633,-17.99715521056));
#48502=CARTESIAN_POINT('Ctrl Pts',(8.814270992878,34.5181491335739,-18.1642080280054));
#48503=CARTESIAN_POINT('Ctrl Pts',(9.23053609210392,34.4249120745718,-18.3353270659959));
#48504=CARTESIAN_POINT('Ctrl Pts',(9.97649944922677,34.1947051258132,-18.7327306189381));
#48505=CARTESIAN_POINT('Ctrl Pts',(10.6790209735713,33.9025959931162,-19.2714823555945));
#48506=CARTESIAN_POINT('Ctrl Pts',(11.4920879596953,33.4429950265762,-20.065251397391));
#48507=CARTESIAN_POINT('Ctrl Pts',(11.9504408299826,33.1531140023176,-20.5385307869332));
#48508=CARTESIAN_POINT('Ctrl Pts',(12.1774708173222,32.9997497984637,-20.7780730187058));
#48509=CARTESIAN_POINT('Ctrl Pts',(12.5406713626334,32.7471412732904,-21.1620343438423));
#48510=CARTESIAN_POINT('Ctrl Pts',(12.997673300029,32.3954626109581,-21.6919929876177));
#48511=CARTESIAN_POINT('Ctrl Pts',(13.8993993294321,31.5803589389699,-22.8835829401895));
#48512=CARTESIAN_POINT('Ctrl Pts',(14.5324532885843,30.8775669453658,-23.8349298069317));
#48513=CARTESIAN_POINT('Ctrl Pts',(14.9514110803021,30.3723459825604,-24.457322833162));
#48514=CARTESIAN_POINT('',(3.2,33.4762280926097,-17.1202264205696));
#48515=CARTESIAN_POINT('Ctrl Pts',(3.2,33.4762280926097,-17.1202264205697));
#48516=CARTESIAN_POINT('Ctrl Pts',(3.5615227483539,32.470273991762,-16.6357844579161));
#48517=CARTESIAN_POINT('Ctrl Pts',(3.95224584525312,31.4490477361342,-16.1504264387208));
#48518=CARTESIAN_POINT('Ctrl Pts',(4.78767430123564,29.4297069892437,-15.1533367200056));
#48519=CARTESIAN_POINT('Ctrl Pts',(5.21513946231862,28.4699606481904,-14.6620752040124));
#48520=CARTESIAN_POINT('Ctrl Pts',(6.79548775402185,25.1212555511771,-13.012167423548));
#48521=CARTESIAN_POINT('Ctrl Pts',(7.9401629593867,23.0391778774888,-12.2240189743849));
#48522=CARTESIAN_POINT('Ctrl Pts',(9.46271935274971,20.413489232316,-11.3125228814697));
#48523=CARTESIAN_POINT('Ctrl Pts',(10.1385443659007,19.3034154994021,-11.0292622078652));
#48524=CARTESIAN_POINT('Ctrl Pts',(11.5967860400667,16.9862280609382,-10.6585988316486));
#48525=CARTESIAN_POINT('Ctrl Pts',(12.399735667707,15.7679338637663,-10.4920203380681));
#48526=CARTESIAN_POINT('Ctrl Pts',(13.6850585208124,13.8903785225595,-10.3029151929985));
#48527=CARTESIAN_POINT('Ctrl Pts',(14.3457395898618,12.9431348360658,-10.2602733177061));
#48528=CARTESIAN_POINT('Ctrl Pts',(15.,12.0570237116074,-10.2098078054769));
#48529=CARTESIAN_POINT('Ctrl Pts',(2.79814995341175,34.3237720576307,-17.5283618512166));
#48530=CARTESIAN_POINT('Ctrl Pts',(2.93286002554174,34.0413567394956,-17.3923509689602));
#48531=CARTESIAN_POINT('Ctrl Pts',(3.06772762579813,33.7587618460436,-17.2562524503664));
#48532=CARTESIAN_POINT('Ctrl Pts',(3.20257974079352,33.47625152623,-17.1201943222877));
#48533=CARTESIAN_POINT('Origin',(2.9,0.,0.));
#48534=CARTESIAN_POINT('',(3.2,24.1401481407882,-28.8273003894017));
#48535=CARTESIAN_POINT('Origin',(3.2,0.,0.));
#48536=CARTESIAN_POINT('Ctrl Pts',(3.19853209668272,24.1400733004768,-28.8273374408964));
#48537=CARTESIAN_POINT('Ctrl Pts',(3.06441460888704,24.3356896029093,-29.0726077758756));
#48538=CARTESIAN_POINT('Ctrl Pts',(2.93029925412543,24.5312702067218,-29.3178337273723));
#48539=CARTESIAN_POINT('Ctrl Pts',(2.79629300805566,24.7266240747468,-29.5627789633676));
#48540=CARTESIAN_POINT('Ctrl Pts',(2.09999999999999,4.38966495848408,-15.1878155149937));
#48541=CARTESIAN_POINT('Ctrl Pts',(2.73333333333332,4.38966495848408,-15.1878155149937));
#48542=CARTESIAN_POINT('Ctrl Pts',(3.36596254895254,4.38957946978066,-15.1878260991564));
#48543=CARTESIAN_POINT('Ctrl Pts',(4.12347126801082,4.38955322135183,-15.1878292451984));
#48544=CARTESIAN_POINT('Ctrl Pts',(4.36306410485066,4.39143213229248,-15.1873073007927));
#48545=CARTESIAN_POINT('Ctrl Pts',(4.85754827137282,4.40010260543508,-15.1849115824678));
#48546=CARTESIAN_POINT('Ctrl Pts',(5.73896685227764,4.42073647768525,-15.1792300101236));
#48547=CARTESIAN_POINT('Ctrl Pts',(6.52602599492339,4.42132553322825,-15.1790826820951));
#48548=CARTESIAN_POINT('Ctrl Pts',(7.12753345010613,4.38299182110871,-15.1894872387425));
#48549=CARTESIAN_POINT('Ctrl Pts',(7.25502865634115,4.37462153877536,-15.191853620938));
#48550=CARTESIAN_POINT('Ctrl Pts',(7.51728707570608,4.35616970860387,-15.1972532622203));
#48551=CARTESIAN_POINT('Ctrl Pts',(7.84585340416012,4.33027233957835,-15.2050840117294));
#48552=CARTESIAN_POINT('Ctrl Pts',(8.2441318948403,4.29329339033759,-15.2162818026573));
#48553=CARTESIAN_POINT('Ctrl Pts',(8.77643068220616,4.23440926929706,-15.2336446863811));
#48554=CARTESIAN_POINT('Ctrl Pts',(9.44110000562817,4.1397604107769,-15.2599899543444));
#48555=CARTESIAN_POINT('Ctrl Pts',(9.96384938741169,4.03395832280009,-15.2862881501386));
#48556=CARTESIAN_POINT('Ctrl Pts',(11.1188752712428,3.75254025914602,-15.3517209561057));
#48557=CARTESIAN_POINT('Ctrl Pts',(12.0804115271536,3.36144010237934,-15.4503087637338));
#48558=CARTESIAN_POINT('Ctrl Pts',(13.00080324578,2.91750211822961,-15.534724281135));
#48559=CARTESIAN_POINT('Ctrl Pts',(13.2107807208523,2.81340029136765,-15.5529519774906));
#48560=CARTESIAN_POINT('Ctrl Pts',(13.3144041536197,2.76145108518079,-15.5616032545832));
#48561=CARTESIAN_POINT('Ctrl Pts',(13.373284229634,2.73178424239228,-15.5664128874317));
#48562=CARTESIAN_POINT('Ctrl Pts',(13.4025633600174,2.7169858062115,-15.5687674529565));
#48563=CARTESIAN_POINT('Ctrl Pts',(13.6877617951153,2.57262378140117,-15.5914878140199));
#48564=CARTESIAN_POINT('Ctrl Pts',(14.2465713444148,2.26056171575794,-15.6382203410322));
#48565=CARTESIAN_POINT('Ctrl Pts',(14.7537307590314,1.9309622388219,-15.6810511943411));
#48566=CARTESIAN_POINT('Ctrl Pts',(14.9999999999997,1.76250180637518,-15.7004962848038));
#48567=CARTESIAN_POINT('Ctrl Pts',(2.09999999999999,6.11093362092453,-22.7291862684821));
#48568=CARTESIAN_POINT('Ctrl Pts',(2.73333333333332,6.11093362092453,-22.7291862684821));
#48569=CARTESIAN_POINT('Ctrl Pts',(3.3655737913602,6.11087106652427,-22.7291970270664));
#48570=CARTESIAN_POINT('Ctrl Pts',(4.12266523196545,6.11085340617054,-22.7291999896352));
#48571=CARTESIAN_POINT('Ctrl Pts',(4.3569775538667,6.11363264974669,-22.7284859949201));
#48572=CARTESIAN_POINT('Ctrl Pts',(4.84797905966998,6.12654915024314,-22.7251818552908));
#48573=CARTESIAN_POINT('Ctrl Pts',(5.73066233595544,6.15746420822384,-22.7172920110342));
#48574=CARTESIAN_POINT('Ctrl Pts',(6.53591128078968,6.15880152770652,-22.7169853053249));
#48575=CARTESIAN_POINT('Ctrl Pts',(7.15865947305896,6.10013179404174,-22.7317937279026));
#48576=CARTESIAN_POINT('Ctrl Pts',(7.28648425494255,6.08758374572187,-22.7350894297213));
#48577=CARTESIAN_POINT('Ctrl Pts',(7.55244779773386,6.05971829150288,-22.7426848792085));
#48578=CARTESIAN_POINT('Ctrl Pts',(7.88537213844326,6.02064645072765,-22.7537144590768));
#48579=CARTESIAN_POINT('Ctrl Pts',(8.29072621569934,5.96466756362568,-22.7695297564594));
#48580=CARTESIAN_POINT('Ctrl Pts',(8.83399521564723,5.87541197003736,-22.794060849192));
#48581=CARTESIAN_POINT('Ctrl Pts',(9.51593856281283,5.73146685019894,-22.831284068277));
#48582=CARTESIAN_POINT('Ctrl Pts',(10.0562578372541,5.56988387032315,-22.8683818954022));
#48583=CARTESIAN_POINT('Ctrl Pts',(11.2544819138336,5.13867129632783,-22.9606714121106));
#48584=CARTESIAN_POINT('Ctrl Pts',(12.2341371971438,4.54497963493266,-23.0984661085317));
#48585=CARTESIAN_POINT('Ctrl Pts',(13.1607383237085,3.8783134664302,-23.2117153171294));
#48586=CARTESIAN_POINT('Ctrl Pts',(13.3718398189947,3.72213984640676,-23.2359021626504));
#48587=CARTESIAN_POINT('Ctrl Pts',(13.4758883775225,3.64427692494074,-23.2472871755526));
#48588=CARTESIAN_POINT('Ctrl Pts',(13.5349923709208,3.59982374741586,-23.2535912907113));
#48589=CARTESIAN_POINT('Ctrl Pts',(13.5643621042971,3.57765592245332,-23.2566667766753));
#48590=CARTESIAN_POINT('Ctrl Pts',(13.8508605081462,3.36143178692841,-23.2863343991313));
#48591=CARTESIAN_POINT('Ctrl Pts',(14.4158889403965,2.89109929538129,-23.3477528779048));
#48592=CARTESIAN_POINT('Ctrl Pts',(14.9236315787721,2.39870457596863,-23.4020283054991));
#48593=CARTESIAN_POINT('Ctrl Pts',(15.169681381964,2.14715825974705,-23.4260803465695));
#48594=CARTESIAN_POINT('Ctrl Pts',(2.09999999999999,7.83220228336497,-30.2705570219704));
#48595=CARTESIAN_POINT('Ctrl Pts',(2.73333333333333,7.83220228336497,-30.2705570219704));
#48596=CARTESIAN_POINT('Ctrl Pts',(3.36510345911249,7.83209226044356,-30.270570640248));
#48597=CARTESIAN_POINT('Ctrl Pts',(4.1217534628143,7.83206130605595,-30.2705741234367));
#48598=CARTESIAN_POINT('Ctrl Pts',(4.35077319609568,7.83567895787034,-30.269681067371));
#48599=CARTESIAN_POINT('Ctrl Pts',(4.83830702967109,7.85271633513914,-30.2654944557726));
#48600=CARTESIAN_POINT('Ctrl Pts',(5.72214362909506,7.89392143672765,-30.2553902143163));
#48601=CARTESIAN_POINT('Ctrl Pts',(6.54567911469843,7.8964013330852,-30.2548130793221));
#48602=CARTESIAN_POINT('Ctrl Pts',(7.18899146074693,7.81535022009343,-30.2744804534963));
#48603=CARTESIAN_POINT('Ctrl Pts',(7.31712941776005,7.79858600371208,-30.2787128644861));
#48604=CARTESIAN_POINT('Ctrl Pts',(7.58666087185036,7.76092169042061,-30.2885887307684));
#48605=CARTESIAN_POINT('Ctrl Pts',(7.92369029396209,7.70812152044347,-30.3029317759761));
#48606=CARTESIAN_POINT('Ctrl Pts',(8.33566195251538,7.6321812153183,-30.3235714663787));
#48607=CARTESIAN_POINT('Ctrl Pts',(8.88877416188324,7.51072584522975,-30.3556463460423));
#48608=CARTESIAN_POINT('Ctrl Pts',(9.58532271430234,7.31403511981607,-30.4044467728404));
#48609=CARTESIAN_POINT('Ctrl Pts',(10.1375097070441,7.0922890814097,-30.4531604646358));
#48610=CARTESIAN_POINT('Ctrl Pts',(11.3564859597505,6.50114151522531,-30.5739966068883));
#48611=CARTESIAN_POINT('Ctrl Pts',(12.3227698011673,5.70961632447872,-30.749314104971));
#48612=CARTESIAN_POINT('Ctrl Pts',(13.2437945503543,4.82611747317232,-30.8902721426667));
#48613=CARTESIAN_POINT('Ctrl Pts',(13.4536418756815,4.61888452203683,-30.9202132651585));
#48614=CARTESIAN_POINT('Ctrl Pts',(13.5572058324948,4.51557794210463,-30.9342418296942));
#48615=CARTESIAN_POINT('Ctrl Pts',(13.616045355569,4.45658101854197,-30.9419927542262));
#48616=CARTESIAN_POINT('Ctrl Pts',(13.6453023755694,4.42715785743315,-30.9457673242247));
#48617=CARTESIAN_POINT('Ctrl Pts',(13.9303991372842,4.14015109313492,-30.9821481247373));
#48618=CARTESIAN_POINT('Ctrl Pts',(14.4834575035054,3.52369906436613,-31.0568154715655));
#48619=CARTESIAN_POINT('Ctrl Pts',(14.98335392639,2.87761683656506,-31.1220628682749));
#48620=CARTESIAN_POINT('Ctrl Pts',(15.2260186760796,2.54742814619257,-31.1506506793037));
#48621=CARTESIAN_POINT('Ctrl Pts',(2.09999999999999,9.55347094580542,-37.8119277754588));
#48622=CARTESIAN_POINT('Ctrl Pts',(2.73333333333332,9.55347094580542,-37.8119277754588));
#48623=CARTESIAN_POINT('Ctrl Pts',(3.3646253867,9.55334556061245,-37.8119373823181));
#48624=CARTESIAN_POINT('Ctrl Pts',(4.12083619687885,9.55331129117588,-37.8119392787534));
#48625=CARTESIAN_POINT('Ctrl Pts',(4.34455066434138,9.55771726793094,-37.8108785541332));
#48626=CARTESIAN_POINT('Ctrl Pts',(4.82869096816822,9.57876287103758,-37.8058356126046));
#48627=CARTESIAN_POINT('Ctrl Pts',(5.7134771442972,9.63033870088108,-37.7934981042942));
#48628=CARTESIAN_POINT('Ctrl Pts',(6.55580364168112,9.63438372222901,-37.7925563845865));
#48629=CARTESIAN_POINT('Ctrl Pts',(7.21828976823775,9.52934075289251,-37.817447696476));
#48630=CARTESIAN_POINT('Ctrl Pts',(7.3467116336193,9.50833437573421,-37.8226219766341));
#48631=CARTESIAN_POINT('Ctrl Pts',(7.61952278444273,9.46057626186425,-37.8348434394394));
#48632=CARTESIAN_POINT('Ctrl Pts',(7.960209967387,9.39369388800056,-37.8525768539309));
#48633=CARTESIAN_POINT('Ctrl Pts',(8.3778920674049,9.29718580374087,-37.8781705824178));
#48634=CARTESIAN_POINT('Ctrl Pts',(8.93892669180996,9.14269283098213,-37.9179631531491));
#48635=CARTESIAN_POINT('Ctrl Pts',(9.64584227564656,8.89230767815167,-37.9785191856093));
#48636=CARTESIAN_POINT('Ctrl Pts',(10.2035290263583,8.61151321278556,-38.0385832751922));
#48637=CARTESIAN_POINT('Ctrl Pts',(11.4269246328553,7.86934876020126,-38.1861224416156));
#48638=CARTESIAN_POINT('Ctrl Pts',(12.3794141170359,6.89524642147764,-38.3965674938924));
#48639=CARTESIAN_POINT('Ctrl Pts',(13.2972381141874,5.79878047753586,-38.5654665629587));
#48640=CARTESIAN_POINT('Ctrl Pts',(13.5062083794909,5.54140336948116,-38.6011993448011));
#48641=CARTESIAN_POINT('Ctrl Pts',(13.6094812333749,5.41297301418053,-38.61791765796));
#48642=CARTESIAN_POINT('Ctrl Pts',(13.6681544593943,5.33961012006986,-38.627141819842));
#48643=CARTESIAN_POINT('Ctrl Pts',(13.6973468401446,5.30300492151899,-38.6316312237005));
#48644=CARTESIAN_POINT('Ctrl Pts',(13.9814496921678,4.94616478641267,-38.6748449459509));
#48645=CARTESIAN_POINT('Ctrl Pts',(14.5280778199499,4.18885241132974,-38.7627420404612));
#48646=CARTESIAN_POINT('Ctrl Pts',(15.0243070371674,3.39004417986617,-38.8395722021707));
#48647=CARTESIAN_POINT('Ctrl Pts',(15.2656150130537,2.98140716137769,-38.873032388801));
#48648=CARTESIAN_POINT('',(3.2,9.24182505978396,-36.4465179346992));
#48649=CARTESIAN_POINT('Ctrl Pts',(3.19846192322169,9.24174412230254,-36.446524619893));
#48650=CARTESIAN_POINT('Ctrl Pts',(3.06435645359065,9.3115682491172,-36.7523808556989));
#48651=CARTESIAN_POINT('Ctrl Pts',(2.93025382215074,9.38137979123532,-37.0581800253732));
#48652=CARTESIAN_POINT('Ctrl Pts',(2.79625939386437,9.4511090207012,-37.3636263694961));
#48653=CARTESIAN_POINT('',(15.,1.76250180637585,-15.7004962848173));
#48654=CARTESIAN_POINT('Ctrl Pts',(15.,1.76250180637585,-15.7004962848173));
#48655=CARTESIAN_POINT('Ctrl Pts',(14.489716577951,2.14749161156547,-16.2136060493571));
#48656=CARTESIAN_POINT('Ctrl Pts',(13.9833803026603,2.52923395303641,-16.7499747962178));
#48657=CARTESIAN_POINT('Ctrl Pts',(13.4460287676664,2.91284724496658,-17.3603709065187));
#48658=CARTESIAN_POINT('Ctrl Pts',(12.8282655680968,3.3538661296022,-18.0621093952879));
#48659=CARTESIAN_POINT('Ctrl Pts',(12.1555414089315,3.86577076245241,-18.8782945384456));
#48660=CARTESIAN_POINT('Ctrl Pts',(11.590490807333,4.2779947817326,-19.615690057469));
#48661=CARTESIAN_POINT('Ctrl Pts',(11.1143368259492,4.62536563214324,-20.2370747816766));
#48662=CARTESIAN_POINT('Ctrl Pts',(10.695315894954,4.91856680462629,-20.8194972243441));
#48663=CARTESIAN_POINT('Ctrl Pts',(10.2957959918397,5.1785107966465,-21.4059609250791));
#48664=CARTESIAN_POINT('Ctrl Pts',(10.0450888109769,5.34163114412759,-21.7739792889792));
#48665=CARTESIAN_POINT('Ctrl Pts',(9.80235305588442,5.49247002263581,-22.1433667549693));
#48666=CARTESIAN_POINT('Ctrl Pts',(9.56010106243628,5.63900849396958,-22.5247929586984));
#48667=CARTESIAN_POINT('Ctrl Pts',(9.36613602954693,5.75633813492419,-22.8301912553154));
#48668=CARTESIAN_POINT('Ctrl Pts',(9.15248571318201,5.88298942934388,-23.173697229624));
#48669=CARTESIAN_POINT('Ctrl Pts',(8.89022359857544,6.03502754169084,-23.6134759700354));
#48670=CARTESIAN_POINT('Ctrl Pts',(8.39222406134029,6.32372692057166,-24.4485550646247));
#48671=CARTESIAN_POINT('Ctrl Pts',(7.76643777388907,6.67223453859443,-25.5605956387439));
#48672=CARTESIAN_POINT('Ctrl Pts',(7.10363554123529,7.0511614476926,-26.8754977862185));
#48673=CARTESIAN_POINT('Ctrl Pts',(6.2355001824917,7.5474781949211,-28.59775065634));
#48674=CARTESIAN_POINT('Ctrl Pts',(5.31040885823697,7.96875536932003,-30.6993155625113));
#48675=CARTESIAN_POINT('Ctrl Pts',(4.4641661690584,8.44366203772272,-32.909077030235));
#48676=CARTESIAN_POINT('Ctrl Pts',(4.30741751125468,8.53162850857804,-33.318388860708));
#48677=CARTESIAN_POINT('Ctrl Pts',(4.15262292089523,8.62235919623212,-33.732460653513));
#48678=CARTESIAN_POINT('Ctrl Pts',(4.,8.71775829923914,-34.1504314334527));
#48679=CARTESIAN_POINT('Ctrl Pts',(3.72434973283382,8.89005737513843,-34.9053230085993));
#48680=CARTESIAN_POINT('Ctrl Pts',(3.45587123478818,9.06598205759024,-35.6760994039458));
#48681=CARTESIAN_POINT('Ctrl Pts',(3.2,9.24182505978395,-36.4465179346992));
#48682=CARTESIAN_POINT('',(15.,2.79596292475043,-30.471996838465));
#48683=CARTESIAN_POINT('Ctrl Pts',(15.,2.79596292475043,-30.471996838465));
#48684=CARTESIAN_POINT('Ctrl Pts',(15.,2.47177016953902,-26.0694692115998));
#48685=CARTESIAN_POINT('Ctrl Pts',(15.,2.09636968496858,-20.8427222796618));
#48686=CARTESIAN_POINT('Ctrl Pts',(15.,1.76250180637585,-15.7004962848173));
#48687=CARTESIAN_POINT('Ctrl Pts',(6.,9.62277221548328,-37.7942092772018));
#48688=CARTESIAN_POINT('Ctrl Pts',(6.38595465246567,9.50256245865601,-37.2711033988583));
#48689=CARTESIAN_POINT('Ctrl Pts',(6.7702364866826,9.36752460422606,-36.7864270136994));
#48690=CARTESIAN_POINT('Ctrl Pts',(7.13915213286207,9.20934876194912,-36.3528657054113));
#48691=CARTESIAN_POINT('Ctrl Pts',(8.10667920093232,8.79451298444103,-35.2157973653154));
#48692=CARTESIAN_POINT('Ctrl Pts',(8.9801988874736,8.36872065597838,-34.3895418272531));
#48693=CARTESIAN_POINT('Ctrl Pts',(9.46656009721066,8.09341256870629,-33.9615794459728));
#48694=CARTESIAN_POINT('Ctrl Pts',(9.65648624874906,7.98590357239622,-33.7944582889962));
#48695=CARTESIAN_POINT('Ctrl Pts',(9.79228848853725,7.90448352099192,-33.6801480890427));
#48696=CARTESIAN_POINT('Ctrl Pts',(9.94593825727815,7.80836128617838,-33.5541469568644));
#48697=CARTESIAN_POINT('Ctrl Pts',(10.1065740866009,7.70786862008357,-33.4224168766375));
#48698=CARTESIAN_POINT('Ctrl Pts',(10.2660951669675,7.60273427161563,-33.2963654618293));
#48699=CARTESIAN_POINT('Ctrl Pts',(10.4261869573617,7.4903924666703,-33.1745211766193));
#48700=CARTESIAN_POINT('Ctrl Pts',(10.8065549509411,7.2234754259092,-32.8850268422731));
#48701=CARTESIAN_POINT('Ctrl Pts',(11.1894211925257,6.91488309382193,-32.619770871127));
#48702=CARTESIAN_POINT('Ctrl Pts',(11.6023503255242,6.54089716906719,-32.3560535901122));
#48703=CARTESIAN_POINT('Ctrl Pts',(11.7531893954247,6.40428368133321,-32.2597201851618));
#48704=CARTESIAN_POINT('Ctrl Pts',(11.9080270687775,6.25882196066766,-32.1636787693489));
#48705=CARTESIAN_POINT('Ctrl Pts',(12.0681766131679,6.1031541062351,-32.0669994274948));
#48706=CARTESIAN_POINT('Ctrl Pts',(12.1838435903474,5.99072400076856,-31.9971733953913));
#48707=CARTESIAN_POINT('Ctrl Pts',(12.310086541016,5.86655265076557,-31.9217320004455));
#48708=CARTESIAN_POINT('Ctrl Pts',(12.5127093730711,5.65894503108766,-31.8047262190236));
#48709=CARTESIAN_POINT('Ctrl Pts',(12.7975492664041,5.36709770250972,-31.6402436976734));
#48710=CARTESIAN_POINT('Ctrl Pts',(13.1874566943566,4.95016249777334,-31.4228609771219));
#48711=CARTESIAN_POINT('Ctrl Pts',(13.6431584568239,4.45104726343863,-31.1770289723232));
#48712=CARTESIAN_POINT('Ctrl Pts',(14.069523646534,3.98406341763974,-30.9470228191864));
#48713=CARTESIAN_POINT('Ctrl Pts',(14.53311408767,3.41883288085212,-30.7098459010755));
#48714=CARTESIAN_POINT('Ctrl Pts',(15.,2.79596292475043,-30.471996838465));
#48715=CARTESIAN_POINT('Origin',(15.,-1.89142793862867,-8.2868872535455));
#48716=CARTESIAN_POINT('',(15.,-0.464917847313567,-15.7922717682507));
#48717=CARTESIAN_POINT('Ctrl Pts',(15.,-0.464917847313565,-15.7922717682507));
#48718=CARTESIAN_POINT('Ctrl Pts',(15.,0.278045388530768,-15.8141442938323));
#48719=CARTESIAN_POINT('Ctrl Pts',(15.,1.02237787096417,-15.7835809051657));
#48720=CARTESIAN_POINT('Ctrl Pts',(15.,1.76250180637586,-15.7004962848173));
#48721=CARTESIAN_POINT('',(15.,-0.316722183622946,-30.5983608557452));
#48722=CARTESIAN_POINT('Ctrl Pts',(15.,-0.464917847313579,-15.7922717682507));
#48723=CARTESIAN_POINT('Ctrl Pts',(15.,-0.381235181719544,-21.0899243277258));
#48724=CARTESIAN_POINT('Ctrl Pts',(15.,-0.341535500947833,-26.4322224392563));
#48725=CARTESIAN_POINT('Ctrl Pts',(15.,-0.316722183622933,-30.5983608557452));
#48726=CARTESIAN_POINT('Origin',(15.,0.,0.));
#48727=CARTESIAN_POINT('Ctrl Pts',(15.,-6.80914057906323,-29.8327941127638));
#48728=CARTESIAN_POINT('Ctrl Pts',(15.,23.0236535337006,-36.641934691827));
#48729=CARTESIAN_POINT('Ctrl Pts',(15.,29.8327941127638,-6.80914057906323));
#48730=CARTESIAN_POINT('Ctrl Pts',(15.,36.641934691827,23.0236535337006));
#48731=CARTESIAN_POINT('Ctrl Pts',(15.,6.80914057906323,29.8327941127638));
#48732=CARTESIAN_POINT('Ctrl Pts',(15.,-23.0236535337006,36.641934691827));
#48733=CARTESIAN_POINT('Ctrl Pts',(15.,-29.8327941127638,6.80914057906323));
#48734=CARTESIAN_POINT('Ctrl Pts',(15.,-36.641934691827,-23.0236535337006));
#48735=CARTESIAN_POINT('Ctrl Pts',(15.,-6.80914057906323,-29.8327941127638));
#48736=CARTESIAN_POINT('Ctrl Pts',(14.7843073131059,-6.83933995053714,-29.9651062042906));
#48737=CARTESIAN_POINT('Ctrl Pts',(14.7843073131059,23.1257662537535,-36.8044461548278));
#48738=CARTESIAN_POINT('Ctrl Pts',(14.7843073131059,29.9651062042906,-6.83933995053714));
#48739=CARTESIAN_POINT('Ctrl Pts',(14.7843073131059,36.8044461548278,23.1257662537535));
#48740=CARTESIAN_POINT('Ctrl Pts',(14.7843073131059,6.83933995053714,29.9651062042906));
#48741=CARTESIAN_POINT('Ctrl Pts',(14.7843073131059,-23.1257662537535,36.8044461548278));
#48742=CARTESIAN_POINT('Ctrl Pts',(14.7843073131059,-29.9651062042906,6.83933995053714));
#48743=CARTESIAN_POINT('Ctrl Pts',(14.7843073131059,-36.8044461548278,-23.1257662537535));
#48744=CARTESIAN_POINT('Ctrl Pts',(14.7843073131059,-6.83933995053714,-29.9651062042906));
#48745=CARTESIAN_POINT('Ctrl Pts',(14.3560298066371,-6.90036423817606,-30.2324710777091));
#48746=CARTESIAN_POINT('Ctrl Pts',(14.3560298066371,23.3321068395331,-37.1328353158852));
#48747=CARTESIAN_POINT('Ctrl Pts',(14.3560298066371,30.2324710777091,-6.90036423817606));
#48748=CARTESIAN_POINT('Ctrl Pts',(14.3560298066371,37.1328353158852,23.3321068395331));
#48749=CARTESIAN_POINT('Ctrl Pts',(14.3560298066371,6.90036423817606,30.2324710777091));
#48750=CARTESIAN_POINT('Ctrl Pts',(14.3560298066371,-23.3321068395331,37.1328353158852));
#48751=CARTESIAN_POINT('Ctrl Pts',(14.3560298066371,-30.2324710777091,6.90036423817606));
#48752=CARTESIAN_POINT('Ctrl Pts',(14.3560298066371,-37.1328353158852,-23.3321068395331));
#48753=CARTESIAN_POINT('Ctrl Pts',(14.3560298066371,-6.90036423817606,-30.2324710777091));
#48754=CARTESIAN_POINT('Ctrl Pts',(13.722936818686,-6.99377723724461,-30.6417401677374));
#48755=CARTESIAN_POINT('Ctrl Pts',(13.722936818686,23.6479629304928,-37.635517404982));
#48756=CARTESIAN_POINT('Ctrl Pts',(13.722936818686,30.6417401677374,-6.99377723724461));
#48757=CARTESIAN_POINT('Ctrl Pts',(13.722936818686,37.635517404982,23.6479629304928));
#48758=CARTESIAN_POINT('Ctrl Pts',(13.722936818686,6.99377723724461,30.6417401677374));
#48759=CARTESIAN_POINT('Ctrl Pts',(13.722936818686,-23.6479629304928,37.635517404982));
#48760=CARTESIAN_POINT('Ctrl Pts',(13.722936818686,-30.6417401677374,6.99377723724461));
#48761=CARTESIAN_POINT('Ctrl Pts',(13.722936818686,-37.635517404982,-23.6479629304928));
#48762=CARTESIAN_POINT('Ctrl Pts',(13.722936818686,-6.99377723724461,-30.6417401677374));
#48763=CARTESIAN_POINT('Ctrl Pts',(12.8977690042853,-7.12214335873524,-31.204148893041));
#48764=CARTESIAN_POINT('Ctrl Pts',(12.8977690042853,24.0820055343058,-38.3262922517763));
#48765=CARTESIAN_POINT('Ctrl Pts',(12.8977690042853,31.204148893041,-7.12214335873524));
#48766=CARTESIAN_POINT('Ctrl Pts',(12.8977690042853,38.3262922517763,24.0820055343058));
#48767=CARTESIAN_POINT('Ctrl Pts',(12.8977690042853,7.12214335873524,31.204148893041));
#48768=CARTESIAN_POINT('Ctrl Pts',(12.8977690042853,-24.0820055343058,38.3262922517763));
#48769=CARTESIAN_POINT('Ctrl Pts',(12.8977690042853,-31.204148893041,7.12214335873524));
#48770=CARTESIAN_POINT('Ctrl Pts',(12.8977690042853,-38.3262922517763,-24.0820055343058));
#48771=CARTESIAN_POINT('Ctrl Pts',(12.8977690042853,-7.12214335873524,-31.204148893041));
#48772=CARTESIAN_POINT('Ctrl Pts',(11.9000549946031,-7.28939328253151,-31.9369186874159));
#48773=CARTESIAN_POINT('Ctrl Pts',(11.9000549946031,24.6475254048843,-39.2263119699474));
#48774=CARTESIAN_POINT('Ctrl Pts',(11.9000549946031,31.9369186874159,-7.28939328253151));
#48775=CARTESIAN_POINT('Ctrl Pts',(11.9000549946031,39.2263119699474,24.6475254048843));
#48776=CARTESIAN_POINT('Ctrl Pts',(11.9000549946031,7.28939328253151,31.9369186874159));
#48777=CARTESIAN_POINT('Ctrl Pts',(11.9000549946031,-24.6475254048843,39.2263119699474));
#48778=CARTESIAN_POINT('Ctrl Pts',(11.9000549946031,-31.9369186874159,7.28939328253151));
#48779=CARTESIAN_POINT('Ctrl Pts',(11.9000549946031,-39.2263119699474,-24.6475254048843));
#48780=CARTESIAN_POINT('Ctrl Pts',(11.9000549946031,-7.28939328253151,-31.9369186874159));
#48781=CARTESIAN_POINT('Ctrl Pts',(10.9391333834985,-7.4640486993045,-32.702134066474));
#48782=CARTESIAN_POINT('Ctrl Pts',(10.9391333834985,25.2380853671694,-40.1661827657784));
#48783=CARTESIAN_POINT('Ctrl Pts',(10.9391333834985,32.702134066474,-7.4640486993045));
#48784=CARTESIAN_POINT('Ctrl Pts',(10.9391333834985,40.1661827657784,25.2380853671694));
#48785=CARTESIAN_POINT('Ctrl Pts',(10.9391333834985,7.4640486993045,32.702134066474));
#48786=CARTESIAN_POINT('Ctrl Pts',(10.9391333834985,-25.2380853671694,40.1661827657784));
#48787=CARTESIAN_POINT('Ctrl Pts',(10.9391333834985,-32.702134066474,7.4640486993045));
#48788=CARTESIAN_POINT('Ctrl Pts',(10.9391333834985,-40.1661827657784,-25.2380853671694));
#48789=CARTESIAN_POINT('Ctrl Pts',(10.9391333834985,-7.4640486993045,-32.702134066474));
#48790=CARTESIAN_POINT('Ctrl Pts',(10.0180552497783,-7.64672372347923,-33.5024856413123));
#48791=CARTESIAN_POINT('Ctrl Pts',(10.0180552497783,25.855761917833,-41.1492093647915));
#48792=CARTESIAN_POINT('Ctrl Pts',(10.0180552497783,33.5024856413123,-7.64672372347923));
#48793=CARTESIAN_POINT('Ctrl Pts',(10.0180552497783,41.1492093647915,25.855761917833));
#48794=CARTESIAN_POINT('Ctrl Pts',(10.0180552497783,7.64672372347923,33.5024856413123));
#48795=CARTESIAN_POINT('Ctrl Pts',(10.0180552497783,-25.855761917833,41.1492093647915));
#48796=CARTESIAN_POINT('Ctrl Pts',(10.0180552497783,-33.5024856413123,7.64672372347923));
#48797=CARTESIAN_POINT('Ctrl Pts',(10.0180552497783,-41.1492093647915,-25.855761917833));
#48798=CARTESIAN_POINT('Ctrl Pts',(10.0180552497783,-7.64672372347923,-33.5024856413123));
#48799=CARTESIAN_POINT('Ctrl Pts',(9.13857394886632,-7.83777126657544,-34.339519618326));
#48800=CARTESIAN_POINT('Ctrl Pts',(9.13857394886632,26.5017483517505,-42.1772908849014));
#48801=CARTESIAN_POINT('Ctrl Pts',(9.13857394886632,34.339519618326,-7.83777126657544));
#48802=CARTESIAN_POINT('Ctrl Pts',(9.13857394886632,42.1772908849014,26.5017483517505));
#48803=CARTESIAN_POINT('Ctrl Pts',(9.13857394886632,7.83777126657544,34.339519618326));
#48804=CARTESIAN_POINT('Ctrl Pts',(9.13857394886632,-26.5017483517505,42.1772908849014));
#48805=CARTESIAN_POINT('Ctrl Pts',(9.13857394886632,-34.339519618326,7.83777126657544));
#48806=CARTESIAN_POINT('Ctrl Pts',(9.13857394886632,-42.1772908849014,-26.5017483517505));
#48807=CARTESIAN_POINT('Ctrl Pts',(9.13857394886632,-7.83777126657544,-34.339519618326));
#48808=CARTESIAN_POINT('Ctrl Pts',(8.29915429043693,-8.03688232886512,-35.21188218125));
#48809=CARTESIAN_POINT('Ctrl Pts',(8.29915429043693,27.1749998523849,-43.2487645101151));
#48810=CARTESIAN_POINT('Ctrl Pts',(8.29915429043693,35.21188218125,-8.03688232886512));
#48811=CARTESIAN_POINT('Ctrl Pts',(8.29915429043693,43.2487645101151,27.1749998523849));
#48812=CARTESIAN_POINT('Ctrl Pts',(8.29915429043693,8.03688232886512,35.21188218125));
#48813=CARTESIAN_POINT('Ctrl Pts',(8.29915429043693,-27.1749998523849,43.2487645101151));
#48814=CARTESIAN_POINT('Ctrl Pts',(8.29915429043693,-35.21188218125,8.03688232886512));
#48815=CARTESIAN_POINT('Ctrl Pts',(8.29915429043693,-43.2487645101151,-27.1749998523849));
#48816=CARTESIAN_POINT('Ctrl Pts',(8.29915429043693,-8.03688232886512,-35.21188218125));
#48817=CARTESIAN_POINT('Ctrl Pts',(7.4968190344241,-8.24345765802359,-36.1169478341035));
#48818=CARTESIAN_POINT('Ctrl Pts',(7.4968190344241,27.8734901760799,-44.3604054921271));
#48819=CARTESIAN_POINT('Ctrl Pts',(7.4968190344241,36.1169478341035,-8.24345765802359));
#48820=CARTESIAN_POINT('Ctrl Pts',(7.4968190344241,44.3604054921271,27.8734901760799));
#48821=CARTESIAN_POINT('Ctrl Pts',(7.4968190344241,8.24345765802359,36.1169478341035));
#48822=CARTESIAN_POINT('Ctrl Pts',(7.4968190344241,-27.8734901760799,44.3604054921271));
#48823=CARTESIAN_POINT('Ctrl Pts',(7.4968190344241,-36.1169478341035,8.24345765802359));
#48824=CARTESIAN_POINT('Ctrl Pts',(7.4968190344241,-44.3604054921271,-27.8734901760799));
#48825=CARTESIAN_POINT('Ctrl Pts',(7.4968190344241,-8.24345765802359,-36.1169478341035));
#48826=CARTESIAN_POINT('Ctrl Pts',(6.88220761950379,-8.41420410800809,-36.8650369106509));
#48827=CARTESIAN_POINT('Ctrl Pts',(6.88220761950379,28.4508328026428,-45.279241018659));
#48828=CARTESIAN_POINT('Ctrl Pts',(6.88220761950379,36.8650369106509,-8.41420410800809));
#48829=CARTESIAN_POINT('Ctrl Pts',(6.88220761950379,45.279241018659,28.4508328026428));
#48830=CARTESIAN_POINT('Ctrl Pts',(6.88220761950379,8.41420410800809,36.8650369106509));
#48831=CARTESIAN_POINT('Ctrl Pts',(6.88220761950379,-28.4508328026428,45.279241018659));
#48832=CARTESIAN_POINT('Ctrl Pts',(6.88220761950379,-36.8650369106509,8.41420410800809));
#48833=CARTESIAN_POINT('Ctrl Pts',(6.88220761950379,-45.279241018659,-28.4508328026428));
#48834=CARTESIAN_POINT('Ctrl Pts',(6.88220761950379,-8.41420410800809,-36.8650369106509));
#48835=CARTESIAN_POINT('Ctrl Pts',(6.43560997955544,-8.54515448010586,-37.4387679776515));
#48836=CARTESIAN_POINT('Ctrl Pts',(6.43560997955544,28.8936134975456,-45.9839224577573));
#48837=CARTESIAN_POINT('Ctrl Pts',(6.43560997955544,37.4387679776515,-8.54515448010586));
#48838=CARTESIAN_POINT('Ctrl Pts',(6.43560997955544,45.9839224577573,28.8936134975456));
#48839=CARTESIAN_POINT('Ctrl Pts',(6.43560997955544,8.54515448010586,37.4387679776515));
#48840=CARTESIAN_POINT('Ctrl Pts',(6.43560997955544,-28.8936134975456,45.9839224577573));
#48841=CARTESIAN_POINT('Ctrl Pts',(6.43560997955544,-37.4387679776515,8.54515448010586));
#48842=CARTESIAN_POINT('Ctrl Pts',(6.43560997955544,-45.9839224577573,-28.8936134975456));
#48843=CARTESIAN_POINT('Ctrl Pts',(6.43560997955544,-8.54515448010586,-37.4387679776515));
#48844=CARTESIAN_POINT('Ctrl Pts',(6.14415685965718,-8.63371847902027,-37.8267922098931));
#48845=CARTESIAN_POINT('Ctrl Pts',(6.14415685965718,29.1930737308728,-46.4605106889134));
#48846=CARTESIAN_POINT('Ctrl Pts',(6.14415685965718,37.8267922098931,-8.63371847902027));
#48847=CARTESIAN_POINT('Ctrl Pts',(6.14415685965718,46.4605106889134,29.1930737308728));
#48848=CARTESIAN_POINT('Ctrl Pts',(6.14415685965718,8.63371847902027,37.8267922098931));
#48849=CARTESIAN_POINT('Ctrl Pts',(6.14415685965718,-29.1930737308728,46.4605106889134));
#48850=CARTESIAN_POINT('Ctrl Pts',(6.14415685965718,-37.8267922098931,8.63371847902027));
#48851=CARTESIAN_POINT('Ctrl Pts',(6.14415685965718,-46.4605106889134,-29.1930737308728));
#48852=CARTESIAN_POINT('Ctrl Pts',(6.14415685965718,-8.63371847902027,-37.8267922098931));
#48853=CARTESIAN_POINT('Ctrl Pts',(6.,-8.67831642429627,-38.0221885750911));
#48854=CARTESIAN_POINT('Ctrl Pts',(6.,29.3438721507948,-46.7005049993874));
#48855=CARTESIAN_POINT('Ctrl Pts',(6.,38.0221885750911,-8.67831642429627));
#48856=CARTESIAN_POINT('Ctrl Pts',(6.,46.7005049993874,29.3438721507948));
#48857=CARTESIAN_POINT('Ctrl Pts',(6.,8.67831642429627,38.0221885750911));
#48858=CARTESIAN_POINT('Ctrl Pts',(6.,-29.3438721507948,46.7005049993874));
#48859=CARTESIAN_POINT('Ctrl Pts',(6.,-38.0221885750911,8.67831642429627));
#48860=CARTESIAN_POINT('Ctrl Pts',(6.,-46.7005049993874,-29.3438721507948));
#48861=CARTESIAN_POINT('Ctrl Pts',(6.,-8.67831642429627,-38.0221885750911));
#48862=CARTESIAN_POINT('Ctrl Pts',(15.,-0.316722183622945,-30.5983608557452));
#48863=CARTESIAN_POINT('Ctrl Pts',(14.0108432136945,1.17201709431794,-31.2361856660366));
#48864=CARTESIAN_POINT('Ctrl Pts',(13.3692319443824,2.16115069187936,-31.5994041040738));
#48865=CARTESIAN_POINT('Ctrl Pts',(12.3476991724842,3.32436243166655,-32.2576222115046));
#48866=CARTESIAN_POINT('Ctrl Pts',(12.0250187050191,3.69179627058093,-32.4655393067194));
#48867=CARTESIAN_POINT('Ctrl Pts',(11.666631757071,4.09680627482432,-32.7013288419197));
#48868=CARTESIAN_POINT('Ctrl Pts',(11.3593868751765,4.42827966965007,-32.911754584138));
#48869=CARTESIAN_POINT('Ctrl Pts',(10.6767716809131,5.16472407974724,-33.3792637840199));
#48870=CARTESIAN_POINT('Ctrl Pts',(10.1321636914396,5.683315063631,-33.7885713862255));
#48871=CARTESIAN_POINT('Ctrl Pts',(9.56604173138329,6.09942379383306,-34.2764646325745));
#48872=CARTESIAN_POINT('Ctrl Pts',(9.34563078589186,6.26142937765097,-34.466418422242));
#48873=CARTESIAN_POINT('Ctrl Pts',(9.12222951098693,6.4073806230979,-34.6687019818405));
#48874=CARTESIAN_POINT('Ctrl Pts',(8.88860711505275,6.54710572768653,-34.8913321958227));
#48875=CARTESIAN_POINT('Ctrl Pts',(8.7583060070074,6.62503633822089,-35.0155024982899));
#48876=CARTESIAN_POINT('Ctrl Pts',(8.62340343546547,6.70326098334285,-35.1456753402879));
#48877=CARTESIAN_POINT('Ctrl Pts',(8.40819516300417,6.81827896718242,-35.3643373125436));
#48878=CARTESIAN_POINT('Ctrl Pts',(8.02443006829128,7.02338208407037,-35.7542611362568));
#48879=CARTESIAN_POINT('Ctrl Pts',(7.46417034513341,7.28861046704501,-36.3577202537473));
#48880=CARTESIAN_POINT('Ctrl Pts',(6.85957019142019,7.5542785284151,-37.0924815402584));
#48881=CARTESIAN_POINT('Ctrl Pts',(6.58024553736739,7.67701690166778,-37.4319405048412));
#48882=CARTESIAN_POINT('Ctrl Pts',(6.28976782192773,7.7784192013204,-37.8052266187655));
#48883=CARTESIAN_POINT('Ctrl Pts',(6.,7.86863926112478,-38.1979648172293));
#48884=CARTESIAN_POINT('Ctrl Pts',(2.1,2.63423723994462,-15.5859107314896));
#48885=CARTESIAN_POINT('Ctrl Pts',(2.73333333333333,2.63423723994462,-15.5859107314896));
#48886=CARTESIAN_POINT('Ctrl Pts',(3.36803664008728,2.63428404646612,-15.585905949688));
#48887=CARTESIAN_POINT('Ctrl Pts',(4.25277473174135,2.63431300446758,-15.5859022596434));
#48888=CARTESIAN_POINT('Ctrl Pts',(4.7726738795535,2.64263459137918,-15.5845888383648));
#48889=CARTESIAN_POINT('Ctrl Pts',(5.76857447316278,2.66677604587533,-15.580829813117));
#48890=CARTESIAN_POINT('Ctrl Pts',(6.48509167696866,2.66613640606125,-15.5809838465372));
#48891=CARTESIAN_POINT('Ctrl Pts',(6.9986700738739,2.63261167807611,-15.5860120825425));
#48892=CARTESIAN_POINT('Ctrl Pts',(7.1248093702523,2.62413102225182,-15.5873970293984));
#48893=CARTESIAN_POINT('Ctrl Pts',(7.37171220185442,2.60630004336253,-15.5904834561901));
#48894=CARTESIAN_POINT('Ctrl Pts',(7.68212025671799,2.5813014534473,-15.5950682446648));
#48895=CARTESIAN_POINT('Ctrl Pts',(8.05074791674676,2.54617937678925,-15.6015350227393));
#48896=CARTESIAN_POINT('Ctrl Pts',(8.41504712921457,2.50497981155993,-15.6088256864165));
#48897=CARTESIAN_POINT('Ctrl Pts',(9.01075531436909,2.42452722421788,-15.622106164644));
#48898=CARTESIAN_POINT('Ctrl Pts',(9.46310495354993,2.33948796976415,-15.6340319240204));
#48899=CARTESIAN_POINT('Ctrl Pts',(10.2678550072569,2.13947451544829,-15.6566084350139));
#48900=CARTESIAN_POINT('Ctrl Pts',(10.980498717346,1.88789553199322,-15.6910504310237));
#48901=CARTESIAN_POINT('Ctrl Pts',(11.7910302128019,1.5198808624596,-15.7315745004185));
#48902=CARTESIAN_POINT('Ctrl Pts',(12.2471583707382,1.29675740685952,-15.7507502462899));
#48903=CARTESIAN_POINT('Ctrl Pts',(12.4732540168102,1.18219132952897,-15.7583530081557));
#48904=CARTESIAN_POINT('Ctrl Pts',(12.8351236964231,0.996750434719523,-15.7683824294791));
#48905=CARTESIAN_POINT('Ctrl Pts',(13.2802523722939,0.745571188508633,-15.7800984771434));
#48906=CARTESIAN_POINT('Ctrl Pts',(14.1612572117153,0.174593511812138,-15.8002843726132));
#48907=CARTESIAN_POINT('Ctrl Pts',(14.7820737708942,-0.295409261491528,
-15.8007188001297));
#48908=CARTESIAN_POINT('Ctrl Pts',(15.1979896574214,-0.617575400326164,
-15.7866563619325));
#48909=CARTESIAN_POINT('Ctrl Pts',(2.1,4.35569033805583,-23.1280895504496));
#48910=CARTESIAN_POINT('Ctrl Pts',(2.73333333333333,4.35569033805583,-23.1280895504496));
#48911=CARTESIAN_POINT('Ctrl Pts',(3.36872398898381,4.35569062738043,-23.1280874009591));
#48912=CARTESIAN_POINT('Ctrl Pts',(4.25416142982039,4.35570368657663,-23.1280836455188));
#48913=CARTESIAN_POINT('Ctrl Pts',(4.78310679221752,4.36813194564395,-23.125880538704));
#48914=CARTESIAN_POINT('Ctrl Pts',(5.77494665368391,4.4039188556977,-23.1196210211601));
#48915=CARTESIAN_POINT('Ctrl Pts',(6.47498050632645,4.40250321929782,-23.1199364094633));
#48916=CARTESIAN_POINT('Ctrl Pts',(6.96728299632452,4.354093744434,-23.1281247524928));
#48917=CARTESIAN_POINT('Ctrl Pts',(7.09310098340823,4.34153119782086,-23.1304190629282));
#48918=CARTESIAN_POINT('Ctrl Pts',(7.33630050458593,4.31533084892448,-23.1354690138891));
#48919=CARTESIAN_POINT('Ctrl Pts',(7.64237623855619,4.27855698732002,-23.1429403183708));
#48920=CARTESIAN_POINT('Ctrl Pts',(8.00393172538093,4.22710168295328,-23.1534475126223));
#48921=CARTESIAN_POINT('Ctrl Pts',(8.36002498314573,4.1668247936586,-23.1653185047848));
#48922=CARTESIAN_POINT('Ctrl Pts',(8.93969209567688,4.04959492469466,-23.1870206770975));
#48923=CARTESIAN_POINT('Ctrl Pts',(9.37530731609186,3.92607810867588,-23.206753996033));
#48924=CARTESIAN_POINT('Ctrl Pts',(10.1434138046995,3.63794852015698,-23.2448736971823));
#48925=CARTESIAN_POINT('Ctrl Pts',(10.8343054438102,3.27311237366711,-23.302594912175));
#48926=CARTESIAN_POINT('Ctrl Pts',(11.6346922265994,2.73179750623232,-23.3737077261503));
#48927=CARTESIAN_POINT('Ctrl Pts',(12.0872651951508,2.40223791703188,-23.4089168529062));
#48928=CARTESIAN_POINT('Ctrl Pts',(12.3122562294304,2.23255415955555,-23.4236833570785));
#48929=CARTESIAN_POINT('Ctrl Pts',(12.6725938536727,1.95767219781265,-23.4441942800126));
#48930=CARTESIAN_POINT('Ctrl Pts',(13.1110177184242,1.58855368014533,-23.4695074870954));
#48931=CARTESIAN_POINT('Ctrl Pts',(13.9921363954637,0.740833940613477,-23.5179668578115));
#48932=CARTESIAN_POINT('Ctrl Pts',(14.6125773377935,0.0396247240743743,
-23.5335057485051));
#48933=CARTESIAN_POINT('Ctrl Pts',(15.0291266285127,-0.440734376589787,
-23.5225596826963));
#48934=CARTESIAN_POINT('Ctrl Pts',(2.1,6.07714343616704,-30.6702683694095));
#48935=CARTESIAN_POINT('Ctrl Pts',(2.73333333333333,6.07714343616704,-30.6702683694095));
#48936=CARTESIAN_POINT('Ctrl Pts',(3.36945958341804,6.07717722320183,-30.6702656075858));
#48937=CARTESIAN_POINT('Ctrl Pts',(4.25562671182518,6.07721688165371,-30.670259318268));
#48938=CARTESIAN_POINT('Ctrl Pts',(4.79359973395393,6.09396500121367,-30.6671255957162));
#48939=CARTESIAN_POINT('Ctrl Pts',(5.78147401822761,6.14136098671505,-30.6583758536804));
#48940=CARTESIAN_POINT('Ctrl Pts',(6.4648840207481,6.13880226019081,-30.6589606350546));
#48941=CARTESIAN_POINT('Ctrl Pts',(6.93656501913405,6.07755693484608,-30.6698536724228));
#48942=CARTESIAN_POINT('Ctrl Pts',(7.06207690982115,6.06095167183043,-30.6730498747395));
#48943=CARTESIAN_POINT('Ctrl Pts',(7.30170804808245,6.02676597688089,-30.6799788900474));
#48944=CARTESIAN_POINT('Ctrl Pts',(7.60368704328889,5.97877943348734,-30.6902211938605));
#48945=CARTESIAN_POINT('Ctrl Pts',(7.95862439600783,5.9119387988861,-30.7045635161671));
#48946=CARTESIAN_POINT('Ctrl Pts',(8.30733299996974,5.83399140756548,-30.720729237723));
#48947=CARTESIAN_POINT('Ctrl Pts',(8.8731248965081,5.68286843237248,-30.7502492385606));
#48948=CARTESIAN_POINT('Ctrl Pts',(9.29620369485914,5.52518105379277,-30.7769877010294));
#48949=CARTESIAN_POINT('Ctrl Pts',(10.0462911639137,5.15759233537921,-30.8292071711315));
#48950=CARTESIAN_POINT('Ctrl Pts',(10.7405327020582,4.67977587197762,-30.910728379429));
#48951=CARTESIAN_POINT('Ctrl Pts',(11.5482388133752,3.9589695893727,-31.0138279185717));
#48952=CARTESIAN_POINT('Ctrl Pts',(12.0041927687279,3.52013192061582,-31.0656488947084));
#48953=CARTESIAN_POINT('Ctrl Pts',(12.2304250340033,3.29424718610841,-31.0878029021856));
#48954=CARTESIAN_POINT('Ctrl Pts',(12.592462326635,2.92853161577797,-31.1190962862895));
#48955=CARTESIAN_POINT('Ctrl Pts',(13.0427831678653,2.42988806009575,-31.1594573795255));
#48956=CARTESIAN_POINT('Ctrl Pts',(13.9385931776195,1.28678743877928,-31.2371495387447));
#48957=CARTESIAN_POINT('Ctrl Pts',(14.5670688438605,0.345402523233098,-31.2672485558412));
#48958=CARTESIAN_POINT('Ctrl Pts',(14.9853697475044,-0.295704939189027,
-31.2586524717173));
#48959=CARTESIAN_POINT('Ctrl Pts',(2.1,7.79859653427825,-38.2124471883694));
#48960=CARTESIAN_POINT('Ctrl Pts',(2.73333333333333,7.79859653427825,-38.2124471883694));
#48961=CARTESIAN_POINT('Ctrl Pts',(3.37021070699167,7.79865015066291,-38.2124467236009));
#48962=CARTESIAN_POINT('Ctrl Pts',(4.25713136478402,7.79871060554537,-38.2124392001889));
#48963=CARTESIAN_POINT('Ctrl Pts',(4.80403820074332,7.81995661662065,-38.2083337385743));
#48964=CARTESIAN_POINT('Ctrl Pts',(5.78815121291481,7.87887020159365,-38.1971151577803));
#48965=CARTESIAN_POINT('Ctrl Pts',(6.45447266161553,7.87478058883867,-38.1980560957262));
#48966=CARTESIAN_POINT('Ctrl Pts',(6.90692957647958,7.80232226231815,-38.2112861879985));
#48967=CARTESIAN_POINT('Ctrl Pts',(7.032165457778,7.78170112754514,-38.2153789543197));
#48968=CARTESIAN_POINT('Ctrl Pts',(7.26851594405159,7.73982585614224,-38.2241216301496));
#48969=CARTESIAN_POINT('Ctrl Pts',(7.56685490730932,7.6809917809098,-38.2370557901758));
#48970=CARTESIAN_POINT('Ctrl Pts',(7.91607146916962,7.59937001992814,-38.2551036608661));
#48971=CARTESIAN_POINT('Ctrl Pts',(8.25886724527956,7.50440308803594,-38.2754297306033));
#48972=CARTESIAN_POINT('Ctrl Pts',(8.81429346985747,7.32035697382287,-38.3125753180262));
#48973=CARTESIAN_POINT('Ctrl Pts',(9.23055651635836,7.1284382229659,-38.3463705594797));
#48974=CARTESIAN_POINT('Ctrl Pts',(9.97651634618026,6.67420404251485,-38.4141644165199));
#48975=CARTESIAN_POINT('Ctrl Pts',(10.6790339240321,6.07086426145419,-38.5216903207257));
#48976=CARTESIAN_POINT('Ctrl Pts',(11.4920994171454,5.16371480780835,-38.6572666452876));
#48977=CARTESIAN_POINT('Ctrl Pts',(11.9504512124452,4.6129529013925,-38.7257133127446));
#48978=CARTESIAN_POINT('Ctrl Pts',(12.1774804536882,4.33005084296087,-38.7551604165864));
#48979=CARTESIAN_POINT('Ctrl Pts',(12.5406793344479,3.87236046705292,-38.7970589070402));
#48980=CARTESIAN_POINT('Ctrl Pts',(12.997676322199,3.23875815742499,-38.852528788328));
#48981=CARTESIAN_POINT('Ctrl Pts',(13.8994019966035,1.79892708623314,-38.9581992267936));
#48982=CARTESIAN_POINT('Ctrl Pts',(14.5324532885843,0.616949591171014,-39.0018896025419));
#48983=CARTESIAN_POINT('Ctrl Pts',(14.9514110803021,-0.184656989198702,
-38.9949476528204));
#48984=CARTESIAN_POINT('',(3.2,7.48695481785668,-36.8470556158206));
#48985=CARTESIAN_POINT('Ctrl Pts',(3.2,7.48695481785666,-36.8470556158206));
#48986=CARTESIAN_POINT('Ctrl Pts',(3.56152274835393,7.23850467267132,-35.758524406553));
#48987=CARTESIAN_POINT('Ctrl Pts',(3.9522458452532,6.98124869657211,-34.6574817939615));
#48988=CARTESIAN_POINT('Ctrl Pts',(4.78767430123564,6.50176646734495,-32.4570223530551));
#48989=CARTESIAN_POINT('Ctrl Pts',(5.21513946231871,6.28745813065541,-31.4003659031685));
#48990=CARTESIAN_POINT('Ctrl Pts',(6.7954877540227,5.48952449917086,-27.7535421576937));
#48991=CARTESIAN_POINT('Ctrl Pts',(7.94016295938835,4.80756957336196,-25.6343057630554));
#48992=CARTESIAN_POINT('Ctrl Pts',(9.46271935274979,3.88311582182901,-23.0131511987367));
#48993=CARTESIAN_POINT('Ctrl Pts',(10.1385443658991,3.41245828241658,-21.9686504652261));
#48994=CARTESIAN_POINT('Ctrl Pts',(11.5967860400689,2.25751184246001,-19.9258955400566));
#48995=CARTESIAN_POINT('Ctrl Pts',(12.3997356677078,1.62815414544412,-18.8695347898452));
#48996=CARTESIAN_POINT('Ctrl Pts',(13.6850585208118,0.605365893689495,-17.2836977845855));
#48997=CARTESIAN_POINT('Ctrl Pts',(14.3457395898618,0.0481078758601368,
-16.5165260745379));
#48998=CARTESIAN_POINT('Ctrl Pts',(15.,-0.464917847313566,-15.7922717682507));
#48999=CARTESIAN_POINT('Ctrl Pts',(2.79815218354944,7.69629621196739,-37.7641605227833));
#49000=CARTESIAN_POINT('Ctrl Pts',(2.93286301340791,7.62655056963892,-37.4585579619049));
#49001=CARTESIAN_POINT('Ctrl Pts',(3.06773150272457,7.55676145962031,-37.1527603668643));
#49002=CARTESIAN_POINT('Ctrl Pts',(3.20258453830003,7.48699350665232,-36.8470540770711));
#49003=CARTESIAN_POINT('Origin',(2.9,0.,0.));
#49004=CARTESIAN_POINT('',(3.2,-7.48695481785666,-36.8470556158206));
#49005=CARTESIAN_POINT('Origin',(3.2,0.,0.));
#49006=CARTESIAN_POINT('Ctrl Pts',(3.19856230423365,-7.48704093025229,-36.8470163272698));
#49007=CARTESIAN_POINT('Ctrl Pts',(3.0644392731241,-7.55683434047029,-37.1528795715508));
#49008=CARTESIAN_POINT('Ctrl Pts',(2.93031838720717,-7.62661528615582,-37.4586872363272));
#49009=CARTESIAN_POINT('Ctrl Pts',(2.79630735614137,-7.69631837557393,-37.7641425125794));
#49010=CARTESIAN_POINT('Ctrl Pts',(2.1,-9.137400984347,-12.90142634814));
#49011=CARTESIAN_POINT('Ctrl Pts',(2.73333333333333,-9.137400984347,-12.90142634814));
#49012=CARTESIAN_POINT('Ctrl Pts',(3.365973712246,-9.13746504152622,-12.9013637498414));
#49013=CARTESIAN_POINT('Ctrl Pts',(4.12348671872558,-9.13748461543386,-12.9013444788804));
#49014=CARTESIAN_POINT('Ctrl Pts',(4.36308068280113,-9.13590525422836,-12.9024878598794));
#49015=CARTESIAN_POINT('Ctrl Pts',(4.85756687529509,-9.12862669836929,-12.9077725838742));
#49016=CARTESIAN_POINT('Ctrl Pts',(5.73898782434893,-9.11132026423094,-12.9203618153208));
#49017=CARTESIAN_POINT('Ctrl Pts',(6.52605775660734,-9.11084083138628,-12.9207276583753));
#49018=CARTESIAN_POINT('Ctrl Pts',(7.12756933428754,-9.14287723972839,-12.8972432395004));
#49019=CARTESIAN_POINT('Ctrl Pts',(7.25506469988018,-9.14994617799211,-12.8921744658959));
#49020=CARTESIAN_POINT('Ctrl Pts',(7.51732351444062,-9.16567242155789,-12.8811147657457));
#49021=CARTESIAN_POINT('Ctrl Pts',(7.84589135656503,-9.18794199222896,-12.8657492998081));
#49022=CARTESIAN_POINT('Ctrl Pts',(8.24417023302519,-9.21975289392636,-12.8438195891331));
#49023=CARTESIAN_POINT('Ctrl Pts',(8.77647055639935,-9.27004204587853,-12.8086070647954));
#49024=CARTESIAN_POINT('Ctrl Pts',(9.44114142908682,-9.34965285699896,-12.7510329694809));
#49025=CARTESIAN_POINT('Ctrl Pts',(9.96389223057755,-9.43618098671083,-12.6847093516977));
#49026=CARTESIAN_POINT('Ctrl Pts',(11.1189211579548,-9.66280193839667,-12.5054821536567));
#49027=CARTESIAN_POINT('Ctrl Pts',(12.080463293236,-9.98373232849783,-12.2611717068893));
#49028=CARTESIAN_POINT('Ctrl Pts',(13.0008495768038,-10.3265199570838,-11.9667211468366));
#49029=CARTESIAN_POINT('Ctrl Pts',(13.2108260900368,-10.4056770861943,-11.8966961179284));
#49030=CARTESIAN_POINT('Ctrl Pts',(13.3144491940718,-10.4448306117047,-11.8614746909584));
#49031=CARTESIAN_POINT('Ctrl Pts',(13.3733290414177,-10.4670878289521,-11.8412790539105));
#49032=CARTESIAN_POINT('Ctrl Pts',(13.4026082954906,-10.4781554201219,-11.8311771752724));
#49033=CARTESIAN_POINT('Ctrl Pts',(13.6877981560128,-10.5859241331148,-11.732479296786));
#49034=CARTESIAN_POINT('Ctrl Pts',(14.2465882704735,-10.8170217282857,-11.5176433731241));
#49035=CARTESIAN_POINT('Ctrl Pts',(14.7537307590314,-11.056004238249,-11.2866625718643));
#49036=CARTESIAN_POINT('Ctrl Pts',(14.9999999999997,-11.1762403837995,-11.167078717827));
#49037=CARTESIAN_POINT('Ctrl Pts',(2.1,-13.9602886030972,-18.9491361350573));
#49038=CARTESIAN_POINT('Ctrl Pts',(2.73333333333333,-13.9602886030972,-18.9491361350573));
#49039=CARTESIAN_POINT('Ctrl Pts',(3.36558929933722,-13.9603388813315,-18.949091413765));
#49040=CARTESIAN_POINT('Ctrl Pts',(4.12268680117359,-13.9603530925967,-18.9490786756313));
#49041=CARTESIAN_POINT('Ctrl Pts',(4.35700071618798,-13.9580622630443,-18.9508062100769));
#49042=CARTESIAN_POINT('Ctrl Pts',(4.84800506483027,-13.9474262305624,-18.9588441525132));
#49043=CARTESIAN_POINT('Ctrl Pts',(5.73069160467532,-13.9219831875589,-18.9780946562289));
#49044=CARTESIAN_POINT('Ctrl Pts',(6.53595554087845,-13.9209135422454,-18.9789455178027));
#49045=CARTESIAN_POINT('Ctrl Pts',(7.15870948280726,-13.969072695455,-18.9423072738915));
#49046=CARTESIAN_POINT('Ctrl Pts',(7.28653449300648,-13.9794730149236,-18.9345516012843));
#49047=CARTESIAN_POINT('Ctrl Pts',(7.55249858901944,-14.0027853431907,-18.9175010740327));
#49048=CARTESIAN_POINT('Ctrl Pts',(7.8854250805442,-14.0357701876927,-18.893829697599));
#49049=CARTESIAN_POINT('Ctrl Pts',(8.29077969779674,-14.0830375031778,-18.8599241823138));
#49050=CARTESIAN_POINT('Ctrl Pts',(8.83405094145081,-14.1578675644896,-18.805435373411));
#49051=CARTESIAN_POINT('Ctrl Pts',(9.51599654655467,-14.2767190591612,-18.7161020141187));
#49052=CARTESIAN_POINT('Ctrl Pts',(10.0563180414682,-14.4064700137606,-18.6129001575941));
#49053=CARTESIAN_POINT('Ctrl Pts',(11.2545469680855,-14.7474852276745,-18.3333024528578));
#49054=CARTESIAN_POINT('Ctrl Pts',(12.2342109401188,-15.2253867757627,-17.9550408590473));
#49055=CARTESIAN_POINT('Ctrl Pts',(13.160804185079,-15.7295857192779,-17.5044322625813));
#49056=CARTESIAN_POINT('Ctrl Pts',(13.3719043594969,-15.8458680331158,-17.3974114070575));
#49057=CARTESIAN_POINT('Ctrl Pts',(13.4759524598702,-15.903315763404,-17.3436343217885));
#49058=CARTESIAN_POINT('Ctrl Pts',(13.5350561403457,-15.9359605015101,-17.3128100925608));
#49059=CARTESIAN_POINT('Ctrl Pts',(13.5644260429486,-15.9521864940619,-17.2973960592047));
#49060=CARTESIAN_POINT('Ctrl Pts',(13.8509127097168,-16.1101904313627,-17.1468470987892));
#49061=CARTESIAN_POINT('Ctrl Pts',(14.4159152208145,-16.4514462123258,-16.8174302408524));
#49062=CARTESIAN_POINT('Ctrl Pts',(14.9236315787721,-16.8008746420588,-16.4663087459205));
#49063=CARTESIAN_POINT('Ctrl Pts',(15.169681381964,-16.9765158478446,-16.2846381189209));
#49064=CARTESIAN_POINT('Ctrl Pts',(2.1,-18.7831762218474,-24.9968459219746));
#49065=CARTESIAN_POINT('Ctrl Pts',(2.73333333333333,-18.7831762218474,-24.9968459219746));
#49066=CARTESIAN_POINT('Ctrl Pts',(3.3651198397079,-18.7832600991187,-24.9967641409249));
#49067=CARTESIAN_POINT('Ctrl Pts',(4.12177662671699,-18.7832835494852,-24.9967408050916));
#49068=CARTESIAN_POINT('Ctrl Pts',(4.35079814858358,-18.7803301229489,-24.9990120557395));
#49069=CARTESIAN_POINT('Ctrl Pts',(4.83833501195452,-18.7664351600051,-25.0097212931742));
#49070=CARTESIAN_POINT('Ctrl Pts',(5.72217492112382,-18.7328455282091,-25.0356357989273));
#49071=CARTESIAN_POINT('Ctrl Pts',(6.54572526829364,-18.7308544639692,-25.0372090892692));
#49072=CARTESIAN_POINT('Ctrl Pts',(7.189043387547,-18.7967679600979,-24.9861010385379));
#49073=CARTESIAN_POINT('Ctrl Pts',(7.31718157815736,-18.8105293955174,-24.9756330333963));
#49074=CARTESIAN_POINT('Ctrl Pts',(7.58671359051966,-18.84173419862,-24.9523431866193));
#49075=CARTESIAN_POINT('Ctrl Pts',(7.92374496455099,-18.8858694172611,-24.9200041574497));
#49076=CARTESIAN_POINT('Ctrl Pts',(8.33571713696631,-18.9493544240891,-24.8735000521768));
#49077=CARTESIAN_POINT('Ctrl Pts',(8.88883102789065,-19.0501590221844,-24.7985395646899));
#49078=CARTESIAN_POINT('Ctrl Pts',(9.58538130299016,-19.2109486375985,-24.6751859365789));
#49079=CARTESIAN_POINT('Ctrl Pts',(10.1375693358685,-19.3872925255919,-24.5321887728776));
#49080=CARTESIAN_POINT('Ctrl Pts',(11.3565468230311,-19.8503443148555,-24.1453469673367));
#49081=CARTESIAN_POINT('Ctrl Pts',(12.3228318792994,-20.4809300681266,-23.6358069932934));
#49082=CARTESIAN_POINT('Ctrl Pts',(13.2438497514686,-21.1419847785548,-23.0329488931636));
#49083=CARTESIAN_POINT('Ctrl Pts',(13.4536958211944,-21.2946007618859,-22.8895961528565));
#49084=CARTESIAN_POINT('Ctrl Pts',(13.5572593885355,-21.3699791139417,-22.8175746974478));
#49085=CARTESIAN_POINT('Ctrl Pts',(13.6160986444917,-21.4128228536293,-22.7762818189615));
#49086=CARTESIAN_POINT('Ctrl Pts',(13.645355806218,-21.4341190597128,-22.755631186663));
#49087=CARTESIAN_POINT('Ctrl Pts',(13.9304427285216,-21.6415024695375,-22.5539291559155));
#49088=CARTESIAN_POINT('Ctrl Pts',(14.4834792629394,-22.0842177076207,-22.1185350536073));
#49089=CARTESIAN_POINT('Ctrl Pts',(14.98335392639,-22.5380437985113,-21.6541002484824));
#49090=CARTESIAN_POINT('Ctrl Pts',(15.2260186760796,-22.7662639303248,-21.4137725438282));
#49091=CARTESIAN_POINT('Ctrl Pts',(2.1,-23.6060638405976,-31.0445557088918));
#49092=CARTESIAN_POINT('Ctrl Pts',(2.73333333333333,-23.6060638405976,-31.0445557088918));
#49093=CARTESIAN_POINT('Ctrl Pts',(3.36464153971337,-23.6061551620833,-31.0444583481246));
#49094=CARTESIAN_POINT('Ctrl Pts',(4.12085950545642,-23.6061797565327,-31.0444310988732));
#49095=CARTESIAN_POINT('Ctrl Pts',(4.34457587227524,-23.6026038074475,-31.0472140637149));
#49096=CARTESIAN_POINT('Ctrl Pts',(4.82871915333435,-23.5855404636303,-31.0605229321991));
#49097=CARTESIAN_POINT('Ctrl Pts',(5.71350842690898,-23.543739000069,-31.0931529169989));
#49098=CARTESIAN_POINT('Ctrl Pts',(6.55584786131197,-23.5404886370307,-31.0957210166559));
#49099=CARTESIAN_POINT('Ctrl Pts',(7.21833910031285,-23.6254456564365,-31.0291118651101));
#49100=CARTESIAN_POINT('Ctrl Pts',(7.34676118501293,-23.6425884371248,-31.0159144331966));
#49101=CARTESIAN_POINT('Ctrl Pts',(7.61957283623088,-23.6819205403188,-30.986195335862));
#49102=CARTESIAN_POINT('Ctrl Pts',(7.96026153975009,-23.7374867325871,-30.944960085127));
#49103=CARTESIAN_POINT('Ctrl Pts',(8.37794406069148,-23.8176688187955,-30.8854641795912));
#49104=CARTESIAN_POINT('Ctrl Pts',(8.93897958734005,-23.9451060235987,-30.7894856598615));
#49105=CARTESIAN_POINT('Ctrl Pts',(9.64589610894272,-24.1485645677299,-30.6314814118357));
#49106=CARTESIAN_POINT('Ctrl Pts',(10.2035826747735,-24.3705984027494,-30.4493953450365));
#49107=CARTESIAN_POINT('Ctrl Pts',(11.4269764335898,-24.9486838559586,-29.9611336557811));
#49108=CARTESIAN_POINT('Ctrl Pts',(12.3794613911947,-25.7205660291737,-29.3307527404956));
#49109=CARTESIAN_POINT('Ctrl Pts',(13.2972801181681,-26.536248516985,-28.5788115668798));
#49110=CARTESIAN_POINT('Ctrl Pts',(13.5062492987541,-26.7246568894861,-28.3998656781212));
#49111=CARTESIAN_POINT('Ctrl Pts',(13.6095218510944,-26.8178025811325,-28.30987870928));
#49112=CARTESIAN_POINT('Ctrl Pts',(13.6681948654715,-26.8707551741385,-28.2582726202542));
#49113=CARTESIAN_POINT('Ctrl Pts',(13.6973873567982,-26.8970881889659,-28.2324525330172));
#49114=CARTESIAN_POINT('Ctrl Pts',(13.9814825393856,-27.1533540380845,-27.980413093245));
#49115=CARTESIAN_POINT('Ctrl Pts',(14.5280933440888,-27.6942372345927,-27.4431392305571));
#49116=CARTESIAN_POINT('Ctrl Pts',(15.0243070371674,-28.25234233925,-26.8665204433862));
#49117=CARTESIAN_POINT('Ctrl Pts',(15.2656150130537,-28.5332835802564,-26.5678972425624));
#49118=CARTESIAN_POINT('',(3.2,-22.7328514723457,-29.9495820327475));
#49119=CARTESIAN_POINT('Ctrl Pts',(3.19847306248522,-22.7329107976785,-29.9495195044252));
#49120=CARTESIAN_POINT('Ctrl Pts',(3.06436549823724,-22.9285035669014,-30.1948090414568));
#49121=CARTESIAN_POINT('Ctrl Pts',(2.93026080897388,-23.1240595470582,-30.4400531793895));
#49122=CARTESIAN_POINT('Ctrl Pts',(2.79626461758213,-23.3193910750582,-30.6850129088235));
#49123=CARTESIAN_POINT('',(15.,-11.1762403838096,-11.1670787178359));
#49124=CARTESIAN_POINT('Ctrl Pts',(15.,-11.1762403838096,-11.1670787178359));
#49125=CARTESIAN_POINT('Ctrl Pts',(14.4897165779515,-11.3373685343331,-11.7879945733865));
#49126=CARTESIAN_POINT('Ctrl Pts',(13.983380302661,-11.5187060499957,-12.4208731978426));
#49127=CARTESIAN_POINT('Ctrl Pts',(13.4460287676664,-11.7567539704294,-13.1013698964346));
#49128=CARTESIAN_POINT('Ctrl Pts',(12.8282655681033,-12.0304244364084,-13.8836991361168));
#49129=CARTESIAN_POINT('Ctrl Pts',(12.155541408943,-12.3493763587429,-14.7928054072806));
#49130=CARTESIAN_POINT('Ctrl Pts',(11.5904908073501,-12.6688779184396,-15.5748537094225));
#49131=CARTESIAN_POINT('Ctrl Pts',(11.1143368259573,-12.9381138758599,-16.2338662149516));
#49132=CARTESIAN_POINT('Ctrl Pts',(10.6953158949572,-13.2106621367002,-16.8262345756793));
#49133=CARTESIAN_POINT('Ctrl Pts',(10.2957959918397,-13.5071054931829,-17.3951211088922));
#49134=CARTESIAN_POINT('Ctrl Pts',(10.0450888109402,-13.6931299631035,-17.7521094288247));
#49135=CARTESIAN_POINT('Ctrl Pts',(9.80235305581407,-13.8878822107991,-18.1003493308506));
#49136=CARTESIAN_POINT('Ctrl Pts',(9.56010106233158,-14.0947279826892,-18.4527330693702));
#49137=CARTESIAN_POINT('Ctrl Pts',(9.36613602939727,-14.2603441511269,-18.7348778000075));
#49138=CARTESIAN_POINT('Ctrl Pts',(9.15248571294299,-14.4499421458783,-19.0480702412718));
#49139=CARTESIAN_POINT('Ctrl Pts',(8.89022359824486,-14.6989807980091,-19.4411359839043));
#49140=CARTESIAN_POINT('Ctrl Pts',(8.39222406105985,-15.1718708059503,-20.1875135464416));
#49141=CARTESIAN_POINT('Ctrl Pts',(7.76643777374077,-15.8240081907589,-21.153333731125));
#49142=CARTESIAN_POINT('Ctrl Pts',(7.10363554123528,-16.6157830223697,-22.2694187973552));
#49143=CARTESIAN_POINT('Ctrl Pts',(6.23550018248711,-17.6528461066184,-23.7312619563649));
#49144=CARTESIAN_POINT('Ctrl Pts',(5.31040885822698,-19.033253690729,-25.3709340011067));
#49145=CARTESIAN_POINT('Ctrl Pts',(4.46416616904233,-20.4648153103685,-27.11999472538));
#49146=CARTESIAN_POINT('Ctrl Pts',(4.30741751124418,-20.7299819880861,-27.4439714337655));
#49147=CARTESIAN_POINT('Ctrl Pts',(4.15262292089009,-20.9971466932259,-27.7730770818396));
#49148=CARTESIAN_POINT('Ctrl Pts',(4.,-21.2644490398942,-28.1082636227258));
#49149=CARTESIAN_POINT('Ctrl Pts',(3.72434973283395,-21.7472203225005,-28.7136396632767));
#49150=CARTESIAN_POINT('Ctrl Pts',(3.45587123478816,-22.240150328922,-29.331754340573));
#49151=CARTESIAN_POINT('Ctrl Pts',(3.2,-22.7328514723457,-29.9495820327474));
#49152=CARTESIAN_POINT('',(15.,-22.0807120920212,-21.1849511094378));
#49153=CARTESIAN_POINT('Ctrl Pts',(15.,-22.0807120920212,-21.1849511094378));
#49154=CARTESIAN_POINT('Ctrl Pts',(15.,-18.8408082676135,-18.1865559292736));
#49155=CARTESIAN_POINT('Ctrl Pts',(15.,-14.9884313390737,-14.634232602943));
#49156=CARTESIAN_POINT('Ctrl Pts',(15.,-11.1762403838096,-11.1670787178359));
#49157=CARTESIAN_POINT('Ctrl Pts',(6.,-23.5490023259382,-31.0876903203335));
#49158=CARTESIAN_POINT('Ctrl Pts',(6.38595465246567,-23.2149712390509,-30.6675553675066));
#49159=CARTESIAN_POINT('Ctrl Pts',(6.77023648668261,-22.9202307074269,-30.25978773824));
#49160=CARTESIAN_POINT('Ctrl Pts',(7.13915213286206,-22.6798798515873,-29.8657998307839));
#49161=CARTESIAN_POINT('Ctrl Pts',(8.10667920093245,-22.049529902305,-28.8325176458075));
#49162=CARTESIAN_POINT('Ctrl Pts',(8.98019888747386,-21.6690144845904,-27.9844578967108));
#49163=CARTESIAN_POINT('Ctrl Pts',(9.46656009721089,-21.5060718063769,-27.502383186396));
#49164=CARTESIAN_POINT('Ctrl Pts',(9.65648624874925,-21.4424419872736,-27.3141309313826));
#49165=CARTESIAN_POINT('Ctrl Pts',(9.79228848853745,-21.4038352459001,-27.1792029279711));
#49166=CARTESIAN_POINT('Ctrl Pts',(9.94593825727835,-21.3652548270746,-27.0254911176928));
#49167=CARTESIAN_POINT('Ctrl Pts',(10.106574086601,-21.3249202556369,-26.8647904259633));
#49168=CARTESIAN_POINT('Ctrl Pts',(10.2660951669676,-21.291919485225,-26.7040013107996));
#49169=CARTESIAN_POINT('Ctrl Pts',(10.4261869573617,-21.2667017567949,-26.5402002816529));
#49170=CARTESIAN_POINT('Ctrl Pts',(10.8065549509411,-21.2067860250638,-26.151019370818));
#49171=CARTESIAN_POINT('Ctrl Pts',(11.1894211925257,-21.1918047278973,-25.7443677774521));
#49172=CARTESIAN_POINT('Ctrl Pts',(11.6023503255242,-21.2187986652524,-25.2875487721924));
#49173=CARTESIAN_POINT('Ctrl Pts',(11.7531893954247,-21.2286592928473,-25.1206771509872));
#49174=CARTESIAN_POINT('Ctrl Pts',(11.9080270687775,-21.2442649897398,-24.9470697549615));
#49175=CARTESIAN_POINT('Ctrl Pts',(12.068176613168,-21.2657353562899,-24.7650851418614));
#49176=CARTESIAN_POINT('Ctrl Pts',(12.1838435903475,-21.2812421902758,-24.6336479269097));
#49177=CARTESIAN_POINT('Ctrl Pts',(12.3100865410161,-21.2996793030358,-24.48952991587));
#49178=CARTESIAN_POINT('Ctrl Pts',(12.5127093730712,-21.3376417331468,-24.2542638313305));
#49179=CARTESIAN_POINT('Ctrl Pts',(12.7975492664042,-21.3910079527075,-23.9235352271283));
#49180=CARTESIAN_POINT('Ctrl Pts',(13.1874566943566,-21.4810061462248,-23.462026248552));
#49181=CARTESIAN_POINT('Ctrl Pts',(13.6431584568239,-21.600000204035,-22.9185284970073));
#49182=CARTESIAN_POINT('Ctrl Pts',(14.069523646534,-21.7113338178396,-22.4100193337122));
#49183=CARTESIAN_POINT('Ctrl Pts',(14.53311408767,-21.878316911732,-21.8202269155209));
#49184=CARTESIAN_POINT('Ctrl Pts',(15.,-22.0807120920212,-21.1849511094378));
#49185=CARTESIAN_POINT('Origin',(15.,-7.65823537717056,-3.68801178249924));
#49186=CARTESIAN_POINT('',(15.,-12.6367667846116,-9.48283298589492));
#49187=CARTESIAN_POINT('Ctrl Pts',(15.,-12.6367667846116,-9.48283298589491));
#49188=CARTESIAN_POINT('Ctrl Pts',(15.,-12.1910490642079,-10.0767937666962));
#49189=CARTESIAN_POINT('Ctrl Pts',(15.,-11.7031502151664,-10.6397366004717));
#49190=CARTESIAN_POINT('Ctrl Pts',(15.,-11.1762403838096,-11.1670787178359));
#49191=CARTESIAN_POINT('',(15.,-24.1202348804503,-18.8301425727982));
#49192=CARTESIAN_POINT('Ctrl Pts',(15.,-12.6367667846116,-9.48283298589491));
#49193=CARTESIAN_POINT('Ctrl Pts',(15.,-16.7264630501964,-12.8512910730167));
#49194=CARTESIAN_POINT('Ctrl Pts',(15.,-20.8784875564221,-16.2131979243164));
#49195=CARTESIAN_POINT('Ctrl Pts',(15.,-24.1202348804503,-18.8301425727982));
#49196=CARTESIAN_POINT('Origin',(15.,0.,0.));
#49197=CARTESIAN_POINT('Ctrl Pts',(15.,-27.569647357814,-13.2768424169973));
#49198=CARTESIAN_POINT('Ctrl Pts',(15.,-14.2928049408167,-40.8464897748113));
#49199=CARTESIAN_POINT('Ctrl Pts',(15.,13.2768424169973,-27.569647357814));
#49200=CARTESIAN_POINT('Ctrl Pts',(15.,40.8464897748113,-14.2928049408167));
#49201=CARTESIAN_POINT('Ctrl Pts',(15.,27.569647357814,13.2768424169973));
#49202=CARTESIAN_POINT('Ctrl Pts',(15.,14.2928049408167,40.8464897748113));
#49203=CARTESIAN_POINT('Ctrl Pts',(15.,-13.2768424169973,27.569647357814));
#49204=CARTESIAN_POINT('Ctrl Pts',(15.,-40.8464897748113,14.2928049408167));
#49205=CARTESIAN_POINT('Ctrl Pts',(15.,-27.569647357814,-13.2768424169973));
#49206=CARTESIAN_POINT('Ctrl Pts',(14.7843073131059,-27.6919221166174,-13.3357268373578));
#49207=CARTESIAN_POINT('Ctrl Pts',(14.7843073131059,-14.3561952792596,-41.0276489539752));
#49208=CARTESIAN_POINT('Ctrl Pts',(14.7843073131059,13.3357268373578,-27.6919221166174));
#49209=CARTESIAN_POINT('Ctrl Pts',(14.7843073131059,41.0276489539752,-14.3561952792596));
#49210=CARTESIAN_POINT('Ctrl Pts',(14.7843073131059,27.6919221166174,13.3357268373578));
#49211=CARTESIAN_POINT('Ctrl Pts',(14.7843073131059,14.3561952792596,41.0276489539752));
#49212=CARTESIAN_POINT('Ctrl Pts',(14.7843073131059,-13.3357268373578,27.6919221166174));
#49213=CARTESIAN_POINT('Ctrl Pts',(14.7843073131059,-41.0276489539752,14.3561952792596));
#49214=CARTESIAN_POINT('Ctrl Pts',(14.7843073131059,-27.6919221166174,-13.3357268373578));
#49215=CARTESIAN_POINT('Ctrl Pts',(14.3560298066371,-27.9390044129707,-13.4547154000382));
#49216=CARTESIAN_POINT('Ctrl Pts',(14.3560298066371,-14.4842890129325,-41.3937198130088));
#49217=CARTESIAN_POINT('Ctrl Pts',(14.3560298066371,13.4547154000382,-27.9390044129707));
#49218=CARTESIAN_POINT('Ctrl Pts',(14.3560298066371,41.3937198130088,-14.4842890129325));
#49219=CARTESIAN_POINT('Ctrl Pts',(14.3560298066371,27.9390044129707,13.4547154000382));
#49220=CARTESIAN_POINT('Ctrl Pts',(14.3560298066371,14.4842890129325,41.3937198130088));
#49221=CARTESIAN_POINT('Ctrl Pts',(14.3560298066371,-13.4547154000382,27.9390044129707));
#49222=CARTESIAN_POINT('Ctrl Pts',(14.3560298066371,-41.3937198130088,14.4842890129325));
#49223=CARTESIAN_POINT('Ctrl Pts',(14.3560298066371,-27.9390044129707,-13.4547154000382));
#49224=CARTESIAN_POINT('Ctrl Pts',(13.722936818686,-28.3172259246361,-13.6368572803433));
#49225=CARTESIAN_POINT('Ctrl Pts',(13.722936818686,-14.6803686442928,-41.9540832049794));
#49226=CARTESIAN_POINT('Ctrl Pts',(13.722936818686,13.6368572803433,-28.3172259246361));
#49227=CARTESIAN_POINT('Ctrl Pts',(13.722936818686,41.9540832049794,-14.6803686442928));
#49228=CARTESIAN_POINT('Ctrl Pts',(13.722936818686,28.3172259246361,13.6368572803433));
#49229=CARTESIAN_POINT('Ctrl Pts',(13.722936818686,14.6803686442928,41.9540832049794));
#49230=CARTESIAN_POINT('Ctrl Pts',(13.722936818686,-13.6368572803433,28.3172259246361));
#49231=CARTESIAN_POINT('Ctrl Pts',(13.722936818686,-41.9540832049794,14.6803686442928));
#49232=CARTESIAN_POINT('Ctrl Pts',(13.722936818686,-28.3172259246361,-13.6368572803433));
#49233=CARTESIAN_POINT('Ctrl Pts',(12.8977690042853,-28.8369697397467,-13.8871527099828));
#49234=CARTESIAN_POINT('Ctrl Pts',(12.8977690042853,-14.949817029764,-42.7241224497295));
#49235=CARTESIAN_POINT('Ctrl Pts',(12.8977690042853,13.8871527099828,-28.8369697397467));
#49236=CARTESIAN_POINT('Ctrl Pts',(12.8977690042853,42.7241224497295,-14.949817029764));
#49237=CARTESIAN_POINT('Ctrl Pts',(12.8977690042853,28.8369697397467,13.8871527099828));
#49238=CARTESIAN_POINT('Ctrl Pts',(12.8977690042853,14.949817029764,42.7241224497295));
#49239=CARTESIAN_POINT('Ctrl Pts',(12.8977690042853,-13.8871527099828,28.8369697397467));
#49240=CARTESIAN_POINT('Ctrl Pts',(12.8977690042853,-42.7241224497295,14.949817029764));
#49241=CARTESIAN_POINT('Ctrl Pts',(12.8977690042853,-28.8369697397467,-13.8871527099828));
#49242=CARTESIAN_POINT('Ctrl Pts',(11.9000549946031,-29.5141508562392,-14.2132659480213));
#49243=CARTESIAN_POINT('Ctrl Pts',(11.9000549946031,-15.3008849082179,-43.7274168042605));
#49244=CARTESIAN_POINT('Ctrl Pts',(11.9000549946031,14.2132659480213,-29.5141508562392));
#49245=CARTESIAN_POINT('Ctrl Pts',(11.9000549946031,43.7274168042605,-15.3008849082179));
#49246=CARTESIAN_POINT('Ctrl Pts',(11.9000549946031,29.5141508562392,14.2132659480213));
#49247=CARTESIAN_POINT('Ctrl Pts',(11.9000549946031,15.3008849082179,43.7274168042605));
#49248=CARTESIAN_POINT('Ctrl Pts',(11.9000549946031,-14.2132659480213,29.5141508562392));
#49249=CARTESIAN_POINT('Ctrl Pts',(11.9000549946031,-43.7274168042605,15.3008849082179));
#49250=CARTESIAN_POINT('Ctrl Pts',(11.9000549946031,-29.5141508562392,-14.2132659480213));
#49251=CARTESIAN_POINT('Ctrl Pts',(10.9391333834985,-30.2213162016529,-14.5538188296728));
#49252=CARTESIAN_POINT('Ctrl Pts',(10.9391333834985,-15.6674973719801,-44.7751350313257));
#49253=CARTESIAN_POINT('Ctrl Pts',(10.9391333834985,14.5538188296728,-30.2213162016529));
#49254=CARTESIAN_POINT('Ctrl Pts',(10.9391333834985,44.7751350313257,-15.6674973719801));
#49255=CARTESIAN_POINT('Ctrl Pts',(10.9391333834985,30.2213162016529,14.5538188296728));
#49256=CARTESIAN_POINT('Ctrl Pts',(10.9391333834985,15.6674973719801,44.7751350313257));
#49257=CARTESIAN_POINT('Ctrl Pts',(10.9391333834985,-14.5538188296728,30.2213162016529));
#49258=CARTESIAN_POINT('Ctrl Pts',(10.9391333834985,-44.7751350313257,15.6674973719801));
#49259=CARTESIAN_POINT('Ctrl Pts',(10.9391333834985,-30.2213162016529,-14.5538188296728));
#49260=CARTESIAN_POINT('Ctrl Pts',(10.0180552497783,-30.9609522745316,-14.9100087895256));
#49261=CARTESIAN_POINT('Ctrl Pts',(10.0180552497783,-16.050943485006,-45.8709610640572));
#49262=CARTESIAN_POINT('Ctrl Pts',(10.0180552497783,14.9100087895256,-30.9609522745316));
#49263=CARTESIAN_POINT('Ctrl Pts',(10.0180552497783,45.8709610640572,-16.050943485006));
#49264=CARTESIAN_POINT('Ctrl Pts',(10.0180552497783,30.9609522745316,14.9100087895256));
#49265=CARTESIAN_POINT('Ctrl Pts',(10.0180552497783,16.050943485006,45.8709610640572));
#49266=CARTESIAN_POINT('Ctrl Pts',(10.0180552497783,-14.9100087895256,30.9609522745316));
#49267=CARTESIAN_POINT('Ctrl Pts',(10.0180552497783,-45.8709610640572,16.050943485006));
#49268=CARTESIAN_POINT('Ctrl Pts',(10.0180552497783,-30.9609522745316,-14.9100087895256));
#49269=CARTESIAN_POINT('Ctrl Pts',(9.13857394886632,-31.734487984447,-15.2825239541621));
#49270=CARTESIAN_POINT('Ctrl Pts',(9.13857394886632,-16.4519640302848,-47.0170119386091));
#49271=CARTESIAN_POINT('Ctrl Pts',(9.13857394886632,15.2825239541621,-31.734487984447));
#49272=CARTESIAN_POINT('Ctrl Pts',(9.13857394886632,47.0170119386091,-16.4519640302848));
#49273=CARTESIAN_POINT('Ctrl Pts',(9.13857394886632,31.734487984447,15.2825239541621));
#49274=CARTESIAN_POINT('Ctrl Pts',(9.13857394886632,16.4519640302848,47.0170119386091));
#49275=CARTESIAN_POINT('Ctrl Pts',(9.13857394886632,-15.2825239541621,31.734487984447));
#49276=CARTESIAN_POINT('Ctrl Pts',(9.13857394886632,-47.0170119386091,16.4519640302848));
#49277=CARTESIAN_POINT('Ctrl Pts',(9.13857394886632,-31.734487984447,-15.2825239541621));
#49278=CARTESIAN_POINT('Ctrl Pts',(8.29915429043693,-32.5406722170424,-15.6707618186629));
#49279=CARTESIAN_POINT('Ctrl Pts',(8.29915429043693,-16.8699103983795,-48.2114340357053));
#49280=CARTESIAN_POINT('Ctrl Pts',(8.29915429043693,15.6707618186629,-32.5406722170424));
#49281=CARTESIAN_POINT('Ctrl Pts',(8.29915429043693,48.2114340357053,-16.8699103983795));
#49282=CARTESIAN_POINT('Ctrl Pts',(8.29915429043693,32.5406722170424,15.6707618186629));
#49283=CARTESIAN_POINT('Ctrl Pts',(8.29915429043693,16.8699103983795,48.2114340357053));
#49284=CARTESIAN_POINT('Ctrl Pts',(8.29915429043693,-15.6707618186629,32.5406722170424));
#49285=CARTESIAN_POINT('Ctrl Pts',(8.29915429043693,-48.2114340357053,16.8699103983795));
#49286=CARTESIAN_POINT('Ctrl Pts',(8.29915429043693,-32.5406722170424,-15.6707618186629));
#49287=CARTESIAN_POINT('Ctrl Pts',(7.4968190344241,-33.3770786491896,-16.0735539273924));
#49288=CARTESIAN_POINT('Ctrl Pts',(7.4968190344241,-17.3035247217972,-49.450632576582));
#49289=CARTESIAN_POINT('Ctrl Pts',(7.4968190344241,16.0735539273924,-33.3770786491896));
#49290=CARTESIAN_POINT('Ctrl Pts',(7.4968190344241,49.450632576582,-17.3035247217972));
#49291=CARTESIAN_POINT('Ctrl Pts',(7.4968190344241,33.3770786491896,16.0735539273924));
#49292=CARTESIAN_POINT('Ctrl Pts',(7.4968190344241,17.3035247217972,49.450632576582));
#49293=CARTESIAN_POINT('Ctrl Pts',(7.4968190344241,-16.0735539273924,33.3770786491896));
#49294=CARTESIAN_POINT('Ctrl Pts',(7.4968190344241,-49.450632576582,17.3035247217972));
#49295=CARTESIAN_POINT('Ctrl Pts',(7.4968190344241,-33.3770786491896,-16.0735539273924));
#49296=CARTESIAN_POINT('Ctrl Pts',(6.88220761950379,-34.0684169111937,-16.4064848873841));
#49297=CARTESIAN_POINT('Ctrl Pts',(6.88220761950379,-17.6619320238096,-50.4749017985778));
#49298=CARTESIAN_POINT('Ctrl Pts',(6.88220761950379,16.4064848873841,-34.0684169111937));
#49299=CARTESIAN_POINT('Ctrl Pts',(6.88220761950379,50.4749017985778,-17.6619320238096));
#49300=CARTESIAN_POINT('Ctrl Pts',(6.88220761950379,34.0684169111937,16.4064848873841));
#49301=CARTESIAN_POINT('Ctrl Pts',(6.88220761950379,17.6619320238096,50.4749017985778));
#49302=CARTESIAN_POINT('Ctrl Pts',(6.88220761950379,-16.4064848873841,34.0684169111937));
#49303=CARTESIAN_POINT('Ctrl Pts',(6.88220761950379,-50.4749017985778,17.6619320238096));
#49304=CARTESIAN_POINT('Ctrl Pts',(6.88220761950379,-34.0684169111937,-16.4064848873841));
#49305=CARTESIAN_POINT('Ctrl Pts',(6.43560997955544,-34.5986241433973,-16.6618192331215));
#49306=CARTESIAN_POINT('Ctrl Pts',(6.43560997955544,-17.9368049102758,-51.2604433765188));
#49307=CARTESIAN_POINT('Ctrl Pts',(6.43560997955544,16.6618192331215,-34.5986241433973));
#49308=CARTESIAN_POINT('Ctrl Pts',(6.43560997955544,51.2604433765188,-17.9368049102758));
#49309=CARTESIAN_POINT('Ctrl Pts',(6.43560997955544,34.5986241433973,16.6618192331215));
#49310=CARTESIAN_POINT('Ctrl Pts',(6.43560997955544,17.9368049102758,51.2604433765188));
#49311=CARTESIAN_POINT('Ctrl Pts',(6.43560997955544,-16.6618192331215,34.5986241433973));
#49312=CARTESIAN_POINT('Ctrl Pts',(6.43560997955544,-51.2604433765188,17.9368049102758));
#49313=CARTESIAN_POINT('Ctrl Pts',(6.43560997955544,-34.5986241433973,-16.6618192331215));
#49314=CARTESIAN_POINT('Ctrl Pts',(6.14415685965718,-34.9572124542593,-16.8345062622337));
#49315=CARTESIAN_POINT('Ctrl Pts',(6.14415685965718,-18.1227061920256,-51.791718716493));
#49316=CARTESIAN_POINT('Ctrl Pts',(6.14415685965718,16.8345062622337,-34.9572124542593));
#49317=CARTESIAN_POINT('Ctrl Pts',(6.14415685965718,51.791718716493,-18.1227061920256));
#49318=CARTESIAN_POINT('Ctrl Pts',(6.14415685965718,34.9572124542593,16.8345062622337));
#49319=CARTESIAN_POINT('Ctrl Pts',(6.14415685965718,18.1227061920256,51.791718716493));
#49320=CARTESIAN_POINT('Ctrl Pts',(6.14415685965718,-16.8345062622337,34.9572124542593));
#49321=CARTESIAN_POINT('Ctrl Pts',(6.14415685965718,-51.791718716493,18.1227061920256));
#49322=CARTESIAN_POINT('Ctrl Pts',(6.14415685965718,-34.9572124542593,-16.8345062622337));
#49323=CARTESIAN_POINT('Ctrl Pts',(6.,-35.1377858481943,-16.9214658255848));
#49324=CARTESIAN_POINT('Ctrl Pts',(6.,-18.2163200226096,-52.0592516737791));
#49325=CARTESIAN_POINT('Ctrl Pts',(6.,16.9214658255848,-35.1377858481943));
#49326=CARTESIAN_POINT('Ctrl Pts',(6.,52.0592516737791,-18.2163200226096));
#49327=CARTESIAN_POINT('Ctrl Pts',(6.,35.1377858481943,16.9214658255848));
#49328=CARTESIAN_POINT('Ctrl Pts',(6.,18.2163200226096,52.0592516737791));
#49329=CARTESIAN_POINT('Ctrl Pts',(6.,-16.9214658255848,35.1377858481943));
#49330=CARTESIAN_POINT('Ctrl Pts',(6.,-52.0592516737791,18.2163200226096));
#49331=CARTESIAN_POINT('Ctrl Pts',(6.,-35.1377858481943,-16.9214658255848));
#49332=CARTESIAN_POINT('Ctrl Pts',(15.,-24.1202348804503,-18.8301425727982));
#49333=CARTESIAN_POINT('Ctrl Pts',(14.0108432136945,-23.6906926400127,-20.3917630740682));
#49334=CARTESIAN_POINT('Ctrl Pts',(13.3692319443824,-23.3579535391276,-21.3915618529718));
#49335=CARTESIAN_POINT('Ctrl Pts',(12.3476991724842,-23.1473185206879,-22.7113896892958));
#49336=CARTESIAN_POINT('Ctrl Pts',(12.025018705019,-23.0807834000492,-23.1282952207817));
#49337=CARTESIAN_POINT('Ctrl Pts',(11.6666317570708,-23.0126114746088,-23.5919571633962));
#49338=CARTESIAN_POINT('Ctrl Pts',(11.3593868751763,-22.9704586633353,-23.9823118033932));
#49339=CARTESIAN_POINT('Ctrl Pts',(10.676771680913,-22.876806494815,-24.8495744466962));
#49340=CARTESIAN_POINT('Ctrl Pts',(10.1321636914396,-22.8734798744455,-25.510224320219));
#49341=CARTESIAN_POINT('Ctrl Pts',(9.56604173138329,-22.9954906247793,-26.139747689115));
#49342=CARTESIAN_POINT('Ctrl Pts',(9.34563078589189,-23.0429936484008,-26.3848430055616));
#49343=CARTESIAN_POINT('Ctrl Pts',(9.12222951098696,-23.1101461905759,-26.6250740206507));
#49344=CARTESIAN_POINT('Ctrl Pts',(8.88860711505281,-23.1970883230411,-26.8731231743128));
#49345=CARTESIAN_POINT('Ctrl Pts',(8.75830600700747,-23.2455796337767,-27.0114706963585));
#49346=CARTESIAN_POINT('Ctrl Pts',(8.62340343546558,-23.2985805913255,-27.1537906260844));
#49347=CARTESIAN_POINT('Ctrl Pts',(8.40819516300432,-23.3978248652992,-27.3800488166559));
#49348=CARTESIAN_POINT('Ctrl Pts',(8.02443006829141,-23.5747998847334,-27.7835184181781));
#49349=CARTESIAN_POINT('Ctrl Pts',(7.46417034513348,-23.8812360292217,-28.3671329236259));
#49350=CARTESIAN_POINT('Ctrl Pts',(6.85957019142019,-24.290054208171,-29.0329567468316));
#49351=CARTESIAN_POINT('Ctrl Pts',(6.58024553736739,-24.4789277896681,-29.3405666737144));
#49352=CARTESIAN_POINT('Ctrl Pts',(6.28976782192773,-24.7075513257838,-29.6525862691847));
#49353=CARTESIAN_POINT('Ctrl Pts',(6.,-24.9583551264995,-29.9679914138325));
#49354=CARTESIAN_POINT('Ctrl Pts',(2.09999999999999,-10.543135638033,-11.7771860002428));
#49355=CARTESIAN_POINT('Ctrl Pts',(2.73333333333333,-10.543135638033,-11.7771860002428));
#49356=CARTESIAN_POINT('Ctrl Pts',(3.36803272841208,-10.5431022073082,-11.7772201003177));
#49357=CARTESIAN_POINT('Ctrl Pts',(4.25276821260583,-10.5430810365691,-11.7772406600604));
#49358=CARTESIAN_POINT('Ctrl Pts',(4.7726650406829,-10.5368654902041,-11.7829280689769));
#49359=CARTESIAN_POINT('Ctrl Pts',(5.76856525243156,-10.5188745659,-11.7994589520322));
#49360=CARTESIAN_POINT('Ctrl Pts',(6.48507937940904,-10.5193931210859,-11.7990555387649));
#49361=CARTESIAN_POINT('Ctrl Pts',(6.99865688135792,-10.5442264472673,-11.7759801222031));
#49362=CARTESIAN_POINT('Ctrl Pts',(7.1247961420266,-10.5505968365102,-11.770213186573));
#49363=CARTESIAN_POINT('Ctrl Pts',(7.37169888445177,-10.564127314078,-11.7581967415648));
#49364=CARTESIAN_POINT('Ctrl Pts',(7.68210670520103,-10.5832981179727,-11.7415107170204));
#49365=CARTESIAN_POINT('Ctrl Pts',(8.05073427412801,-10.6102522860635,-11.7180831591284));
#49366=CARTESIAN_POINT('Ctrl Pts',(8.41503345999962,-10.641639777048,-11.6904177872868));
#49367=CARTESIAN_POINT('Ctrl Pts',(9.01074144008478,-10.7021842311636,-11.6357976675359));
#49368=CARTESIAN_POINT('Ctrl Pts',(9.4630915836405,-10.7645290505238,-11.5767471383662));
#49369=CARTESIAN_POINT('Ctrl Pts',(10.2678427399453,-10.9068861685958,-11.4344468552384));
#49370=CARTESIAN_POINT('Ctrl Pts',(10.9804879072974,-11.0906707746144,-11.2592289323592));
#49371=CARTESIAN_POINT('Ctrl Pts',(11.7910205592258,-11.3518074464669,-10.996769538782));
#49372=CARTESIAN_POINT('Ctrl Pts',(12.2471496193426,-11.5059150850389,-10.8342802498727));
#49373=CARTESIAN_POINT('Ctrl Pts',(12.4732460256849,-11.5832901851512,-10.7494488910709));
#49374=CARTESIAN_POINT('Ctrl Pts',(12.8351174828998,-11.7067525897982,-10.6107180331633));
#49375=CARTESIAN_POINT('Ctrl Pts',(13.2802512034868,-11.872521853359,-10.4216414569813));
#49376=CARTESIAN_POINT('Ctrl Pts',(14.1612564248657,-12.2443027142459,-9.98781870483396));
#49377=CARTESIAN_POINT('Ctrl Pts',(14.7820737708942,-12.5376840654805,-9.62062677307173));
#49378=CARTESIAN_POINT('Ctrl Pts',(15.1979896574214,-12.7275569106452,-9.35997935634041));
#49379=CARTESIAN_POINT('Ctrl Pts',(2.09999999999999,-15.3665400340489,-17.8255438053547));
#49380=CARTESIAN_POINT('Ctrl Pts',(2.73333333333333,-15.3665400340489,-17.8255438053547));
#49381=CARTESIAN_POINT('Ctrl Pts',(3.3687181809592,-15.3665376853649,-17.825543073398));
#49382=CARTESIAN_POINT('Ctrl Pts',(4.2541517406304,-15.3665263774122,-17.8255511225364));
#49383=CARTESIAN_POINT('Ctrl Pts',(4.78309364461817,-15.3570547633814,-17.8338945202897));
#49384=CARTESIAN_POINT('Ctrl Pts',(5.77493293929972,-15.3298480612272,-17.8579711392587));
#49385=CARTESIAN_POINT('Ctrl Pts',(6.47496215402976,-15.3309764425276,-17.8570616603784));
#49386=CARTESIAN_POINT('Ctrl Pts',(6.96726328871316,-15.3675608640459,-17.824319195921));
#49387=CARTESIAN_POINT('Ctrl Pts',(7.09308121852369,-15.377187236198,-17.8159278901612));
#49388=CARTESIAN_POINT('Ctrl Pts',(7.33628060567667,-15.3974710703976,-17.7985922469198));
#49389=CARTESIAN_POINT('Ctrl Pts',(7.64235593139221,-15.4262403669694,-17.7744996748306));
#49390=CARTESIAN_POINT('Ctrl Pts',(8.00391129102422,-15.4665370619219,-17.7408214399693));
#49391=CARTESIAN_POINT('Ctrl Pts',(8.36000437958409,-15.513400053435,-17.7010966390644));
#49392=CARTESIAN_POINT('Ctrl Pts',(8.9396712633142,-15.6034591512378,-17.6229736918479));
#49393=CARTESIAN_POINT('Ctrl Pts',(9.37528665277327,-15.6958982632444,-17.5387083063492));
#49394=CARTESIAN_POINT('Ctrl Pts',(10.1433938392068,-15.9053466146459,-17.3372073728695));
#49395=CARTESIAN_POINT('Ctrl Pts',(10.8342866476536,-16.1779457660886,-17.0879562123254));
#49396=CARTESIAN_POINT('Ctrl Pts',(11.6346749715978,-16.5710483980858,-16.7090772220389));
#49397=CARTESIAN_POINT('Ctrl Pts',(12.0872491273666,-16.8040533312314,-16.4733694239515));
#49398=CARTESIAN_POINT('Ctrl Pts',(12.3122412108241,-16.9213946705885,-16.3499117769089));
#49399=CARTESIAN_POINT('Ctrl Pts',(12.6725812427255,-17.1088177167675,-16.1477879438135));
#49400=CARTESIAN_POINT('Ctrl Pts',(13.1110124042394,-17.358752386583,-15.8749798027102));
#49401=CARTESIAN_POINT('Ctrl Pts',(13.9921319659501,-17.9251842036961,-15.2424196482269));
#49402=CARTESIAN_POINT('Ctrl Pts',(14.6125773377935,-18.3745300756618,-14.7038806929422));
#49403=CARTESIAN_POINT('Ctrl Pts',(15.0291266285127,-18.6654710972975,-14.3214960647507));
#49404=CARTESIAN_POINT('Ctrl Pts',(2.09999999999999,-20.1899444300649,-23.8739016104667));
#49405=CARTESIAN_POINT('Ctrl Pts',(2.73333333333333,-20.1899444300649,-23.8739016104667));
#49406=CARTESIAN_POINT('Ctrl Pts',(3.36945279028916,-20.1899202539663,-23.8739271559913));
#49407=CARTESIAN_POINT('Ctrl Pts',(4.2556151808724,-20.1898901685131,-23.873954635471));
#49408=CARTESIAN_POINT('Ctrl Pts',(4.79358405809382,-20.1769973476943,-23.8850954394867));
#49409=CARTESIAN_POINT('Ctrl Pts',(5.781457677744,-20.1406055273539,-23.9166958135384));
#49410=CARTESIAN_POINT('Ctrl Pts',(6.46486276385338,-20.1426565583293,-23.9150612533684));
#49411=CARTESIAN_POINT('Ctrl Pts',(6.93654238579164,-20.1893583815516,-23.8739698938311));
#49412=CARTESIAN_POINT('Ctrl Pts',(7.06205421776047,-20.2022104664193,-23.8629801928831));
#49413=CARTESIAN_POINT('Ctrl Pts',(7.30168521565929,-20.2289421717304,-23.8405729535745));
#49414=CARTESIAN_POINT('Ctrl Pts',(7.60366388861905,-20.2668688425343,-23.809441722807));
#49415=CARTESIAN_POINT('Ctrl Pts',(7.95860109522663,-20.3197565331949,-23.7661259375574));
#49416=CARTESIAN_POINT('Ctrl Pts',(8.30730975845261,-20.3809946218758,-23.7152635567132));
#49417=CARTESIAN_POINT('Ctrl Pts',(8.8731012800961,-20.4982979004896,-23.615516281743));
#49418=CARTESIAN_POINT('Ctrl Pts',(9.29618129829887,-20.6175188842592,-23.508902976663));
#49419=CARTESIAN_POINT('Ctrl Pts',(10.0462711259633,-20.8875329990534,-23.2540694624143));
#49420=CARTESIAN_POINT('Ctrl Pts',(10.7405155672895,-21.2491820582357,-22.9313257121034));
#49421=CARTESIAN_POINT('Ctrl Pts',(11.5482234021021,-21.7792041800607,-22.4320578933702));
#49422=CARTESIAN_POINT('Ctrl Pts',(12.0041785857202,-22.0933306986234,-22.121270230917));
#49423=CARTESIAN_POINT('Ctrl Pts',(12.2304118102814,-22.2514886727216,-21.9584788027488));
#49424=CARTESIAN_POINT('Ctrl Pts',(12.5924512492605,-22.5039758796212,-21.6920608765541));
#49425=CARTESIAN_POINT('Ctrl Pts',(13.0427785940057,-22.8464337698471,-21.3273673525245));
#49426=CARTESIAN_POINT('Ctrl Pts',(13.9385893244826,-23.6198877956831,-20.4820953239141));
#49427=CARTESIAN_POINT('Ctrl Pts',(14.5670688438605,-24.2303643403375,-19.7648571735367));
#49428=CARTESIAN_POINT('Ctrl Pts',(14.9853697475044,-24.6233676158593,-19.2582596049827));
#49429=CARTESIAN_POINT('Ctrl Pts',(2.09999999999999,-25.0133488260808,-29.9222594155786));
#49430=CARTESIAN_POINT('Ctrl Pts',(2.73333333333333,-25.0133488260808,-29.9222594155786));
#49431=CARTESIAN_POINT('Ctrl Pts',(3.3702033632722,-25.0133137772673,-29.9223022183699));
#49432=CARTESIAN_POINT('Ctrl Pts',(4.25711862532379,-25.0132696203947,-29.9223453341099));
#49433=CARTESIAN_POINT('Ctrl Pts',(4.80402085288096,-24.9968125168733,-29.9363970223899));
#49434=CARTESIAN_POINT('Ctrl Pts',(5.78813313564812,-24.951309348524,-29.9754629517883));
#49435=CARTESIAN_POINT('Ctrl Pts',(6.45445006013163,-24.9545928566979,-29.9728540151355));
#49436=CARTESIAN_POINT('Ctrl Pts',(6.90690581340697,-25.0101128882108,-29.9244532685749));
#49437=CARTESIAN_POINT('Ctrl Pts',(7.0321416409966,-25.0261697865242,-29.9108828348662));
#49438=CARTESIAN_POINT('Ctrl Pts',(7.26849200273963,-25.0591138242421,-29.8835944575659));
#49439=CARTESIAN_POINT('Ctrl Pts',(7.56683080333734,-25.1059083784109,-29.8456606556004));
#49440=CARTESIAN_POINT('Ctrl Pts',(7.91604722627538,-25.1709090389714,-29.7930989156434));
#49441=CARTESIAN_POINT('Ctrl Pts',(8.25884332748362,-25.2460113850425,-29.7315240189041));
#49442=CARTESIAN_POINT('Ctrl Pts',(8.8142690913405,-25.3898037321514,-29.61079095463));
#49443=CARTESIAN_POINT('Ctrl Pts',(9.23053436408081,-25.5358852579794,-29.4818139880829));
#49444=CARTESIAN_POINT('Ctrl Pts',(9.97649801930199,-25.8720992258963,-29.16894819951));
#49445=CARTESIAN_POINT('Ctrl Pts',(10.6790198772432,-26.3323429661403,-28.7642792997449));
#49446=CARTESIAN_POINT('Ctrl Pts',(11.4920869896606,-27.0039397656116,-28.1395712188247));
#49447=CARTESIAN_POINT('Ctrl Pts',(11.9504399507504,-27.4008484986125,-27.7516435052251));
#49448=CARTESIAN_POINT('Ctrl Pts',(12.1774700011005,-27.6002581978098,-27.5488212641388));
#49449=CARTESIAN_POINT('Ctrl Pts',(12.540670686897,-27.9183822175908,-27.2171066391423));
#49450=CARTESIAN_POINT('Ctrl Pts',(12.9976730423846,-28.3567980745589,-26.7563181574512));
#49451=CARTESIAN_POINT('Ctrl Pts',(13.8993991018205,-29.3371347665202,-25.6964971094244));
#49452=CARTESIAN_POINT('Ctrl Pts',(14.5324532885843,-30.1082433886537,-24.7996310338783));
#49453=CARTESIAN_POINT('Ctrl Pts',(14.9514110803021,-30.6026094817751,-24.1685815379353));
#49454=CARTESIAN_POINT('',(3.2,-24.1401481407882,-28.8273003894017));
#49455=CARTESIAN_POINT('Ctrl Pts',(3.2,-24.1401481407882,-28.8273003894017));
#49456=CARTESIAN_POINT('Ctrl Pts',(3.56152274835421,-23.4440063035266,-27.9543661360881));
#49457=CARTESIAN_POINT('Ctrl Pts',(3.95224584525397,-22.743573003028,-27.0667464745569));
#49458=CARTESIAN_POINT('Ctrl Pts',(4.787674301238,-21.3221368163265,-25.3199081516513));
#49459=CARTESIAN_POINT('Ctrl Pts',(5.2151394623216,-20.6296286000308,-24.4935406264987));
#49460=CARTESIAN_POINT('Ctrl Pts',(6.79548775402686,-18.2759304665965,-21.5959335780027));
#49461=CARTESIAN_POINT('Ctrl Pts',(7.94016295939582,-17.0442366760427,-19.7414374675915));
#49462=CARTESIAN_POINT('Ctrl Pts',(9.46271935276147,-15.5713230036123,-17.3844072806034));
#49463=CARTESIAN_POINT('Ctrl Pts',(10.1385443659149,-15.0481496226839,-16.3651968434456));
#49464=CARTESIAN_POINT('Ctrl Pts',(11.5967860400763,-14.1711568382327,-14.1885864925966));
#49465=CARTESIAN_POINT('Ctrl Pts',(12.3997356677094,-13.7376588526878,-13.0379046765038));
#49466=CARTESIAN_POINT('Ctrl Pts',(13.6850585208087,-13.1354996003446,-11.2495034212006));
#49467=CARTESIAN_POINT('Ctrl Pts',(14.3457395898605,-12.8831452960905,-10.3354978215121));
#49468=CARTESIAN_POINT('Ctrl Pts',(15.,-12.6367667846116,-9.48283298589492));
#49469=CARTESIAN_POINT('Ctrl Pts',(2.79814976461967,-24.7266470076605,-29.5627760094694));
#49470=CARTESIAN_POINT('Ctrl Pts',(2.93285977270366,-24.531202871586,-29.3177067107927));
#49471=CARTESIAN_POINT('Ctrl Pts',(3.06772729768953,-24.3356333359279,-29.0724818414568));
#49472=CARTESIAN_POINT('Ctrl Pts',(3.2025793347187,-24.1401219978448,-28.8273304373552));
#49473=CARTESIAN_POINT('Origin',(2.9,0.,0.));
#49474=CARTESIAN_POINT('',(3.2,-33.4762280926097,-17.1202264205697));
#49475=CARTESIAN_POINT('Origin',(3.2,0.,0.));
#49476=CARTESIAN_POINT('Ctrl Pts',(3.19855924658779,-33.4762497065829,-17.1201427543021));
#49477=CARTESIAN_POINT('Ctrl Pts',(3.06443679751087,-33.7588989525607,-17.2562771750589));
#49478=CARTESIAN_POINT('Ctrl Pts',(2.9303164767804,-34.0414969702962,-17.3923866976636));
#49479=CARTESIAN_POINT('Ctrl Pts',(2.79630592797694,-34.3237709021223,-17.5283375865302));
#49480=CARTESIAN_POINT('Ctrl Pts',(2.1,-15.7838176169527,-0.899999999999997));
#49481=CARTESIAN_POINT('Ctrl Pts',(2.73333333333333,-15.7838176169527,-0.899999999999997));
#49482=CARTESIAN_POINT('Ctrl Pts',(3.36596566980363,-15.7838088294802,-0.89991334692306));
#49483=CARTESIAN_POINT('Ctrl Pts',(4.12347559197154,-15.7838060309894,-0.899886769079504));
#49484=CARTESIAN_POINT('Ctrl Pts',(4.36306874504969,-15.7837152633585,-0.901834641161809));
#49485=CARTESIAN_POINT('Ctrl Pts',(4.85755348006649,-15.7833089582346,-0.910820654567172));
#49486=CARTESIAN_POINT('Ctrl Pts',(5.73897272285415,-15.7823612829529,-0.932201228099064));
#49487=CARTESIAN_POINT('Ctrl Pts',(6.52603489331944,-15.782348631485,-0.93280713780616));
#49488=CARTESIAN_POINT('Ctrl Pts',(7.1275435062192,-15.7839622361425,-0.893118870461858));
#49489=CARTESIAN_POINT('Ctrl Pts',(7.25503875736122,-15.7844067237825,-0.884431863337579));
#49490=CARTESIAN_POINT('Ctrl Pts',(7.51729728777054,-15.7855650629912,-0.865241085102853));
#49491=CARTESIAN_POINT('Ctrl Pts',(7.84586404221675,-15.7874367544175,-0.838250317529829));
#49492=CARTESIAN_POINT('Ctrl Pts',(8.24414264130042,-15.7901251990884,-0.799706719121714));
#49493=CARTESIAN_POINT('Ctrl Pts',(8.77644186211642,-15.7939497820795,-0.738435083081115));
#49494=CARTESIAN_POINT('Ctrl Pts',(9.44111162245666,-15.7985731396741,-0.640296638236062));
#49495=CARTESIAN_POINT('Ctrl Pts',(9.96386140770947,-15.8006687624932,-0.531294988793781));
#49496=CARTESIAN_POINT('Ctrl Pts',(11.1188881593647,-15.801839487482,-0.242371579936367));
#49497=CARTESIAN_POINT('Ctrl Pts',(12.080426103097,-15.8109272922644,0.160862502399577));
#49498=CARTESIAN_POINT('Ctrl Pts',(13.0008162933431,-15.7944409326678,0.612453502691948));
#49499=CARTESIAN_POINT('Ctrl Pts',(13.210793498058,-15.7890467971084,0.718001212690115));
#49500=CARTESIAN_POINT('Ctrl Pts',(13.3144168382157,-15.7859213877517,0.770572988426763));
#49501=CARTESIAN_POINT('Ctrl Pts',(13.3732968497844,-15.784008942705,0.800566234451453));
#49502=CARTESIAN_POINT('Ctrl Pts',(13.4025760150423,-15.7830115107287,0.815517600240429));
#49503=CARTESIAN_POINT('Ctrl Pts',(13.6877720326255,-15.7730387773425,0.961314730638964));
#49504=CARTESIAN_POINT('Ctrl Pts',(14.2465760997328,-15.7491595629163,1.27594900526736));
#49505=CARTESIAN_POINT('Ctrl Pts',(14.7537307590314,-15.7175740225323,1.606813173185));
#49506=CARTESIAN_POINT('Ctrl Pts',(14.9999999999997,-15.6990456112166,1.77537689056615));
#49507=CARTESIAN_POINT('Ctrl Pts',(2.1,-23.5191287709962,-0.899999999999997));
#49508=CARTESIAN_POINT('Ctrl Pts',(2.73333333333333,-23.5191287709962,-0.899999999999997));
#49509=CARTESIAN_POINT('Ctrl Pts',(3.3655781264468,-23.5191252884321,-0.899935556524944));
#49510=CARTESIAN_POINT('Ctrl Pts',(4.12267126809373,-23.5191242310313,-0.89991735126274));
#49511=CARTESIAN_POINT('Ctrl Pts',(4.35698403697962,-23.5190465734764,-0.902785708978077));
#49512=CARTESIAN_POINT('Ctrl Pts',(4.84798634051153,-23.5186994574573,-0.916113399717105));
#49513=CARTESIAN_POINT('Ctrl Pts',(5.73067052875929,-23.5178866627675,-0.948008744665266));
#49514=CARTESIAN_POINT('Ctrl Pts',(6.535923680173,-23.517885158871,-0.949379309188695));
#49515=CARTESIAN_POINT('Ctrl Pts',(7.15867348703883,-23.5192670336036,-0.888884811529982));
#49516=CARTESIAN_POINT('Ctrl Pts',(7.28649833326676,-23.5196879006994,-0.875917985293893));
#49517=CARTESIAN_POINT('Ctrl Pts',(7.55246203150236,-23.5208922670236,-0.847060977328295));
#49518=CARTESIAN_POINT('Ctrl Pts',(7.88538697752817,-23.5229509940679,-0.806514180409723));
#49519=CARTESIAN_POINT('Ctrl Pts',(8.29074120651406,-23.5259132916756,-0.748419508807197));
#49520=CARTESIAN_POINT('Ctrl Pts',(8.8340108396217,-23.5299680738502,-0.655942701497698));
#49521=CARTESIAN_POINT('Ctrl Pts',(9.51595482357549,-23.5342272010875,-0.507323297625138));
#49522=CARTESIAN_POINT('Ctrl Pts',(10.0562747286729,-23.5344392632137,-0.341535964232884));
#49523=CARTESIAN_POINT('Ctrl Pts',(11.2545001865845,-23.5284609002258,0.0994030366123566));
#49524=CARTESIAN_POINT('Ctrl Pts',(12.2341579615793,-23.5306916466498,0.708875196748114));
#49525=CARTESIAN_POINT('Ctrl Pts',(13.1607568713765,-23.4927543604707,1.38402604346733));
#49526=CARTESIAN_POINT('Ctrl Pts',(13.3718579954519,-23.4815829003965,1.54166599939733));
#49527=CARTESIAN_POINT('Ctrl Pts',(13.4759064249217,-23.4753563425579,1.62011007351799));
#49528=CARTESIAN_POINT('Ctrl Pts',(13.5350103301451,-23.4716106415352,1.66485146824944));
#49529=CARTESIAN_POINT('Ctrl Pts',(13.5643801112264,-23.4696762113674,1.68714788583071));
#49530=CARTESIAN_POINT('Ctrl Pts',(13.8508752065214,-23.4504857575959,1.9045506874055));
#49531=CARTESIAN_POINT('Ctrl Pts',(14.4158963288387,-23.4057058787818,2.37675373622547));
#49532=CARTESIAN_POINT('Ctrl Pts',(14.9236315787721,-23.34905257923,2.86887715082168));
#49533=CARTESIAN_POINT('Ctrl Pts',(15.169681381964,-23.3165272641956,3.11946875835517));
#49534=CARTESIAN_POINT('Ctrl Pts',(2.1,-31.2544399250396,-0.899999999999996));
#49535=CARTESIAN_POINT('Ctrl Pts',(2.73333333333333,-31.2544399250396,-0.899999999999996));
#49536=CARTESIAN_POINT('Ctrl Pts',(3.36510803949126,-31.2544285975785,-0.899887954579111));
#49537=CARTESIAN_POINT('Ctrl Pts',(4.1217599483887,-31.2544250687149,-0.899856461790129));
#49538=CARTESIAN_POINT('Ctrl Pts',(4.35078018391394,-31.2543593971872,-0.903581998407283));
#49539=CARTESIAN_POINT('Ctrl Pts',(4.83831486811687,-31.2540689041506,-0.921123484582133));
#49540=CARTESIAN_POINT('Ctrl Pts',(5.72215239235997,-31.2533869648983,-0.963543461248137));
#49541=CARTESIAN_POINT('Ctrl Pts',(6.54569204847154,-31.253375981803,-0.966087209027176));
#49542=CARTESIAN_POINT('Ctrl Pts',(7.18900601609011,-31.2545146303357,-0.882690915352525));
#49543=CARTESIAN_POINT('Ctrl Pts',(7.31714403897362,-31.2549105346497,-0.865405180349154));
#49544=CARTESIAN_POINT('Ctrl Pts',(7.58667564997587,-31.2561576889986,-0.826487518155644));
#49545=CARTESIAN_POINT('Ctrl Pts',(7.92370562146597,-31.2583919516221,-0.771819144977552));
#49546=CARTESIAN_POINT('Ctrl Pts',(8.33567742441321,-31.2616158481274,-0.693189967012442));
#49547=CARTESIAN_POINT('Ctrl Pts',(8.88879010852856,-31.265860135187,-0.567641912212619));
#49548=CARTESIAN_POINT('Ctrl Pts',(9.58533914692519,-31.2696691847387,-0.365023033156311));
#49549=CARTESIAN_POINT('Ctrl Pts',(10.1375264374995,-31.2678183104491,-0.137996175847509));
#49550=CARTESIAN_POINT('Ctrl Pts',(11.3565030519649,-31.2540818885826,0.465220229785789));
#49551=CARTESIAN_POINT('Ctrl Pts',(12.3227872766541,-31.2488724320959,1.27591572087597));
#49552=CARTESIAN_POINT('Ctrl Pts',(13.2438100919778,-31.1896995065743,2.16862824846055));
#49553=CARTESIAN_POINT('Ctrl Pts',(13.4536570645148,-31.1727762889572,2.37732774887136));
#49554=CARTESIAN_POINT('Ctrl Pts',(13.5572209116411,-31.1634652599129,2.4811657802529));
#49555=CARTESIAN_POINT('Ctrl Pts',(13.6160603594674,-31.1578938077571,2.54040820945414));
#49556=CARTESIAN_POINT('Ctrl Pts',(13.6453174194113,-31.1550264688678,2.56993362549346));
#49557=CARTESIAN_POINT('Ctrl Pts',(13.9304114081194,-31.1266303388415,2.85783766366555));
#49558=CARTESIAN_POINT('Ctrl Pts',(14.4834636188671,-31.0622526519641,3.47544368375122));
#49559=CARTESIAN_POINT('Ctrl Pts',(14.98335392639,-30.9820977609996,4.11984152156402));
#49560=CARTESIAN_POINT('Ctrl Pts',(15.2260186760796,-30.9364949201562,4.44811307850482));
#49561=CARTESIAN_POINT('Ctrl Pts',(2.1,-38.9897510790831,-0.899999999999995));
#49562=CARTESIAN_POINT('Ctrl Pts',(2.73333333333333,-38.9897510790831,-0.899999999999995));
#49563=CARTESIAN_POINT('Ctrl Pts',(3.36462990527675,-38.9897323635969,-0.899873465153036));
#49564=CARTESIAN_POINT('Ctrl Pts',(4.1208427270016,-38.9897265328331,-0.899838966037325));
#49565=CARTESIAN_POINT('Ctrl Pts',(4.34455772832346,-38.9896728108089,-0.904370340701259));
#49566=CARTESIAN_POINT('Ctrl Pts',(4.82869886846261,-38.9894393624541,-0.926010025459942));
#49567=CARTESIAN_POINT('Ctrl Pts',(5.71348591011319,-38.9888878390437,-0.979037562584771));
#49568=CARTESIAN_POINT('Ctrl Pts',(6.55581603709115,-38.988869624559,-0.983187703385992));
#49569=CARTESIAN_POINT('Ctrl Pts',(7.21830359959701,-38.9897625234554,-0.875238407743373));
#49570=CARTESIAN_POINT('Ctrl Pts',(7.3467255268605,-38.990132712043,-0.853607279018514));
#49571=CARTESIAN_POINT('Ctrl Pts',(7.61953681834974,-38.991420569913,-0.804326922325396));
#49572=CARTESIAN_POINT('Ctrl Pts',(7.96022442918569,-38.9938266042631,-0.735174920601364));
#49573=CARTESIAN_POINT('Ctrl Pts',(8.37790664744398,-38.9973035670093,-0.635391241461812));
#49574=CARTESIAN_POINT('Ctrl Pts',(8.93894152673479,-39.0017204784551,-0.475916526516923));
#49575=CARTESIAN_POINT('Ctrl Pts',(9.6458573751342,-39.0050422513425,-0.218333539006556));
#49576=CARTESIAN_POINT('Ctrl Pts',(10.2035440776973,-39.001117677713,0.0687868979514879));
#49577=CARTESIAN_POINT('Ctrl Pts',(11.4269391757474,-38.9798103474589,0.825175481853652));
#49578=CARTESIAN_POINT('Ctrl Pts',(12.379427420675,-38.968220494253,1.82168627873895));
#49579=CARTESIAN_POINT('Ctrl Pts',(13.2972499365664,-38.8888984651817,2.92824372486156));
#49580=CARTESIAN_POINT('Ctrl Pts',(13.5062198971924,-38.8664635788881,3.18711889465918));
#49581=CARTESIAN_POINT('Ctrl Pts',(13.6094926661745,-38.8541842965825,3.31604931695643));
#49582=CARTESIAN_POINT('Ctrl Pts',(13.6681658325864,-38.8468524163685,3.38962535504308));
#49583=CARTESIAN_POINT('Ctrl Pts',(13.6973582444968,-38.8430838348503,3.42631180642128));
#49584=CARTESIAN_POINT('Ctrl Pts',(13.981458935376,-38.8058099556096,3.78381873659936));
#49585=CARTESIAN_POINT('Ctrl Pts',(14.5280821792823,-38.7229860114931,4.5416971141935));
#49586=CARTESIAN_POINT('Ctrl Pts',(15.0243070371674,-38.6201388341544,5.33756918640965));
#49587=CARTESIAN_POINT('Ctrl Pts',(15.2656150130537,-38.5618298130439,5.74340641366416));
#49588=CARTESIAN_POINT('',(3.2,-37.5892271801377,-0.900000000000009));
#49589=CARTESIAN_POINT('Ctrl Pts',(3.19846504060563,-37.5892155742874,-0.899918216107268));
#49590=CARTESIAN_POINT('Ctrl Pts',(3.06435898455936,-37.9029407045989,-0.899932532575135));
#49591=CARTESIAN_POINT('Ctrl Pts',(2.93025577717209,-38.216607400202,-0.899947286012378));
#49592=CARTESIAN_POINT('Ctrl Pts',(2.79626085549373,-38.5299117979594,-0.89996027252497));
#49593=CARTESIAN_POINT('',(15.,-15.6990456112299,1.77537689056849));
#49594=CARTESIAN_POINT('Ctrl Pts',(15.,-15.6990456112299,1.77537689056849));
#49595=CARTESIAN_POINT('Ctrl Pts',(14.4897165779516,-16.2849589337065,1.51421724761149));
#49596=CARTESIAN_POINT('Ctrl Pts',(13.9833803026614,-16.8928254585971,1.26139925814643));
#49597=CARTESIAN_POINT('Ctrl Pts',(13.4460287676664,-17.5732796520164,1.02322986490673));
#49598=CARTESIAN_POINT('Ctrl Pts',(12.828265568108,-18.355560025857,0.749419748395156));
#49599=CARTESIAN_POINT('Ctrl Pts',(12.155541408957,-19.2651912004079,0.431967913798082));
#49600=CARTESIAN_POINT('Ctrl Pts',(11.5904908073729,-20.0758271479682,0.194165150923072));
#49601=CARTESIAN_POINT('Ctrl Pts',(11.1143368259691,-20.7589297458909,-0.00622527785325226));
#49602=CARTESIAN_POINT('Ctrl Pts',(10.6953158949622,-21.3919930406842,-0.162474098896682));
#49603=CARTESIAN_POINT('Ctrl Pts',(10.2957959918397,-22.0215958519058,-0.285400301904625));
#49604=CARTESIAN_POINT('Ctrl Pts',(10.0450888109335,-22.4166849192045,-0.362539091673938));
#49605=CARTESIAN_POINT('Ctrl Pts',(9.80235305580163,-22.8103758783969,-0.427399680658795));
#49606=CARTESIAN_POINT('Ctrl Pts',(9.56010106231365,-23.2148468084221,-0.485388811488509));
#49607=CARTESIAN_POINT('Ctrl Pts',(9.36613602937194,-23.5386964335034,-0.531819239200157));
#49608=CARTESIAN_POINT('Ctrl Pts',(9.15248571290285,-23.9017725603612,-0.578857851041087));
#49609=CARTESIAN_POINT('Ctrl Pts',(8.89022359818963,-24.3643567925319,-0.629224074447282));
#49610=CARTESIAN_POINT('Ctrl Pts',(8.39222406101306,-25.2427403660727,-0.724862577069152));
#49611=CARTESIAN_POINT('Ctrl Pts',(7.76643777371613,-26.4044500016645,-0.817180074306374));
#49612=CARTESIAN_POINT('Ctrl Pts',(7.10363554123529,-27.7707039763826,-0.894013240725695));
#49613=CARTESIAN_POINT('Ctrl Pts',(6.23550018249052,-29.5602172374331,-0.994648973713817));
#49614=CARTESIAN_POINT('Ctrl Pts',(5.31040885823351,-31.7028345140282,-0.937721664108877));
#49615=CARTESIAN_POINT('Ctrl Pts',(4.46416616905172,-33.9628693235812,-0.909003245197519));
#49616=CARTESIAN_POINT('Ctrl Pts',(4.30741751125037,-34.3814932331411,-0.903683762174411));
#49617=CARTESIAN_POINT('Ctrl Pts',(4.15262292089316,-34.8053728589431,-0.899999999999994));
#49618=CARTESIAN_POINT('Ctrl Pts',(4.,-35.2340925362767,-0.899999999999994));
#49619=CARTESIAN_POINT('Ctrl Pts',(3.72434973283394,-36.0083975548465,-0.899999999999995));
#49620=CARTESIAN_POINT('Ctrl Pts',(3.45587123478811,-36.7989959013664,-0.899999999999995));
#49621=CARTESIAN_POINT('Ctrl Pts',(3.2,-37.5892271801377,-0.899999999999995));
#49622=CARTESIAN_POINT('',(15.,-30.3301605390585,4.05479489924437));
#49623=CARTESIAN_POINT('Ctrl Pts',(15.,-30.3301605390585,4.05479489924437));
#49624=CARTESIAN_POINT('Ctrl Pts',(15.,-25.9658737968045,3.39120490592858));
#49625=CARTESIAN_POINT('Ctrl Pts',(15.,-20.7866378565132,2.59413270773475));
#49626=CARTESIAN_POINT('Ctrl Pts',(15.,-15.6990456112299,1.77537689056849));
#49627=CARTESIAN_POINT('Ctrl Pts',(6.,-38.9878978038234,-0.97150647893904));
#49628=CARTESIAN_POINT('Ctrl Pts',(6.38595465246567,-38.4511580946401,-0.970712640298574));
#49629=CARTESIAN_POINT('Ctrl Pts',(6.77023648668261,-37.9485848088862,-0.946911108705782));
#49630=CARTESIAN_POINT('Ctrl Pts',(7.13915213286207,-37.4906963516412,-0.889177532284711));
#49631=CARTESIAN_POINT('Ctrl Pts',(8.10667920093238,-36.2898270441738,-0.737764062830719));
#49632=CARTESIAN_POINT('Ctrl Pts',(8.98019888747373,-35.389539750921,-0.506506391035769));
#49633=CARTESIAN_POINT('Ctrl Pts',(9.46656009721079,-34.9110454673415,-0.333331441085477));
#49634=CARTESIAN_POINT('Ctrl Pts',(9.65648624874915,-34.7241913844214,-0.265705875706425));
#49635=CARTESIAN_POINT('Ctrl Pts',(9.79228848853734,-34.5946295139584,-0.211763607435485));
#49636=CARTESIAN_POINT('Ctrl Pts',(9.94593825727822,-34.4503982837665,-0.146089247346362));
#49637=CARTESIAN_POINT('Ctrl Pts',(10.1065740866009,-34.2996092297643,-0.0774288426831876));
#49638=CARTESIAN_POINT('Ctrl Pts',(10.2660951669675,-34.1533235936857,-0.00297951038240219));
#49639=CARTESIAN_POINT('Ctrl Pts',(10.4261869573617,-34.0095357957359,0.0794327468215139));
#49640=CARTESIAN_POINT('Ctrl Pts',(10.8065549509411,-33.6679050595643,0.275239070442707));
#49641=CARTESIAN_POINT('Ctrl Pts',(11.1894211925257,-33.3406313554732,0.517069342042946));
#49642=CARTESIAN_POINT('Ctrl Pts',(11.6023503255242,-33.0003063200243,0.822996043177648));
#49643=CARTESIAN_POINT('Ctrl Pts',(11.7531893954247,-32.8759888337811,0.934748146309273));
#49644=CARTESIAN_POINT('Ctrl Pts',(11.9080270687775,-32.7499870988422,1.05519161239494));
#49645=CARTESIAN_POINT('Ctrl Pts',(12.0681766131679,-32.621092353582,1.18544337126706));
#49646=CARTESIAN_POINT('Ctrl Pts',(12.1838435903475,-32.5279989538141,1.27951686537783));
#49647=CARTESIAN_POINT('Ctrl Pts',(12.3100865410161,-32.4268183073742,1.38378769072677));
#49648=CARTESIAN_POINT('Ctrl Pts',(12.5127093730713,-32.2665490637521,1.56015391817218));
#49649=CARTESIAN_POINT('Ctrl Pts',(12.7975492664043,-32.041248322494,1.80808322062817));
#49650=CARTESIAN_POINT('Ctrl Pts',(13.1874566943567,-31.7365390294451,2.16619278329376));
#49651=CARTESIAN_POINT('Ctrl Pts',(13.6431584568239,-31.3858069581634,2.5980913893376));
#49652=CARTESIAN_POINT('Ctrl Pts',(14.069523646534,-31.057653857987,3.00218579113323));
#49653=CARTESIAN_POINT('Ctrl Pts',(14.53311408767,-30.7006478334489,3.5004679889341));
#49654=CARTESIAN_POINT('Ctrl Pts',(15.,-30.3301605390585,4.05479489924437));
#49655=CARTESIAN_POINT('Origin',(15.,-7.65823537717056,3.68801178249925));
#49656=CARTESIAN_POINT('',(15.,-15.2928725900315,3.96737244938058));
#49657=CARTESIAN_POINT('Ctrl Pts',(15.,-15.2928725900315,3.96737244938057));
#49658=CARTESIAN_POINT('Ctrl Pts',(15.,-15.3032674728402,3.92730370856767));
#49659=CARTESIAN_POINT('Ctrl Pts',(15.,-15.3135058702623,3.88719029713218));
#49660=CARTESIAN_POINT('Ctrl Pts',(15.,-15.4950281428345,3.16414676313573));
#49661=CARTESIAN_POINT('Ctrl Pts',(15.,-15.62026181147,2.47203486354725));
#49662=CARTESIAN_POINT('Ctrl Pts',(15.,-15.6990456112299,1.77537689056849));
#49663=CARTESIAN_POINT('',(15.,-29.7607187491733,7.11755713237394));
#49664=CARTESIAN_POINT('Ctrl Pts',(15.,-15.2928725900315,3.96737244938059));
#49665=CARTESIAN_POINT('Ctrl Pts',(15.,-20.4763230842092,5.06462647823764));
#49666=CARTESIAN_POINT('Ctrl Pts',(15.,-25.6935126383795,6.2146953165994));
#49667=CARTESIAN_POINT('Ctrl Pts',(15.,-29.7607187491733,7.11755713237393));
#49668=CARTESIAN_POINT('Origin',(15.,0.,0.));
#49669=CARTESIAN_POINT('Ctrl Pts',(15.,-27.569647357814,13.2768424169973));
#49670=CARTESIAN_POINT('Ctrl Pts',(15.,-40.8464897748113,-14.2928049408167));
#49671=CARTESIAN_POINT('Ctrl Pts',(15.,-13.2768424169973,-27.569647357814));
#49672=CARTESIAN_POINT('Ctrl Pts',(15.,14.2928049408167,-40.8464897748113));
#49673=CARTESIAN_POINT('Ctrl Pts',(15.,27.569647357814,-13.2768424169973));
#49674=CARTESIAN_POINT('Ctrl Pts',(15.,40.8464897748113,14.2928049408167));
#49675=CARTESIAN_POINT('Ctrl Pts',(15.,13.2768424169973,27.569647357814));
#49676=CARTESIAN_POINT('Ctrl Pts',(15.,-14.2928049408167,40.8464897748113));
#49677=CARTESIAN_POINT('Ctrl Pts',(15.,-27.569647357814,13.2768424169973));
#49678=CARTESIAN_POINT('Ctrl Pts',(14.7843073131059,-27.6919221166174,13.3357268373578));
#49679=CARTESIAN_POINT('Ctrl Pts',(14.7843073131059,-41.0276489539752,-14.3561952792596));
#49680=CARTESIAN_POINT('Ctrl Pts',(14.7843073131059,-13.3357268373578,-27.6919221166174));
#49681=CARTESIAN_POINT('Ctrl Pts',(14.7843073131059,14.3561952792596,-41.0276489539752));
#49682=CARTESIAN_POINT('Ctrl Pts',(14.7843073131059,27.6919221166174,-13.3357268373578));
#49683=CARTESIAN_POINT('Ctrl Pts',(14.7843073131059,41.0276489539752,14.3561952792596));
#49684=CARTESIAN_POINT('Ctrl Pts',(14.7843073131059,13.3357268373578,27.6919221166174));
#49685=CARTESIAN_POINT('Ctrl Pts',(14.7843073131059,-14.3561952792596,41.0276489539752));
#49686=CARTESIAN_POINT('Ctrl Pts',(14.7843073131059,-27.6919221166174,13.3357268373578));
#49687=CARTESIAN_POINT('Ctrl Pts',(14.3560298066371,-27.9390044129707,13.4547154000382));
#49688=CARTESIAN_POINT('Ctrl Pts',(14.3560298066371,-41.3937198130089,-14.4842890129324));
#49689=CARTESIAN_POINT('Ctrl Pts',(14.3560298066371,-13.4547154000382,-27.9390044129707));
#49690=CARTESIAN_POINT('Ctrl Pts',(14.3560298066371,14.4842890129324,-41.3937198130089));
#49691=CARTESIAN_POINT('Ctrl Pts',(14.3560298066371,27.9390044129707,-13.4547154000382));
#49692=CARTESIAN_POINT('Ctrl Pts',(14.3560298066371,41.3937198130089,14.4842890129324));
#49693=CARTESIAN_POINT('Ctrl Pts',(14.3560298066371,13.4547154000382,27.9390044129707));
#49694=CARTESIAN_POINT('Ctrl Pts',(14.3560298066371,-14.4842890129324,41.3937198130089));
#49695=CARTESIAN_POINT('Ctrl Pts',(14.3560298066371,-27.9390044129707,13.4547154000382));
#49696=CARTESIAN_POINT('Ctrl Pts',(13.722936818686,-28.3172259246361,13.6368572803433));
#49697=CARTESIAN_POINT('Ctrl Pts',(13.722936818686,-41.9540832049794,-14.6803686442928));
#49698=CARTESIAN_POINT('Ctrl Pts',(13.722936818686,-13.6368572803433,-28.3172259246361));
#49699=CARTESIAN_POINT('Ctrl Pts',(13.722936818686,14.6803686442928,-41.9540832049794));
#49700=CARTESIAN_POINT('Ctrl Pts',(13.722936818686,28.3172259246361,-13.6368572803433));
#49701=CARTESIAN_POINT('Ctrl Pts',(13.722936818686,41.9540832049794,14.6803686442928));
#49702=CARTESIAN_POINT('Ctrl Pts',(13.722936818686,13.6368572803433,28.3172259246361));
#49703=CARTESIAN_POINT('Ctrl Pts',(13.722936818686,-14.6803686442928,41.9540832049794));
#49704=CARTESIAN_POINT('Ctrl Pts',(13.722936818686,-28.3172259246361,13.6368572803433));
#49705=CARTESIAN_POINT('Ctrl Pts',(12.8977690042853,-28.8369697397467,13.8871527099828));
#49706=CARTESIAN_POINT('Ctrl Pts',(12.8977690042853,-42.7241224497295,-14.9498170297639));
#49707=CARTESIAN_POINT('Ctrl Pts',(12.8977690042853,-13.8871527099828,-28.8369697397467));
#49708=CARTESIAN_POINT('Ctrl Pts',(12.8977690042853,14.9498170297639,-42.7241224497295));
#49709=CARTESIAN_POINT('Ctrl Pts',(12.8977690042853,28.8369697397467,-13.8871527099828));
#49710=CARTESIAN_POINT('Ctrl Pts',(12.8977690042853,42.7241224497295,14.9498170297639));
#49711=CARTESIAN_POINT('Ctrl Pts',(12.8977690042853,13.8871527099828,28.8369697397467));
#49712=CARTESIAN_POINT('Ctrl Pts',(12.8977690042853,-14.9498170297639,42.7241224497295));
#49713=CARTESIAN_POINT('Ctrl Pts',(12.8977690042853,-28.8369697397467,13.8871527099828));
#49714=CARTESIAN_POINT('Ctrl Pts',(11.9000549946031,-29.5141508562392,14.2132659480213));
#49715=CARTESIAN_POINT('Ctrl Pts',(11.9000549946031,-43.7274168042605,-15.3008849082179));
#49716=CARTESIAN_POINT('Ctrl Pts',(11.9000549946031,-14.2132659480213,-29.5141508562392));
#49717=CARTESIAN_POINT('Ctrl Pts',(11.9000549946031,15.3008849082179,-43.7274168042605));
#49718=CARTESIAN_POINT('Ctrl Pts',(11.9000549946031,29.5141508562392,-14.2132659480213));
#49719=CARTESIAN_POINT('Ctrl Pts',(11.9000549946031,43.7274168042605,15.3008849082179));
#49720=CARTESIAN_POINT('Ctrl Pts',(11.9000549946031,14.2132659480213,29.5141508562392));
#49721=CARTESIAN_POINT('Ctrl Pts',(11.9000549946031,-15.3008849082179,43.7274168042605));
#49722=CARTESIAN_POINT('Ctrl Pts',(11.9000549946031,-29.5141508562392,14.2132659480213));
#49723=CARTESIAN_POINT('Ctrl Pts',(10.9391333834985,-30.2213162016529,14.5538188296728));
#49724=CARTESIAN_POINT('Ctrl Pts',(10.9391333834985,-44.7751350313257,-15.6674973719801));
#49725=CARTESIAN_POINT('Ctrl Pts',(10.9391333834985,-14.5538188296728,-30.2213162016529));
#49726=CARTESIAN_POINT('Ctrl Pts',(10.9391333834985,15.6674973719801,-44.7751350313257));
#49727=CARTESIAN_POINT('Ctrl Pts',(10.9391333834985,30.2213162016529,-14.5538188296728));
#49728=CARTESIAN_POINT('Ctrl Pts',(10.9391333834985,44.7751350313257,15.6674973719801));
#49729=CARTESIAN_POINT('Ctrl Pts',(10.9391333834985,14.5538188296728,30.2213162016529));
#49730=CARTESIAN_POINT('Ctrl Pts',(10.9391333834985,-15.6674973719801,44.7751350313257));
#49731=CARTESIAN_POINT('Ctrl Pts',(10.9391333834985,-30.2213162016529,14.5538188296728));
#49732=CARTESIAN_POINT('Ctrl Pts',(10.0180552497783,-30.9609522745316,14.9100087895256));
#49733=CARTESIAN_POINT('Ctrl Pts',(10.0180552497783,-45.8709610640572,-16.0509434850059));
#49734=CARTESIAN_POINT('Ctrl Pts',(10.0180552497783,-14.9100087895256,-30.9609522745316));
#49735=CARTESIAN_POINT('Ctrl Pts',(10.0180552497783,16.0509434850059,-45.8709610640572));
#49736=CARTESIAN_POINT('Ctrl Pts',(10.0180552497783,30.9609522745316,-14.9100087895256));
#49737=CARTESIAN_POINT('Ctrl Pts',(10.0180552497783,45.8709610640572,16.0509434850059));
#49738=CARTESIAN_POINT('Ctrl Pts',(10.0180552497783,14.9100087895256,30.9609522745316));
#49739=CARTESIAN_POINT('Ctrl Pts',(10.0180552497783,-16.0509434850059,45.8709610640572));
#49740=CARTESIAN_POINT('Ctrl Pts',(10.0180552497783,-30.9609522745316,14.9100087895256));
#49741=CARTESIAN_POINT('Ctrl Pts',(9.13857394886632,-31.734487984447,15.2825239541622));
#49742=CARTESIAN_POINT('Ctrl Pts',(9.13857394886632,-47.0170119386091,-16.4519640302848));
#49743=CARTESIAN_POINT('Ctrl Pts',(9.13857394886632,-15.2825239541622,-31.734487984447));
#49744=CARTESIAN_POINT('Ctrl Pts',(9.13857394886632,16.4519640302848,-47.0170119386091));
#49745=CARTESIAN_POINT('Ctrl Pts',(9.13857394886632,31.734487984447,-15.2825239541622));
#49746=CARTESIAN_POINT('Ctrl Pts',(9.13857394886632,47.0170119386091,16.4519640302848));
#49747=CARTESIAN_POINT('Ctrl Pts',(9.13857394886632,15.2825239541622,31.734487984447));
#49748=CARTESIAN_POINT('Ctrl Pts',(9.13857394886632,-16.4519640302848,47.0170119386091));
#49749=CARTESIAN_POINT('Ctrl Pts',(9.13857394886632,-31.734487984447,15.2825239541622));
#49750=CARTESIAN_POINT('Ctrl Pts',(8.29915429043693,-32.5406722170424,15.6707618186629));
#49751=CARTESIAN_POINT('Ctrl Pts',(8.29915429043693,-48.2114340357053,-16.8699103983794));
#49752=CARTESIAN_POINT('Ctrl Pts',(8.29915429043693,-15.6707618186629,-32.5406722170424));
#49753=CARTESIAN_POINT('Ctrl Pts',(8.29915429043693,16.8699103983794,-48.2114340357053));
#49754=CARTESIAN_POINT('Ctrl Pts',(8.29915429043693,32.5406722170424,-15.6707618186629));
#49755=CARTESIAN_POINT('Ctrl Pts',(8.29915429043693,48.2114340357053,16.8699103983794));
#49756=CARTESIAN_POINT('Ctrl Pts',(8.29915429043693,15.6707618186629,32.5406722170424));
#49757=CARTESIAN_POINT('Ctrl Pts',(8.29915429043693,-16.8699103983794,48.2114340357053));
#49758=CARTESIAN_POINT('Ctrl Pts',(8.29915429043693,-32.5406722170424,15.6707618186629));
#49759=CARTESIAN_POINT('Ctrl Pts',(7.4968190344241,-33.3770786491896,16.0735539273924));
#49760=CARTESIAN_POINT('Ctrl Pts',(7.4968190344241,-49.450632576582,-17.3035247217972));
#49761=CARTESIAN_POINT('Ctrl Pts',(7.4968190344241,-16.0735539273924,-33.3770786491896));
#49762=CARTESIAN_POINT('Ctrl Pts',(7.4968190344241,17.3035247217972,-49.450632576582));
#49763=CARTESIAN_POINT('Ctrl Pts',(7.4968190344241,33.3770786491896,-16.0735539273924));
#49764=CARTESIAN_POINT('Ctrl Pts',(7.4968190344241,49.450632576582,17.3035247217972));
#49765=CARTESIAN_POINT('Ctrl Pts',(7.4968190344241,16.0735539273924,33.3770786491896));
#49766=CARTESIAN_POINT('Ctrl Pts',(7.4968190344241,-17.3035247217972,49.450632576582));
#49767=CARTESIAN_POINT('Ctrl Pts',(7.4968190344241,-33.3770786491896,16.0735539273924));
#49768=CARTESIAN_POINT('Ctrl Pts',(6.88220761950379,-34.0684169111937,16.4064848873841));
#49769=CARTESIAN_POINT('Ctrl Pts',(6.88220761950379,-50.4749017985778,-17.6619320238096));
#49770=CARTESIAN_POINT('Ctrl Pts',(6.88220761950379,-16.4064848873841,-34.0684169111937));
#49771=CARTESIAN_POINT('Ctrl Pts',(6.88220761950379,17.6619320238096,-50.4749017985778));
#49772=CARTESIAN_POINT('Ctrl Pts',(6.88220761950379,34.0684169111937,-16.4064848873841));
#49773=CARTESIAN_POINT('Ctrl Pts',(6.88220761950379,50.4749017985778,17.6619320238096));
#49774=CARTESIAN_POINT('Ctrl Pts',(6.88220761950379,16.4064848873841,34.0684169111937));
#49775=CARTESIAN_POINT('Ctrl Pts',(6.88220761950379,-17.6619320238096,50.4749017985778));
#49776=CARTESIAN_POINT('Ctrl Pts',(6.88220761950379,-34.0684169111937,16.4064848873841));
#49777=CARTESIAN_POINT('Ctrl Pts',(6.43560997955544,-34.5986241433973,16.6618192331215));
#49778=CARTESIAN_POINT('Ctrl Pts',(6.43560997955544,-51.2604433765188,-17.9368049102758));
#49779=CARTESIAN_POINT('Ctrl Pts',(6.43560997955544,-16.6618192331215,-34.5986241433973));
#49780=CARTESIAN_POINT('Ctrl Pts',(6.43560997955544,17.9368049102758,-51.2604433765188));
#49781=CARTESIAN_POINT('Ctrl Pts',(6.43560997955544,34.5986241433973,-16.6618192331215));
#49782=CARTESIAN_POINT('Ctrl Pts',(6.43560997955544,51.2604433765188,17.9368049102758));
#49783=CARTESIAN_POINT('Ctrl Pts',(6.43560997955544,16.6618192331215,34.5986241433973));
#49784=CARTESIAN_POINT('Ctrl Pts',(6.43560997955544,-17.9368049102758,51.2604433765188));
#49785=CARTESIAN_POINT('Ctrl Pts',(6.43560997955544,-34.5986241433973,16.6618192331215));
#49786=CARTESIAN_POINT('Ctrl Pts',(6.14415685965718,-34.9572124542593,16.8345062622337));
#49787=CARTESIAN_POINT('Ctrl Pts',(6.14415685965718,-51.791718716493,-18.1227061920256));
#49788=CARTESIAN_POINT('Ctrl Pts',(6.14415685965718,-16.8345062622337,-34.9572124542593));
#49789=CARTESIAN_POINT('Ctrl Pts',(6.14415685965718,18.1227061920256,-51.791718716493));
#49790=CARTESIAN_POINT('Ctrl Pts',(6.14415685965718,34.9572124542593,-16.8345062622337));
#49791=CARTESIAN_POINT('Ctrl Pts',(6.14415685965718,51.791718716493,18.1227061920256));
#49792=CARTESIAN_POINT('Ctrl Pts',(6.14415685965718,16.8345062622337,34.9572124542593));
#49793=CARTESIAN_POINT('Ctrl Pts',(6.14415685965718,-18.1227061920256,51.791718716493));
#49794=CARTESIAN_POINT('Ctrl Pts',(6.14415685965718,-34.9572124542593,16.8345062622337));
#49795=CARTESIAN_POINT('Ctrl Pts',(6.,-35.1377858481943,16.9214658255848));
#49796=CARTESIAN_POINT('Ctrl Pts',(6.,-52.0592516737791,-18.2163200226096));
#49797=CARTESIAN_POINT('Ctrl Pts',(6.,-16.9214658255848,-35.1377858481943));
#49798=CARTESIAN_POINT('Ctrl Pts',(6.,18.2163200226096,-52.0592516737791));
#49799=CARTESIAN_POINT('Ctrl Pts',(6.,35.1377858481943,-16.9214658255848));
#49800=CARTESIAN_POINT('Ctrl Pts',(6.,52.0592516737791,18.2163200226096));
#49801=CARTESIAN_POINT('Ctrl Pts',(6.,16.9214658255848,35.1377858481943));
#49802=CARTESIAN_POINT('Ctrl Pts',(6.,-18.2163200226096,52.0592516737791));
#49803=CARTESIAN_POINT('Ctrl Pts',(6.,-35.1377858481943,16.9214658255848));
#49804=CARTESIAN_POINT('Ctrl Pts',(15.,-29.7607187491733,7.11755713237394));
#49805=CARTESIAN_POINT('Ctrl Pts',(14.0108432136945,-30.7138276143533,5.80807302883452));
#49806=CARTESIAN_POINT('Ctrl Pts',(13.3692319443824,-31.2880423397517,4.92456278175723));
#49807=CARTESIAN_POINT('Ctrl Pts',(12.3476991724842,-32.1885965077159,3.9369824968736));
#49808=CARTESIAN_POINT('Ctrl Pts',(12.025018705019,-32.473062408263,3.62502689764848));
#49809=CARTESIAN_POINT('Ctrl Pts',(11.6666317570709,-32.7930634119362,3.28263944738858));
#49810=CARTESIAN_POINT('Ctrl Pts',(11.3593868751764,-33.0719731108646,3.0063009153141));
#49811=CARTESIAN_POINT('Ctrl Pts',(10.676771680913,-33.6916351769729,2.39235128793105));
#49812=CARTESIAN_POINT('Ctrl Pts',(10.1321636914396,-34.2060779331065,1.97784197265519));
#49813=CARTESIAN_POINT('Ctrl Pts',(9.56604173138329,-34.7743315804091,1.68073241792726));
#49814=CARTESIAN_POINT('Ctrl Pts',(9.34563078589188,-34.9955724657979,1.56505734701922));
#49815=CARTESIAN_POINT('Ctrl Pts',(9.12222951098695,-35.2252615616749,1.46777773062118));
#49816=CARTESIAN_POINT('Ctrl Pts',(8.88860711505279,-35.4734017321514,1.38109570926743));
#49817=CARTESIAN_POINT('Ctrl Pts',(8.75830600700743,-35.6118000181306,1.33274947351874));
#49818=CARTESIAN_POINT('Ctrl Pts',(8.62340343546551,-35.7561157762934,1.28545226594596));
#49819=CARTESIAN_POINT('Ctrl Pts',(8.40819516300419,-35.994889345564,1.22197488938494));
#49820=CARTESIAN_POINT('Ctrl Pts',(8.0244300682913,-36.4206767020539,1.10878034927987));
#49821=CARTESIAN_POINT('Ctrl Pts',(7.46417034513342,-37.0680247070473,0.984484082043485));
#49822=CARTESIAN_POINT('Ctrl Pts',(6.85957019142019,-37.843480699196,0.88897664134793));
#49823=CARTESIAN_POINT('Ctrl Pts',(6.58024553736738,-38.2017405762566,0.844852301206911));
#49824=CARTESIAN_POINT('Ctrl Pts',(6.28976782192772,-38.5882317623753,0.829056343619504));
#49825=CARTESIAN_POINT('Ctrl Pts',(6.,-38.9911990462069,0.828490759799981));
#49826=CARTESIAN_POINT('Ctrl Pts',(2.09999999999999,-15.7813123397985,0.900000000000003));
#49827=CARTESIAN_POINT('Ctrl Pts',(2.73333333333332,-15.7813123397985,0.900000000000003));
#49828=CARTESIAN_POINT('Ctrl Pts',(3.36803860157905,-15.7813180616194,0.899953654229283));
#49829=CARTESIAN_POINT('Ctrl Pts',(4.25277800527128,-15.7813208936813,0.899924760368668));
#49830=CARTESIAN_POINT('Ctrl Pts',(4.77267831987932,-15.7818921151941,0.891519719936119));
#49831=CARTESIAN_POINT('Ctrl Pts',(5.76857910493608,-15.7835993122471,0.867147114519683));
#49832=CARTESIAN_POINT('Ctrl Pts',(6.48509785298667,-15.7836071130985,0.867805461117988));
#49833=CARTESIAN_POINT('Ctrl Pts',(6.99867669895435,-15.7810493145741,0.901608701736404));
#49834=CARTESIAN_POINT('Ctrl Pts',(7.12481601332274,-15.7805124139621,0.910184915185508));
#49835=CARTESIAN_POINT('Ctrl Pts',(7.37171888970191,-15.7795536904041,0.928255643534913));
#49836=CARTESIAN_POINT('Ctrl Pts',(7.68212706220351,-15.7784608126719,0.95364774366657));
#49837=CARTESIAN_POINT('Ctrl Pts',(8.05075476794032,-15.7769500570881,0.98932824296244));
#49838=CARTESIAN_POINT('Ctrl Pts',(8.4150539939394,-15.7748901547651,1.03111723775223));
#49839=CARTESIAN_POINT('Ctrl Pts',(9.01076228194079,-15.7699352805976,1.11250789981985));
#49840=CARTESIAN_POINT('Ctrl Pts',(9.46311166877534,-15.7626389942107,1.19806894000414));
#49841=CARTESIAN_POINT('Ctrl Pts',(10.2678611694051,-15.7401422438828,1.39809158506708));
#49842=CARTESIAN_POINT('Ctrl Pts',(10.9805041482584,-15.7177390832667,1.65102715488742));
#49843=CARTESIAN_POINT('Ctrl Pts',(11.7910350621702,-15.6753561835242,2.018832180911));
#49844=CARTESIAN_POINT('Ctrl Pts',(12.2471627654155,-15.6444015292051,2.24062830476412));
#49845=CARTESIAN_POINT('Ctrl Pts',(12.4732580281126,-15.6263203413021,2.35401357536145));
#49846=CARTESIAN_POINT('Ctrl Pts',(12.8351268106022,-15.5948338653055,2.53703642714019));
#49847=CARTESIAN_POINT('Ctrl Pts',(13.2802529432254,-15.5503636458461,2.78452402958302));
#49848=CARTESIAN_POINT('Ctrl Pts',(14.1612575904519,-15.4429889615419,3.34567779498745));
#49849=CARTESIAN_POINT('Ctrl Pts',(14.7820737708942,-15.3388270460161,3.80399343913107));
#49850=CARTESIAN_POINT('Ctrl Pts',(15.1979896574214,-15.2534284724017,4.11495301335945));
#49851=CARTESIAN_POINT('Ctrl Pts',(2.09999999999999,-23.5174523402227,0.900000000000004));
#49852=CARTESIAN_POINT('Ctrl Pts',(2.73333333333332,-23.5174523402227,0.900000000000004));
#49853=CARTESIAN_POINT('Ctrl Pts',(3.3687269008229,-23.5174503117464,0.899999549356805));
#49854=CARTESIAN_POINT('Ctrl Pts',(4.25416629436656,-23.5174495574097,0.899986128047576));
#49855=CARTESIAN_POINT('Ctrl Pts',(4.78311339604061,-23.5180672355084,0.887379402076836));
#49856=CARTESIAN_POINT('Ctrl Pts',(5.77495354160743,-23.5199279942482,0.851096896517873));
#49857=CARTESIAN_POINT('Ctrl Pts',(6.47498972136719,-23.5199204649197,0.85254775775783));
#49858=CARTESIAN_POINT('Ctrl Pts',(6.96729289121827,-23.5171313867364,0.901565775281088));
#49859=CARTESIAN_POINT('Ctrl Pts',(7.09311090714753,-23.5165727443299,0.914323892311043));
#49860=CARTESIAN_POINT('Ctrl Pts',(7.3363104955997,-23.5156659563351,0.940991080822883));
#49861=CARTESIAN_POINT('Ctrl Pts',(7.64238643469451,-23.5147669843648,0.978505552682822));
#49862=CARTESIAN_POINT('Ctrl Pts',(8.00394198529363,-23.5135608591914,1.0310088470534));
#49863=CARTESIAN_POINT('Ctrl Pts',(8.36003532842669,-23.51172134836,1.09241611183573));
#49864=CARTESIAN_POINT('Ctrl Pts',(8.93970255550973,-23.5067933041018,1.21153595067129));
#49865=CARTESIAN_POINT('Ctrl Pts',(9.37531769324352,-23.4985467770246,1.33634734778052));
#49866=CARTESIAN_POINT('Ctrl Pts',(10.1434238337742,-23.4715958512647,1.62573582070569));
#49867=CARTESIAN_POINT('Ctrl Pts',(10.8343148881383,-23.4466861730614,1.9942694300716));
#49868=CARTESIAN_POINT('Ctrl Pts',(11.6347008962811,-23.3955621594738,2.53783642516313));
#49869=CARTESIAN_POINT('Ctrl Pts',(12.0872732667126,-23.3565546277241,2.86696783800558));
#49870=CARTESIAN_POINT('Ctrl Pts',(12.3122637721678,-23.3331927346526,3.03568289878328));
#49871=CARTESIAN_POINT('Ctrl Pts',(12.6726001818386,-23.2920224649212,3.30823650944636));
#49872=CARTESIAN_POINT('Ctrl Pts',(13.1110203697175,-23.2345645363005,3.67373154677588));
#49873=CARTESIAN_POINT('Ctrl Pts',(13.9921386008757,-23.093173534576,4.51098032026392));
#49874=CARTESIAN_POINT('Ctrl Pts',(14.6125773377935,-22.9522889563178,5.19806642891103));
#49875=CARTESIAN_POINT('Ctrl Pts',(15.0291266285127,-22.834727375518,5.66394619523217));
#49876=CARTESIAN_POINT('Ctrl Pts',(2.09999999999999,-31.253592340647,0.900000000000005));
#49877=CARTESIAN_POINT('Ctrl Pts',(2.73333333333333,-31.253592340647,0.900000000000005));
#49878=CARTESIAN_POINT('Ctrl Pts',(3.36946298994113,-31.253597129858,0.899967083396557));
#49879=CARTESIAN_POINT('Ctrl Pts',(4.25563250306681,-31.2535998064671,0.899927315911795));
#49880=CARTESIAN_POINT('Ctrl Pts',(4.793607610529,-31.2542714423515,0.882902120180317));
#49881=CARTESIAN_POINT('Ctrl Pts',(5.78148222806676,-31.256287669969,0.834747506040562));
#49882=CARTESIAN_POINT('Ctrl Pts',(6.46489469701572,-31.2562883708318,0.837373215514036));
#49883=CARTESIAN_POINT('Ctrl Pts',(6.93657638553836,-31.2532799135509,0.899507277096636));
#49884=CARTESIAN_POINT('Ctrl Pts',(7.0620883058075,-31.2527009610395,0.91640744616794));
#49885=CARTESIAN_POINT('Ctrl Pts',(7.30171951451256,-31.2518492172623,0.951277918119689));
#49886=CARTESIAN_POINT('Ctrl Pts',(7.60369867143904,-31.2511567052462,1.00034060541384));
#49887=CARTESIAN_POINT('Ctrl Pts',(7.95863609743802,-31.250265994518,1.06869690052304));
#49888=CARTESIAN_POINT('Ctrl Pts',(8.30734467161686,-31.2486814680989,1.14828732937022));
#49889=CARTESIAN_POINT('Ctrl Pts',(8.87313675628991,-31.2438333199221,1.30219016402905));
#49890=CARTESIAN_POINT('Ctrl Pts',(9.29621494250681,-31.2348126008038,1.46187419583854));
#49891=CARTESIAN_POINT('Ctrl Pts',(10.0463012266451,-31.203926559761,1.83186702435988));
#49892=CARTESIAN_POINT('Ctrl Pts',(10.7405413064001,-31.1770796248539,2.31584417428653));
#49893=CARTESIAN_POINT('Ctrl Pts',(11.548246551431,-31.1171997774263,3.04151994117155));
#49894=CARTESIAN_POINT('Ctrl Pts',(12.004199888209,-31.0700709489218,3.48088598485862));
#49895=CARTESIAN_POINT('Ctrl Pts',(12.2304316701899,-31.0414054563015,3.70603673720389));
#49896=CARTESIAN_POINT('Ctrl Pts',(12.5924678805365,-30.9905349539073,4.06954570137746));
#49897=CARTESIAN_POINT('Ctrl Pts',(13.0427854461794,-30.9189256840333,4.56466621801912));
#49898=CARTESIAN_POINT('Ctrl Pts',(13.9385950929121,-30.7403061321327,5.69639486896618));
#49899=CARTESIAN_POINT('Ctrl Pts',(14.5670688438605,-30.560172646277,6.62087479005202));
#49900=CARTESIAN_POINT('Ctrl Pts',(14.9853697475044,-30.4091322526247,7.24399554120779));
#49901=CARTESIAN_POINT('Ctrl Pts',(2.09999999999999,-38.9897323410713,0.900000000000005));
#49902=CARTESIAN_POINT('Ctrl Pts',(2.73333333333332,-38.9897323410713,0.900000000000005));
#49903=CARTESIAN_POINT('Ctrl Pts',(3.37021439053497,-38.9897437514265,0.899948482776489));
#49904=CARTESIAN_POINT('Ctrl Pts',(4.25713776543909,-38.9897498389542,0.899888266525458));
#49905=CARTESIAN_POINT('Ctrl Pts',(4.80404692086918,-38.990474960491,0.878261830529841));
#49906=CARTESIAN_POINT('Ctrl Pts',(5.78816029898518,-38.9926471520414,0.818329038315272));
#49907=CARTESIAN_POINT('Ctrl Pts',(6.45448401595128,-38.9926543924743,0.822526832763617));
#49908=CARTESIAN_POINT('Ctrl Pts',(6.90694151240769,-38.9894292569544,0.896112921981724));
#49909=CARTESIAN_POINT('Ctrl Pts',(7.03217742077181,-38.9888307738593,0.917127783371819));
#49910=CARTESIAN_POINT('Ctrl Pts',(7.26852796949471,-38.9880361255997,0.959898627245754));
#49911=CARTESIAN_POINT('Ctrl Pts',(7.56686701397648,-38.987554172558,1.02013588655783));
#49912=CARTESIAN_POINT('Ctrl Pts',(7.91608364547376,-38.9869869932131,1.10372729413102));
#49913=CARTESIAN_POINT('Ctrl Pts',(8.25887925774823,-38.9856712995636,1.20083627874114));
#49914=CARTESIAN_POINT('Ctrl Pts',(8.8143057136887,-38.9809314590746,1.38853371701586));
#49915=CARTESIAN_POINT('Ctrl Pts',(9.23056764068725,-38.9711733909723,1.58316088294249));
#49916=CARTESIAN_POINT('Ctrl Pts',(9.9765255462537,-38.9361908258605,2.04109193749097));
#49917=CARTESIAN_POINT('Ctrl Pts',(10.6790409718292,-38.9067650394502,2.6532312853716));
#49918=CARTESIAN_POINT('Ctrl Pts',(11.4921056515298,-38.8370824836761,3.56780480358298));
#49919=CARTESIAN_POINT('Ctrl Pts',(11.9504568599563,-38.7812570292348,4.119988399869));
#49920=CARTESIAN_POINT('Ctrl Pts',(12.1774856937747,-38.7470142391924,4.4023497722438));
#49921=CARTESIAN_POINT('Ctrl Pts',(12.5406836647159,-38.6860166444278,4.85788735474899));
#49922=CARTESIAN_POINT('Ctrl Pts',(12.9976779503012,-38.5991062464697,5.48794489488544));
#49923=CARTESIAN_POINT('Ctrl Pts',(13.899403431329,-38.3817347701346,6.91519011870003));
#49924=CARTESIAN_POINT('Ctrl Pts',(14.5324532885843,-38.1613150005834,8.07725552357689));
#49925=CARTESIAN_POINT('Ctrl Pts',(14.9514110803021,-37.9761728551056,8.85721942423245));
#49926=CARTESIAN_POINT('',(3.2,-37.5892271801377,0.89999999999999));
#49927=CARTESIAN_POINT('Ctrl Pts',(3.2,-37.5892271801377,0.900000000000005));
#49928=CARTESIAN_POINT('Ctrl Pts',(3.56152274835416,-36.4727023625927,0.900000000000005));
#49929=CARTESIAN_POINT('Ctrl Pts',(3.95224584525393,-35.3420203470068,0.905801001195174));
#49930=CARTESIAN_POINT('Ctrl Pts',(4.7876743012376,-33.0900361849772,0.883613319940321));
#49931=CARTESIAN_POINT('Ctrl Pts',(5.21513946232122,-32.0121842271598,0.857420319092421));
#49932=CARTESIAN_POINT('Ctrl Pts',(6.7954877540273,-28.2792370299721,0.82385346267847));
#49933=CARTESIAN_POINT('Ctrl Pts',(7.94016295939677,-26.0613850693145,1.01713589289149));
#49934=CARTESIAN_POINT('Ctrl Pts',(9.46271935276041,-23.3002380102246,1.33514989708753));
#49935=CARTESIAN_POINT('Ctrl Pts',(10.1385443659136,-22.1771939355819,1.56158379060409));
#49936=CARTESIAN_POINT('Ctrl Pts',(11.5967860400749,-19.9286553808136,2.23301757819717));
#49937=CARTESIAN_POINT('Ctrl Pts',(12.3997356677083,-18.7587345375746,2.6115335830299));
#49938=CARTESIAN_POINT('Ctrl Pts',(13.6850585208096,-16.9850659799596,3.25579646640259));
#49939=CARTESIAN_POINT('Ctrl Pts',(14.3457395898606,-16.1131272918145,3.62837109684756));
#49940=CARTESIAN_POINT('Ctrl Pts',(15.,-15.2928725900315,3.96737244938057));
#49941=CARTESIAN_POINT('Ctrl Pts',(2.79815339721959,-38.5299211738669,0.89998254368834));
#49942=CARTESIAN_POINT('Ctrl Pts',(2.93286463944684,-38.2164608351329,0.899976638205042));
#49943=CARTESIAN_POINT('Ctrl Pts',(3.06773361277345,-37.9028006789536,0.899969723070092));
#49944=CARTESIAN_POINT('Ctrl Pts',(3.20258714969926,-37.5892342471181,0.89996249608849));
#49945=CARTESIAN_POINT('Origin',(2.9,0.,0.));
#49946=CARTESIAN_POINT('',(3.2,-34.2572188230213,15.4984824583453));
#49947=CARTESIAN_POINT('Origin',(3.2,0.,0.));
#49948=CARTESIAN_POINT('Ctrl Pts',(3.19854856993727,-34.2571641451328,15.4985534066746));
#49949=CARTESIAN_POINT('Ctrl Pts',(3.06442805771908,-34.5398277577011,15.6346586929013));
#49950=CARTESIAN_POINT('Ctrl Pts',(2.93030968617731,-34.8224399543122,15.7707394686964));
#49951=CARTESIAN_POINT('Ctrl Pts',(2.7963008307409,-35.1047259901887,15.9066658257295));
#49952=CARTESIAN_POINT('Ctrl Pts',(2.10000000000001,-10.5446976527894,11.7791447047943));
#49953=CARTESIAN_POINT('Ctrl Pts',(2.73333333333334,-10.5446976527894,11.7791447047943));
#49954=CARTESIAN_POINT('Ctrl Pts',(3.36597186493151,-10.5446228424995,11.7791929127825));
#49955=CARTESIAN_POINT('Ctrl Pts',(4.12348416497485,-10.544599841335,11.7792076131232));
#49956=CARTESIAN_POINT('Ctrl Pts',(4.36307794326233,-10.5460660330961,11.7779222515897));
#49957=CARTESIAN_POINT('Ctrl Pts',(4.85756380192522,-10.5528379728112,11.7720020900147));
#49958=CARTESIAN_POINT('Ctrl Pts',(5.73898435898537,-10.5689627252743,11.7579308551903));
#49959=CARTESIAN_POINT('Ctrl Pts',(6.5260525135352,-10.569426646963,11.7575444691643));
#49960=CARTESIAN_POINT('Ctrl Pts',(7.12756341256172,-10.5394024697514,11.7835517417896));
#49961=CARTESIAN_POINT('Ctrl Pts',(7.25505875202547,-10.5328878017875,11.7893155337016));
#49962=CARTESIAN_POINT('Ctrl Pts',(7.51731750157009,-10.5186059928894,11.8021864593304));
#49963=CARTESIAN_POINT('Ctrl Pts',(7.84588509512945,-10.4986704206583,11.8204784852481));
#49964=CARTESIAN_POINT('Ctrl Pts',(8.24416390812632,-10.4702119644218,11.8466119866418));
#49965=CARTESIAN_POINT('Ctrl Pts',(8.77646398006391,-10.4246920294427,11.8878046798892));
#49966=CARTESIAN_POINT('Ctrl Pts',(9.4411345989597,-10.3508464915215,11.9526079594429));
#49967=CARTESIAN_POINT('Ctrl Pts',(9.96388516997986,-10.26693159457,12.0222081514324));
#49968=CARTESIAN_POINT('Ctrl Pts',(11.1189136052353,-10.0417705507235,12.2032651710146));
#49969=CARTESIAN_POINT('Ctrl Pts',(12.080454797577,-9.73217262268696,12.461784447063));
#49970=CARTESIAN_POINT('Ctrl Pts',(13.0008419744711,-9.36882675367162,12.7304564924823));
#49971=CARTESIAN_POINT('Ctrl Pts',(13.2108186458783,-9.28294322582199,12.7920469879376));
#49972=CARTESIAN_POINT('Ctrl Pts',(13.3144418038317,-9.23989237192285,12.8223813622727));
#49973=CARTESIAN_POINT('Ctrl Pts',(13.3733216886662,-9.21525036961191,12.8395866023987));
#49974=CARTESIAN_POINT('Ctrl Pts',(13.4026009224713,-9.20293900388632,12.8481288210721));
#49975=CARTESIAN_POINT('Ctrl Pts',(13.6877921880979,-9.08273430560209,12.9312335785886));
#49976=CARTESIAN_POINT('Ctrl Pts',(14.2465854854714,-8.82185938319892,13.1087324358622));
#49977=CARTESIAN_POINT('Ctrl Pts',(14.7537307590314,-8.54348998776827,13.2903258258105));
#49978=CARTESIAN_POINT('Ctrl Pts',(14.9999999999997,-8.40014929121784,13.3809374892743));
#49979=CARTESIAN_POINT('Ctrl Pts',(2.10000000000001,-15.3675852715397,17.8268544917116));
#49980=CARTESIAN_POINT('Ctrl Pts',(2.73333333333334,-15.3675852715397,17.8268544917116));
#49981=CARTESIAN_POINT('Ctrl Pts',(3.36558673280158,-15.3675309972709,17.8268931877247));
#49982=CARTESIAN_POINT('Ctrl Pts',(4.12268323605138,-15.3675155744444,17.8269040940857));
#49983=CARTESIAN_POINT('Ctrl Pts',(4.35699688852519,-15.3697095936867,17.8250550840541));
#49984=CARTESIAN_POINT('Ctrl Pts',(4.84800076874878,-15.3799128467904,17.8164742582301));
#49985=CARTESIAN_POINT('Ctrl Pts',(5.73068676826158,-15.4043424369138,17.7959526739925));
#49986=CARTESIAN_POINT('Ctrl Pts',(6.53594823423175,-15.4054106862613,17.7950986738855));
#49987=CARTESIAN_POINT('Ctrl Pts',(7.1587012295895,-15.3589748828166,17.8338974101007));
#49988=CARTESIAN_POINT('Ctrl Pts',(7.28652620235657,-15.349099382339,17.8423111652112));
#49989=CARTESIAN_POINT('Ctrl Pts',(7.55249020735376,-15.3272888912512,17.8612448875003));
#49990=CARTESIAN_POINT('Ctrl Pts',(7.88541634569422,-15.296871309982,17.8881352701714));
#49991=CARTESIAN_POINT('Ctrl Pts',(8.29077087410829,-15.2532979369236,17.9266727888899));
#49992=CARTESIAN_POINT('Ctrl Pts',(8.83404175048086,-15.1835241926749,17.9875016868031));
#49993=CARTESIAN_POINT('Ctrl Pts',(9.51598698571077,-15.0699838270507,18.0834946709078));
#49994=CARTESIAN_POINT('Ctrl Pts',(10.0563081198985,-14.9404974117035,18.1870277549497));
#49995=CARTESIAN_POINT('Ctrl Pts',(11.2545362612146,-14.5920275075708,18.4572762053696));
#49996=CARTESIAN_POINT('Ctrl Pts',(12.234198837956,-14.1169082623771,18.8390235742434));
#49997=CARTESIAN_POINT('Ctrl Pts',(13.1607933780956,-13.5654020914808,19.230311654985));
#49998=CARTESIAN_POINT('Ctrl Pts',(13.3718937697732,-13.4351891537631,19.319864196407));
#49999=CARTESIAN_POINT('Ctrl Pts',(13.4759419453006,-13.3699770181973,19.3639050860963));
#50000=CARTESIAN_POINT('Ctrl Pts',(13.5350456770886,-13.3326614567115,19.3888723313051));
#50001=CARTESIAN_POINT('Ctrl Pts',(13.5644155519561,-13.3140232750371,19.4012615507239));
#50002=CARTESIAN_POINT('Ctrl Pts',(13.8509041424671,-13.1320888318584,19.5218042916467));
#50003=CARTESIAN_POINT('Ctrl Pts',(14.4159109000634,-12.7349925891042,19.7812032596373));
#50004=CARTESIAN_POINT('Ctrl Pts',(14.9236315787721,-12.3149176903677,20.0437400385662));
#50005=CARTESIAN_POINT('Ctrl Pts',(15.169681381964,-12.0987180801296,20.1745520350237));
#50006=CARTESIAN_POINT('Ctrl Pts',(2.10000000000001,-20.1904728902899,23.8745642786288));
#50007=CARTESIAN_POINT('Ctrl Pts',(2.73333333333334,-20.1904728902899,23.8745642786288));
#50008=CARTESIAN_POINT('Ctrl Pts',(3.36511712968511,-20.1903753535268,23.8746272630908));
#50009=CARTESIAN_POINT('Ctrl Pts',(4.121772800169,-20.1903476480764,23.8746447505209));
#50010=CARTESIAN_POINT('Ctrl Pts',(4.35079402756333,-20.1932192199635,23.8722707271526));
#50011=CARTESIAN_POINT('Ctrl Pts',(4.8383303920068,-20.2067520378879,23.8611070555741));
#50012=CARTESIAN_POINT('Ctrl Pts',(5.72216975316483,-20.2394914205133,23.8341259601004));
#50013=CARTESIAN_POINT('Ctrl Pts',(6.54571765172787,-20.2414694717274,23.8325340970902));
#50014=CARTESIAN_POINT('Ctrl Pts',(7.18903482077842,-20.1769761054267,23.8854220896065));
#50015=CARTESIAN_POINT('Ctrl Pts',(7.31717297311608,-20.1637083631821,23.8965091360279));
#50016=CARTESIAN_POINT('Ctrl Pts',(7.58670489366458,-20.1340587603168,23.9217490624975));
#50017=CARTESIAN_POINT('Ctrl Pts',(7.9237359471977,-20.0927097147463,23.9575814811403));
#50018=CARTESIAN_POINT('Ctrl Pts',(8.33570803507908,-20.033244865644,24.0091266187489));
#50019=CARTESIAN_POINT('Ctrl Pts',(8.88882165089384,-19.9377329009591,24.0907234000965));
#50020=CARTESIAN_POINT('Ctrl Pts',(9.58537164389797,-19.7816931867799,24.220032764451));
#50021=CARTESIAN_POINT('Ctrl Pts',(10.1375595094415,-19.6030413696372,24.3601352854168));
#50022=CARTESIAN_POINT('Ctrl Pts',(11.3565368036444,-19.1228605744218,24.7254965438271));
#50023=CARTESIAN_POINT('Ctrl Pts',(12.3228216885107,-18.4857791115471,25.2268877754026));
#50024=CARTESIAN_POINT('Ctrl Pts',(13.2438406910188,-17.750936776662,25.7372203191382));
#50025=CARTESIAN_POINT('Ctrl Pts',(13.4536869673219,-17.5772178337914,25.8541109862439));
#50026=CARTESIAN_POINT('Ctrl Pts',(13.5572505985671,-17.4902288030533,25.9115731915362));
#50027=CARTESIAN_POINT('Ctrl Pts',(13.6160898983384,-17.4404375643633,25.9441542389479));
#50028=CARTESIAN_POINT('Ctrl Pts',(13.6453470368304,-17.4155658515524,25.9603212957986));
#50029=CARTESIAN_POINT('Ctrl Pts',(13.9304355722608,-17.172772609941,26.1176229975696));
#50030=CARTESIAN_POINT('Ctrl Pts',(14.4834756840846,-16.6497787408563,26.4523558285942));
#50031=CARTESIAN_POINT('Ctrl Pts',(14.98335392639,-16.0960001898358,26.7914585964211));
#50032=CARTESIAN_POINT('Ctrl Pts',(15.2260186760796,-15.8109142456191,26.9604788277526));
#50033=CARTESIAN_POINT('Ctrl Pts',(2.10000000000001,-25.0133605090401,29.9222740655461));
#50034=CARTESIAN_POINT('Ctrl Pts',(2.73333333333334,-25.0133605090401,29.9222740655461));
#50035=CARTESIAN_POINT('Ctrl Pts',(3.3646388685928,-25.0132463360064,29.922340718268));
#50036=CARTESIAN_POINT('Ctrl Pts',(4.12085565775573,-25.013214625916,29.9223584112847));
#50037=CARTESIAN_POINT('Ctrl Pts',(4.34457171221109,-25.0167236229088,29.9194913308185));
#50038=CARTESIAN_POINT('Ctrl Pts',(4.82871450329817,-25.033495966797,29.9058171622753));
#50039=CARTESIAN_POINT('Ctrl Pts',(5.71350326403012,-25.0746098135769,29.8723244268729));
#50040=CARTESIAN_POINT('Ctrl Pts',(6.55584056634621,-25.0778382570217,29.869726006846));
#50041=CARTESIAN_POINT('Ctrl Pts',(7.21833096387863,-24.9939949679208,29.9377306666232));
#50042=CARTESIAN_POINT('Ctrl Pts',(7.346753012671,-24.9773138147238,29.9515069240579));
#50043=CARTESIAN_POINT('Ctrl Pts',(7.61956458160806,-24.939587672514,29.9832397322665));
#50044=CARTESIAN_POINT('Ctrl Pts',(7.96025303539806,-24.8870218547869,30.0282369104503));
#50045=CARTESIAN_POINT('Ctrl Pts',(8.37793548706869,-24.8111754981506,30.0931695423523));
#50046=CARTESIAN_POINT('Ctrl Pts',(8.93897086621509,-24.689246172225,30.196054236466));
#50047=CARTESIAN_POINT('Ctrl Pts',(9.64588723426547,-24.4899298952911,30.3592522311079));
#50048=CARTESIAN_POINT('Ctrl Pts',(10.203573833095,-24.2630022112468,30.5352010907534));
#50049=CARTESIAN_POINT('Ctrl Pts',(11.4269679031769,-23.6583467725441,30.990143976638));
#50050=CARTESIAN_POINT('Ctrl Pts',(12.3794536276398,-22.8720122911001,31.6023997058208));
#50051=CARTESIAN_POINT('Ctrl Pts',(13.2972732213526,-21.957416724469,32.2303091018155));
#50052=CARTESIAN_POINT('Ctrl Pts',(13.5062425804685,-21.7410324541202,32.3741745574719));
#50053=CARTESIAN_POINT('Ctrl Pts',(13.6095151823004,-21.6325747352925,32.4449609360363));
#50054=CARTESIAN_POINT('Ctrl Pts',(13.6681882314017,-21.570479426627,32.485102482123));
#50055=CARTESIAN_POINT('Ctrl Pts',(13.6973807045977,-21.5394470731678,32.5050297522711));
#50056=CARTESIAN_POINT('Ctrl Pts',(13.9814771447632,-21.2367010730438,32.6987871955309));
#50057=CARTESIAN_POINT('Ctrl Pts',(14.5280907883129,-20.5925372303219,33.1065563793246));
#50058=CARTESIAN_POINT('Ctrl Pts',(15.0243070371674,-19.9061830796774,33.5223603522699));
#50059=CARTESIAN_POINT('Ctrl Pts',(15.2656150130537,-19.5525316786335,33.7298078962616));
#50060=CARTESIAN_POINT('',(3.2,-24.1401481407882,28.8273003894017));
#50061=CARTESIAN_POINT('Ctrl Pts',(3.198471221358,-24.1400746652962,28.8273438520674));
#50062=CARTESIAN_POINT('Ctrl Pts',(3.06436400315688,-24.3356906767046,29.0726148396917));
#50063=CARTESIAN_POINT('Ctrl Pts',(2.93025965397856,-24.531270609612,29.3178398607618));
#50064=CARTESIAN_POINT('Ctrl Pts',(2.79626375401858,-24.726623224287,29.5627827604819));
#50065=CARTESIAN_POINT('',(15.,-8.40014929122428,13.3809374892862));
#50066=CARTESIAN_POINT('Ctrl Pts',(15.,-8.40014929122428,13.3809374892862));
#50067=CARTESIAN_POINT('Ctrl Pts',(14.4897165779514,-8.96964310337579,13.6761925967553));
#50068=CARTESIAN_POINT('Ctrl Pts',(13.983380302661,-9.54630274603464,13.9938123448954));
#50069=CARTESIAN_POINT('Ctrl Pts',(13.4460287676664,-10.1567673260582,14.3773166678879));
#50070=CARTESIAN_POINT('Ctrl Pts',(12.828265568102,-10.858584530656,14.8182102769869));
#50071=CARTESIAN_POINT('Ctrl Pts',(12.1555414089414,-11.6739241299084,15.3314605852401));
#50072=CARTESIAN_POINT('Ctrl Pts',(11.5904908073485,-12.3652690628769,15.8169736923657));
#50073=CARTESIAN_POINT('Ctrl Pts',(11.1143368259563,-12.9478481122936,16.2261034204366));
#50074=CARTESIAN_POINT('Ctrl Pts',(10.6953158949566,-13.4647168679094,16.6236326882214));
#50075=CARTESIAN_POINT('Ctrl Pts',(10.2957959918397,-13.9533753754527,17.0392327535223));
#50076=CARTESIAN_POINT('Ctrl Pts',(10.0450888109516,-14.2600189140784,17.3000305759477));
#50077=CARTESIAN_POINT('Ctrl Pts',(9.80235305583622,-14.5561912626385,17.5673906464135));
#50078=CARTESIAN_POINT('Ctrl Pts',(9.56010106236485,-14.8537124907605,17.8474631215382));
#50079=CARTESIAN_POINT('Ctrl Pts',(9.36613602944513,-15.0919301994367,18.0717100558112));
#50080=CARTESIAN_POINT('Ctrl Pts',(9.15248571301987,-15.3550807294054,18.3262463074901));
#50081=CARTESIAN_POINT('Ctrl Pts',(8.89022359835155,-15.6828751797185,18.6565063967794));
#50082=CARTESIAN_POINT('Ctrl Pts',(8.39222406115036,-16.3053115722546,19.2836246972252));
#50083=CARTESIAN_POINT('Ctrl Pts',(7.76643777378863,-17.1018024085652,20.1343268458305));
#50084=CARTESIAN_POINT('Ctrl Pts',(7.10363554123529,-18.0137184170549,21.1546025207168));
#50085=CARTESIAN_POINT('Ctrl Pts',(6.23550018248797,-19.2081418699258,22.4909549732834));
#50086=CARTESIAN_POINT('Ctrl Pts',(5.31040885822886,-20.4995343283109,24.2016142119962));
#50087=CARTESIAN_POINT('Ctrl Pts',(4.46416616904574,-21.8861900198845,25.9864862188989));
#50088=CARTESIAN_POINT('Ctrl Pts',(4.30741751124639,-22.1430388190083,26.3170962141187));
#50089=CARTESIAN_POINT('Ctrl Pts',(4.15262292089116,-22.4044433616665,26.6507954384915));
#50090=CARTESIAN_POINT('Ctrl Pts',(4.,-22.6717457083367,26.9859819793801));
#50091=CARTESIAN_POINT('Ctrl Pts',(3.72434973283383,-23.1545169909432,27.5913580199313));
#50092=CARTESIAN_POINT('Ctrl Pts',(3.45587123478797,-23.6474469973648,28.2094726972278));
#50093=CARTESIAN_POINT('Ctrl Pts',(3.2,-24.1401481407882,28.8273003894017));
#50094=CARTESIAN_POINT('',(15.,-15.7403794776611,26.2411976460531));
#50095=CARTESIAN_POINT('Ctrl Pts',(15.,-15.7403794776611,26.2411976460531));
#50096=CARTESIAN_POINT('Ctrl Pts',(15.,-13.5381067497035,22.4153192789932));
#50097=CARTESIAN_POINT('Ctrl Pts',(15.,-10.9320820978596,17.8690631788246));
#50098=CARTESIAN_POINT('Ctrl Pts',(15.,-8.40014929122428,13.3809374892862));
#50099=CARTESIAN_POINT('Ctrl Pts',(6.,-25.0681110272506,29.8762415562171));
#50100=CARTESIAN_POINT('Ctrl Pts',(6.38595465246566,-24.7328386442811,29.4570965039835));
#50101=CARTESIAN_POINT('Ctrl Pts',(6.77023648668261,-24.4008805391967,29.0790088991504));
#50102=CARTESIAN_POINT('Ctrl Pts',(7.13915213286206,-24.0702538280742,28.757013583941));
#50103=CARTESIAN_POINT('Ctrl Pts',(8.10667920093243,-23.2031442442141,27.9125409071019));
#50104=CARTESIAN_POINT('Ctrl Pts',(8.98019888747383,-22.4610197697564,27.3528547579367));
#50105=CARTESIAN_POINT('Ctrl Pts',(9.46656009721086,-22.027289835851,27.0867256780847));
#50106=CARTESIAN_POINT('Ctrl Pts',(9.65648624874925,-21.8579164246816,26.9828011237888));
#50107=CARTESIAN_POINT('Ctrl Pts',(9.79228848853746,-21.7349621561682,26.9151380286895));
#50108=CARTESIAN_POINT('Ctrl Pts',(9.94593825727838,-21.5936891727254,26.8433208059295));
#50109=CARTESIAN_POINT('Ctrl Pts',(10.106574086601,-21.4459928693584,26.768238238398));
#50110=CARTESIAN_POINT('Ctrl Pts',(10.2660951669676,-21.2965784352636,26.7002859221237));
#50111=CARTESIAN_POINT('Ctrl Pts',(10.4261869573617,-21.1424957123869,26.6392512968066));
#50112=CARTESIAN_POINT('Ctrl Pts',(10.8065549509411,-20.7764048841091,26.4942368778062));
#50113=CARTESIAN_POINT('Ctrl Pts',(11.1894211925257,-20.3832825474409,26.3891427006873));
#50114=CARTESIAN_POINT('Ctrl Pts',(11.6023503255242,-19.9319102322466,26.3138080519751));
#50115=CARTESIAN_POINT('Ctrl Pts',(11.7531893954247,-19.7670282349209,26.2862890240476));
#50116=CARTESIAN_POINT('Ctrl Pts',(11.9080270687775,-19.5943009445266,26.2628721736317));
#50117=CARTESIAN_POINT('Ctrl Pts',(12.0681766131679,-19.4121014596106,26.2433088471935));
#50118=CARTESIAN_POINT('Ctrl Pts',(12.1838435903474,-19.2805090548735,26.2291793606483));
#50119=CARTESIAN_POINT('Ctrl Pts',(12.3100865410161,-19.135901739712,26.2150849420816));
#50120=CARTESIAN_POINT('Ctrl Pts',(12.5127093730712,-18.8980868317012,26.1997439459511));
#50121=CARTESIAN_POINT('Ctrl Pts',(12.7975492664042,-18.5637751830891,26.1781781250753));
#50122=CARTESIAN_POINT('Ctrl Pts',(13.1874566943566,-18.0938107160767,26.1632244670392));
#50123=CARTESIAN_POINT('Ctrl Pts',(13.6431584568239,-17.5374609190085,26.1582954681053));
#50124=CARTESIAN_POINT('Ctrl Pts',(14.069523646534,-17.0169270823873,26.1536837818257));
#50125=CARTESIAN_POINT('Ctrl Pts',(14.53311408767,-16.4047647574916,26.1852391011876));
#50126=CARTESIAN_POINT('Ctrl Pts',(15.,-15.7403794776611,26.2411976460531));
#50127=CARTESIAN_POINT('Origin',(15.,-1.89142793862867,8.2868872535455));
#50128=CARTESIAN_POINT('',(15.,-6.43313341740755,14.4300655106231));
#50129=CARTESIAN_POINT('Ctrl Pts',(15.,-6.43313341740755,14.4300655106231));
#50130=CARTESIAN_POINT('Ctrl Pts',(15.,-7.09235331145211,14.1361756785447));
#50131=CARTESIAN_POINT('Ctrl Pts',(15.,-7.73147565640373,13.7970939349841));
#50132=CARTESIAN_POINT('Ctrl Pts',(15.,-8.36396313002149,13.4036029817217));
#50133=CARTESIAN_POINT('Ctrl Pts',(15.,-8.38206859073762,13.3922880081493));
#50134=CARTESIAN_POINT('Ctrl Pts',(15.,-8.40014929122428,13.3809374892862));
#50135=CARTESIAN_POINT('',(15.,-12.9907743917407,27.7055911451623));
#50136=CARTESIAN_POINT('Ctrl Pts',(15.,-6.43313341740754,14.4300655106231));
#50137=CARTESIAN_POINT('Ctrl Pts',(15.,-8.80709419494161,19.1667769918265));
#50138=CARTESIAN_POINT('Ctrl Pts',(15.,-11.1607986514941,23.9627962274343));
#50139=CARTESIAN_POINT('Ctrl Pts',(15.,-12.9907743917407,27.7055911451623));
#50140=CARTESIAN_POINT('Origin',(15.,0.,0.));
#50141=CARTESIAN_POINT('Ctrl Pts',(15.,-6.80914057906322,29.8327941127638));
#50142=CARTESIAN_POINT('Ctrl Pts',(15.,-36.641934691827,23.0236535337006));
#50143=CARTESIAN_POINT('Ctrl Pts',(15.,-29.8327941127638,-6.80914057906322));
#50144=CARTESIAN_POINT('Ctrl Pts',(15.,-23.0236535337006,-36.641934691827));
#50145=CARTESIAN_POINT('Ctrl Pts',(15.,6.80914057906322,-29.8327941127638));
#50146=CARTESIAN_POINT('Ctrl Pts',(15.,36.641934691827,-23.0236535337006));
#50147=CARTESIAN_POINT('Ctrl Pts',(15.,29.8327941127638,6.80914057906322));
#50148=CARTESIAN_POINT('Ctrl Pts',(15.,23.0236535337006,36.641934691827));
#50149=CARTESIAN_POINT('Ctrl Pts',(15.,-6.80914057906322,29.8327941127638));
#50150=CARTESIAN_POINT('Ctrl Pts',(14.7843073131059,-6.83933995053713,29.9651062042906));
#50151=CARTESIAN_POINT('Ctrl Pts',(14.7843073131059,-36.8044461548278,23.1257662537535));
#50152=CARTESIAN_POINT('Ctrl Pts',(14.7843073131059,-29.9651062042906,-6.83933995053713));
#50153=CARTESIAN_POINT('Ctrl Pts',(14.7843073131059,-23.1257662537535,-36.8044461548278));
#50154=CARTESIAN_POINT('Ctrl Pts',(14.7843073131059,6.83933995053713,-29.9651062042906));
#50155=CARTESIAN_POINT('Ctrl Pts',(14.7843073131059,36.8044461548278,-23.1257662537535));
#50156=CARTESIAN_POINT('Ctrl Pts',(14.7843073131059,29.9651062042906,6.83933995053713));
#50157=CARTESIAN_POINT('Ctrl Pts',(14.7843073131059,23.1257662537535,36.8044461548278));
#50158=CARTESIAN_POINT('Ctrl Pts',(14.7843073131059,-6.83933995053713,29.9651062042906));
#50159=CARTESIAN_POINT('Ctrl Pts',(14.3560298066371,-6.90036423817605,30.2324710777091));
#50160=CARTESIAN_POINT('Ctrl Pts',(14.3560298066371,-37.1328353158852,23.3321068395331));
#50161=CARTESIAN_POINT('Ctrl Pts',(14.3560298066371,-30.2324710777091,-6.90036423817605));
#50162=CARTESIAN_POINT('Ctrl Pts',(14.3560298066371,-23.3321068395331,-37.1328353158852));
#50163=CARTESIAN_POINT('Ctrl Pts',(14.3560298066371,6.90036423817605,-30.2324710777091));
#50164=CARTESIAN_POINT('Ctrl Pts',(14.3560298066371,37.1328353158852,-23.3321068395331));
#50165=CARTESIAN_POINT('Ctrl Pts',(14.3560298066371,30.2324710777091,6.90036423817605));
#50166=CARTESIAN_POINT('Ctrl Pts',(14.3560298066371,23.3321068395331,37.1328353158852));
#50167=CARTESIAN_POINT('Ctrl Pts',(14.3560298066371,-6.90036423817605,30.2324710777091));
#50168=CARTESIAN_POINT('Ctrl Pts',(13.722936818686,-6.9937772372446,30.6417401677374));
#50169=CARTESIAN_POINT('Ctrl Pts',(13.722936818686,-37.635517404982,23.6479629304928));
#50170=CARTESIAN_POINT('Ctrl Pts',(13.722936818686,-30.6417401677374,-6.9937772372446));
#50171=CARTESIAN_POINT('Ctrl Pts',(13.722936818686,-23.6479629304928,-37.635517404982));
#50172=CARTESIAN_POINT('Ctrl Pts',(13.722936818686,6.9937772372446,-30.6417401677374));
#50173=CARTESIAN_POINT('Ctrl Pts',(13.722936818686,37.635517404982,-23.6479629304928));
#50174=CARTESIAN_POINT('Ctrl Pts',(13.722936818686,30.6417401677374,6.9937772372446));
#50175=CARTESIAN_POINT('Ctrl Pts',(13.722936818686,23.6479629304928,37.635517404982));
#50176=CARTESIAN_POINT('Ctrl Pts',(13.722936818686,-6.9937772372446,30.6417401677374));
#50177=CARTESIAN_POINT('Ctrl Pts',(12.8977690042853,-7.12214335873523,31.204148893041));
#50178=CARTESIAN_POINT('Ctrl Pts',(12.8977690042853,-38.3262922517763,24.0820055343058));
#50179=CARTESIAN_POINT('Ctrl Pts',(12.8977690042853,-31.204148893041,-7.12214335873523));
#50180=CARTESIAN_POINT('Ctrl Pts',(12.8977690042853,-24.0820055343058,-38.3262922517763));
#50181=CARTESIAN_POINT('Ctrl Pts',(12.8977690042853,7.12214335873523,-31.204148893041));
#50182=CARTESIAN_POINT('Ctrl Pts',(12.8977690042853,38.3262922517763,-24.0820055343058));
#50183=CARTESIAN_POINT('Ctrl Pts',(12.8977690042853,31.204148893041,7.12214335873523));
#50184=CARTESIAN_POINT('Ctrl Pts',(12.8977690042853,24.0820055343058,38.3262922517763));
#50185=CARTESIAN_POINT('Ctrl Pts',(12.8977690042853,-7.12214335873523,31.204148893041));
#50186=CARTESIAN_POINT('Ctrl Pts',(11.9000549946031,-7.2893932825315,31.9369186874159));
#50187=CARTESIAN_POINT('Ctrl Pts',(11.9000549946031,-39.2263119699474,24.6475254048844));
#50188=CARTESIAN_POINT('Ctrl Pts',(11.9000549946031,-31.9369186874159,-7.2893932825315));
#50189=CARTESIAN_POINT('Ctrl Pts',(11.9000549946031,-24.6475254048844,-39.2263119699474));
#50190=CARTESIAN_POINT('Ctrl Pts',(11.9000549946031,7.2893932825315,-31.9369186874159));
#50191=CARTESIAN_POINT('Ctrl Pts',(11.9000549946031,39.2263119699474,-24.6475254048844));
#50192=CARTESIAN_POINT('Ctrl Pts',(11.9000549946031,31.9369186874159,7.2893932825315));
#50193=CARTESIAN_POINT('Ctrl Pts',(11.9000549946031,24.6475254048844,39.2263119699474));
#50194=CARTESIAN_POINT('Ctrl Pts',(11.9000549946031,-7.2893932825315,31.9369186874159));
#50195=CARTESIAN_POINT('Ctrl Pts',(10.9391333834985,-7.4640486993045,32.702134066474));
#50196=CARTESIAN_POINT('Ctrl Pts',(10.9391333834985,-40.1661827657784,25.2380853671695));
#50197=CARTESIAN_POINT('Ctrl Pts',(10.9391333834985,-32.702134066474,-7.4640486993045));
#50198=CARTESIAN_POINT('Ctrl Pts',(10.9391333834985,-25.2380853671695,-40.1661827657784));
#50199=CARTESIAN_POINT('Ctrl Pts',(10.9391333834985,7.4640486993045,-32.702134066474));
#50200=CARTESIAN_POINT('Ctrl Pts',(10.9391333834985,40.1661827657784,-25.2380853671695));
#50201=CARTESIAN_POINT('Ctrl Pts',(10.9391333834985,32.702134066474,7.4640486993045));
#50202=CARTESIAN_POINT('Ctrl Pts',(10.9391333834985,25.2380853671695,40.1661827657784));
#50203=CARTESIAN_POINT('Ctrl Pts',(10.9391333834985,-7.4640486993045,32.702134066474));
#50204=CARTESIAN_POINT('Ctrl Pts',(10.0180552497783,-7.64672372347922,33.5024856413123));
#50205=CARTESIAN_POINT('Ctrl Pts',(10.0180552497783,-41.1492093647915,25.855761917833));
#50206=CARTESIAN_POINT('Ctrl Pts',(10.0180552497783,-33.5024856413123,-7.64672372347922));
#50207=CARTESIAN_POINT('Ctrl Pts',(10.0180552497783,-25.855761917833,-41.1492093647915));
#50208=CARTESIAN_POINT('Ctrl Pts',(10.0180552497783,7.64672372347922,-33.5024856413123));
#50209=CARTESIAN_POINT('Ctrl Pts',(10.0180552497783,41.1492093647915,-25.855761917833));
#50210=CARTESIAN_POINT('Ctrl Pts',(10.0180552497783,33.5024856413123,7.64672372347922));
#50211=CARTESIAN_POINT('Ctrl Pts',(10.0180552497783,25.855761917833,41.1492093647915));
#50212=CARTESIAN_POINT('Ctrl Pts',(10.0180552497783,-7.64672372347922,33.5024856413123));
#50213=CARTESIAN_POINT('Ctrl Pts',(9.13857394886632,-7.83777126657543,34.339519618326));
#50214=CARTESIAN_POINT('Ctrl Pts',(9.13857394886632,-42.1772908849014,26.5017483517505));
#50215=CARTESIAN_POINT('Ctrl Pts',(9.13857394886632,-34.339519618326,-7.83777126657543));
#50216=CARTESIAN_POINT('Ctrl Pts',(9.13857394886632,-26.5017483517505,-42.1772908849014));
#50217=CARTESIAN_POINT('Ctrl Pts',(9.13857394886632,7.83777126657543,-34.339519618326));
#50218=CARTESIAN_POINT('Ctrl Pts',(9.13857394886632,42.1772908849014,-26.5017483517505));
#50219=CARTESIAN_POINT('Ctrl Pts',(9.13857394886632,34.339519618326,7.83777126657543));
#50220=CARTESIAN_POINT('Ctrl Pts',(9.13857394886632,26.5017483517505,42.1772908849014));
#50221=CARTESIAN_POINT('Ctrl Pts',(9.13857394886632,-7.83777126657543,34.339519618326));
#50222=CARTESIAN_POINT('Ctrl Pts',(8.29915429043693,-8.03688232886511,35.21188218125));
#50223=CARTESIAN_POINT('Ctrl Pts',(8.29915429043693,-43.2487645101151,27.1749998523849));
#50224=CARTESIAN_POINT('Ctrl Pts',(8.29915429043693,-35.21188218125,-8.03688232886511));
#50225=CARTESIAN_POINT('Ctrl Pts',(8.29915429043693,-27.1749998523849,-43.2487645101151));
#50226=CARTESIAN_POINT('Ctrl Pts',(8.29915429043693,8.03688232886511,-35.21188218125));
#50227=CARTESIAN_POINT('Ctrl Pts',(8.29915429043693,43.2487645101151,-27.1749998523849));
#50228=CARTESIAN_POINT('Ctrl Pts',(8.29915429043693,35.21188218125,8.03688232886511));
#50229=CARTESIAN_POINT('Ctrl Pts',(8.29915429043693,27.1749998523849,43.2487645101151));
#50230=CARTESIAN_POINT('Ctrl Pts',(8.29915429043693,-8.03688232886511,35.21188218125));
#50231=CARTESIAN_POINT('Ctrl Pts',(7.4968190344241,-8.24345765802358,36.1169478341035));
#50232=CARTESIAN_POINT('Ctrl Pts',(7.4968190344241,-44.3604054921271,27.8734901760799));
#50233=CARTESIAN_POINT('Ctrl Pts',(7.4968190344241,-36.1169478341035,-8.24345765802358));
#50234=CARTESIAN_POINT('Ctrl Pts',(7.4968190344241,-27.8734901760799,-44.3604054921271));
#50235=CARTESIAN_POINT('Ctrl Pts',(7.4968190344241,8.24345765802358,-36.1169478341035));
#50236=CARTESIAN_POINT('Ctrl Pts',(7.4968190344241,44.3604054921271,-27.8734901760799));
#50237=CARTESIAN_POINT('Ctrl Pts',(7.4968190344241,36.1169478341035,8.24345765802358));
#50238=CARTESIAN_POINT('Ctrl Pts',(7.4968190344241,27.8734901760799,44.3604054921271));
#50239=CARTESIAN_POINT('Ctrl Pts',(7.4968190344241,-8.24345765802358,36.1169478341035));
#50240=CARTESIAN_POINT('Ctrl Pts',(6.88220761950379,-8.41420410800808,36.8650369106509));
#50241=CARTESIAN_POINT('Ctrl Pts',(6.88220761950379,-45.279241018659,28.4508328026428));
#50242=CARTESIAN_POINT('Ctrl Pts',(6.88220761950379,-36.8650369106509,-8.41420410800808));
#50243=CARTESIAN_POINT('Ctrl Pts',(6.88220761950379,-28.4508328026428,-45.279241018659));
#50244=CARTESIAN_POINT('Ctrl Pts',(6.88220761950379,8.41420410800808,-36.8650369106509));
#50245=CARTESIAN_POINT('Ctrl Pts',(6.88220761950379,45.279241018659,-28.4508328026428));
#50246=CARTESIAN_POINT('Ctrl Pts',(6.88220761950379,36.8650369106509,8.41420410800808));
#50247=CARTESIAN_POINT('Ctrl Pts',(6.88220761950379,28.4508328026428,45.279241018659));
#50248=CARTESIAN_POINT('Ctrl Pts',(6.88220761950379,-8.41420410800808,36.8650369106509));
#50249=CARTESIAN_POINT('Ctrl Pts',(6.43560997955544,-8.54515448010585,37.4387679776515));
#50250=CARTESIAN_POINT('Ctrl Pts',(6.43560997955544,-45.9839224577573,28.8936134975456));
#50251=CARTESIAN_POINT('Ctrl Pts',(6.43560997955544,-37.4387679776515,-8.54515448010585));
#50252=CARTESIAN_POINT('Ctrl Pts',(6.43560997955544,-28.8936134975456,-45.9839224577573));
#50253=CARTESIAN_POINT('Ctrl Pts',(6.43560997955544,8.54515448010585,-37.4387679776515));
#50254=CARTESIAN_POINT('Ctrl Pts',(6.43560997955544,45.9839224577573,-28.8936134975456));
#50255=CARTESIAN_POINT('Ctrl Pts',(6.43560997955544,37.4387679776515,8.54515448010585));
#50256=CARTESIAN_POINT('Ctrl Pts',(6.43560997955544,28.8936134975456,45.9839224577573));
#50257=CARTESIAN_POINT('Ctrl Pts',(6.43560997955544,-8.54515448010585,37.4387679776515));
#50258=CARTESIAN_POINT('Ctrl Pts',(6.14415685965718,-8.63371847902026,37.8267922098931));
#50259=CARTESIAN_POINT('Ctrl Pts',(6.14415685965718,-46.4605106889134,29.1930737308729));
#50260=CARTESIAN_POINT('Ctrl Pts',(6.14415685965718,-37.8267922098931,-8.63371847902026));
#50261=CARTESIAN_POINT('Ctrl Pts',(6.14415685965718,-29.1930737308729,-46.4605106889134));
#50262=CARTESIAN_POINT('Ctrl Pts',(6.14415685965718,8.63371847902026,-37.8267922098931));
#50263=CARTESIAN_POINT('Ctrl Pts',(6.14415685965718,46.4605106889134,-29.1930737308729));
#50264=CARTESIAN_POINT('Ctrl Pts',(6.14415685965718,37.8267922098931,8.63371847902026));
#50265=CARTESIAN_POINT('Ctrl Pts',(6.14415685965718,29.1930737308729,46.4605106889134));
#50266=CARTESIAN_POINT('Ctrl Pts',(6.14415685965718,-8.63371847902026,37.8267922098931));
#50267=CARTESIAN_POINT('Ctrl Pts',(6.,-8.67831642429626,38.0221885750911));
#50268=CARTESIAN_POINT('Ctrl Pts',(6.,-46.7005049993874,29.3438721507949));
#50269=CARTESIAN_POINT('Ctrl Pts',(6.,-38.0221885750911,-8.67831642429626));
#50270=CARTESIAN_POINT('Ctrl Pts',(6.,-29.3438721507949,-46.7005049993874));
#50271=CARTESIAN_POINT('Ctrl Pts',(6.,8.67831642429626,-38.0221885750911));
#50272=CARTESIAN_POINT('Ctrl Pts',(6.,46.7005049993874,-29.3438721507949));
#50273=CARTESIAN_POINT('Ctrl Pts',(6.,38.0221885750911,8.67831642429626));
#50274=CARTESIAN_POINT('Ctrl Pts',(6.,29.3438721507949,46.7005049993874));
#50275=CARTESIAN_POINT('Ctrl Pts',(6.,-8.67831642429626,38.0221885750911));
#50276=CARTESIAN_POINT('Ctrl Pts',(15.,-12.9907743917407,27.7055911451623));
#50277=CARTESIAN_POINT('Ctrl Pts',(14.0108432136945,-14.6088239471801,27.6343116779264));
#50278=CARTESIAN_POINT('Ctrl Pts',(13.3692319443824,-15.6575970987913,27.5323911990493));
#50279=CARTESIAN_POINT('Ctrl Pts',(12.3476991724842,-16.9912047967252,27.6207265630898));
#50280=CARTESIAN_POINT('Ctrl Pts',(12.0250187050191,-17.4124630932992,27.6486298250765));
#50281=CARTESIAN_POINT('Ctrl Pts',(11.6666317570709,-17.879669743489,27.6853416006481));
#50282=CARTESIAN_POINT('Ctrl Pts',(11.3593868751765,-18.2696172606052,27.731107727427));
#50283=CARTESIAN_POINT('Ctrl Pts',(10.6767716809131,-19.1359753867601,27.8327877076734));
#50284=CARTESIAN_POINT('Ctrl Pts',(10.1321636914396,-19.7808016313084,27.9765529194963));
#50285=CARTESIAN_POINT('Ctrl Pts',(9.56604173138328,-20.367391588899,28.2355867335771));
#50286=CARTESIAN_POINT('Ctrl Pts',(9.34563078589188,-20.5957714368658,28.3364375959427));
#50287=CARTESIAN_POINT('Ctrl Pts',(9.12222951098698,-20.8150365124456,28.4553629135261));
#50288=CARTESIAN_POINT('Ctrl Pts',(8.88860711505283,-21.0375201114275,28.595321354551));
#50289=CARTESIAN_POINT('Ctrl Pts',(8.75830600700746,-21.1616086404974,28.6733821067016));
#50290=CARTESIAN_POINT('Ctrl Pts',(8.62340343546554,-21.2885664898727,28.7567233832714));
#50291=CARTESIAN_POINT('Ctrl Pts',(8.40819516300422,-21.4870679866862,28.9038265799739));
#50292=CARTESIAN_POINT('Ctrl Pts',(8.02443006829132,-21.8410411163157,29.166144898733));
#50293=CARTESIAN_POINT('Ctrl Pts',(7.46417034513343,-22.3418347305613,29.5947644941187));
#50294=CARTESIAN_POINT('Ctrl Pts',(6.85957019142019,-22.899994357402,30.1414924867737));
#50295=CARTESIAN_POINT('Ctrl Pts',(6.58024553736738,-23.1578635354298,30.3940802614732));
#50296=CARTESIAN_POINT('Ctrl Pts',(6.28976782192773,-23.4111866254207,30.6864026200108));
#50297=CARTESIAN_POINT('Ctrl Pts',(6.,-23.6628748086085,31.0011024931715));
#50298=CARTESIAN_POINT('Ctrl Pts',(2.09999999999999,-9.1358389695905,12.8994676435885));
#50299=CARTESIAN_POINT('Ctrl Pts',(2.73333333333333,-9.1358389695905,12.8994676435885));
#50300=CARTESIAN_POINT('Ctrl Pts',(3.36803396034652,-9.13587946857483,12.8994427611867));
#50301=CARTESIAN_POINT('Ctrl Pts',(4.25277026443832,-9.13590413998491,12.8994267516404));
#50302=CARTESIAN_POINT('Ctrl Pts',(4.77266782207174,-9.14283195334969,12.8946326691098));
#50303=CARTESIAN_POINT('Ctrl Pts',(5.76856815409261,-9.16295171178049,12.8807712941876));
#50304=CARTESIAN_POINT('Ctrl Pts',(6.48508324968699,-9.16244277980798,12.8811872446167));
#50305=CARTESIAN_POINT('Ctrl Pts',(6.99866103340899,-9.13441989422394,12.9002632404603));
#50306=CARTESIAN_POINT('Ctrl Pts',(7.1248003053003,-9.12737999976702,12.9051906488153));
#50307=CARTESIAN_POINT('Ctrl Pts',(7.37170307579371,-9.11265400996954,12.9157079837048));
#50308=CARTESIAN_POINT('Ctrl Pts',(7.68211097020559,-9.09212039919145,12.9306851681623));
#50309=CARTESIAN_POINT('Ctrl Pts',(8.05073856781673,-9.06328234581171,12.9517504216116));
#50310=CARTESIAN_POINT('Ctrl Pts',(8.41503776200927,-9.02932619481544,12.9761948589261));
#50311=CARTESIAN_POINT('Ctrl Pts',(9.01074580667397,-8.96260310536268,13.0230672198542));
#50312=CARTESIAN_POINT('Ctrl Pts',(9.46309579122147,-8.89115997747123,13.0707089963125));
#50313=CARTESIAN_POINT('Ctrl Pts',(10.2678466003299,-8.72074990849221,13.1778321896751));
#50314=CARTESIAN_POINT('Ctrl Pts',(10.9804913088774,-8.50902906615356,13.3180193104141));
#50315=CARTESIAN_POINT('Ctrl Pts',(11.7910235970548,-8.19504180806732,13.5142059637011));
#50316=CARTESIAN_POINT('Ctrl Pts',(12.2471523736939,-8.00233437587927,13.6282924769383));
#50317=CARTESIAN_POINT('Ctrl Pts',(12.473248541207,-7.90241242624034,13.6848508114561));
#50318=CARTESIAN_POINT('Ctrl Pts',(12.835119440223,-7.73968708601252,13.7743470979446));
#50319=CARTESIAN_POINT('Ctrl Pts',(13.2802515759032,-7.51846451475199,13.893886306531));
#50320=CARTESIAN_POINT('Ctrl Pts',(14.1612566771783,-7.01278962913115,14.1598111690564));
#50321=CARTESIAN_POINT('Ctrl Pts',(14.7820737708942,-6.58952040585146,14.3641290043432));
#50322=CARTESIAN_POINT('Ctrl Pts',(15.1979896574214,-6.293157281203,14.4912418342554));
#50323=CARTESIAN_POINT('Ctrl Pts',(2.09999999999999,-13.9592433656065,18.9478254487004));
#50324=CARTESIAN_POINT('Ctrl Pts',(2.73333333333333,-13.9592433656065,18.9478254487004));
#50325=CARTESIAN_POINT('Ctrl Pts',(3.36872001028818,-13.9592430229431,18.9478231191763));
#50326=CARTESIAN_POINT('Ctrl Pts',(4.25415479043436,-13.9592533149426,18.9478139437242));
#50327=CARTESIAN_POINT('Ctrl Pts',(4.7830977821647,-13.9694950763228,18.9404364496675));
#50328=CARTESIAN_POINT('Ctrl Pts',(5.77493725537989,-13.9990220924234,18.9192694384421));
#50329=CARTESIAN_POINT('Ctrl Pts',(6.4749679303508,-13.9978840640735,18.9201673597862));
#50330=CARTESIAN_POINT('Ctrl Pts',(6.96726949180708,-13.9578216279669,18.9485487239907));
#50331=CARTESIAN_POINT('Ctrl Pts',(7.09308743961926,-13.9474986367052,18.9560665046118));
#50332=CARTESIAN_POINT('Ctrl Pts',(7.33628686896228,-13.9260840480499,18.9719842439271));
#50333=CARTESIAN_POINT('Ctrl Pts',(7.64236232313703,-13.8961937138069,18.9946711654445));
#50334=CARTESIAN_POINT('Ctrl Pts',(8.00391772282853,-13.8543929989952,19.0264634303694));
#50335=CARTESIAN_POINT('Ctrl Pts',(8.36001086452926,-13.8052361360177,19.0633119060548));
#50336=CARTESIAN_POINT('Ctrl Pts',(8.93967782036849,-13.7090318701985,19.1337290363374));
#50337=CARTESIAN_POINT('Ctrl Pts',(9.37529315599633,-13.6063093912297,19.2050998156635));
#50338=CARTESIAN_POINT('Ctrl Pts',(10.1434001221335,-13.3632536306442,19.3644588529799));
#50339=CARTESIAN_POINT('Ctrl Pts',(10.834292561854,-13.0595924539228,19.5747599519676));
#50340=CARTESIAN_POINT('Ctrl Pts',(11.6346804009544,-12.6027392234137,19.8736981509546));
#50341=CARTESIAN_POINT('Ctrl Pts',(12.0872541836183,-12.3210927384552,20.0484111755836));
#50342=CARTESIAN_POINT('Ctrl Pts',(12.312245937423,-12.1746196452708,20.1353385324134));
#50343=CARTESIAN_POINT('Ctrl Pts',(12.6725852131256,-11.9358582362001,20.2730855006835));
#50344=CARTESIAN_POINT('Ctrl Pts',(13.111014081714,-11.6142751048964,20.4560476897286));
#50345=CARTESIAN_POINT('Ctrl Pts',(13.9921333654529,-10.8715316570354,20.8675199651784));
#50346=CARTESIAN_POINT('Ctrl Pts',(14.6125773377935,-10.2465061114962,21.1857635085628));
#50347=CARTESIAN_POINT('Ctrl Pts',(15.0291266285127,-9.80896819642242,21.3843214467584));
#50348=CARTESIAN_POINT('Ctrl Pts',(2.09999999999999,-18.7826477616224,24.9961832538124));
#50349=CARTESIAN_POINT('Ctrl Pts',(2.73333333333333,-18.7826477616224,24.9961832538124));
#50350=CARTESIAN_POINT('Ctrl Pts',(3.36945492966225,-18.7826777179121,24.9961656007647));
#50351=CARTESIAN_POINT('Ctrl Pts',(4.2556188098197,-18.7827110508831,24.9961424923783));
#50352=CARTESIAN_POINT('Ctrl Pts',(4.79358899047167,-18.7964412840621,24.9860521050349));
#50353=CARTESIAN_POINT('Ctrl Pts',(5.78146281943922,-18.8353472835957,24.9576044685868));
#50354=CARTESIAN_POINT('Ctrl Pts',(6.46486945359605,-18.8332967951376,24.959240722034));
#50355=CARTESIAN_POINT('Ctrl Pts',(6.93654950905192,-18.7828433682711,24.9956280758371));
#50356=CARTESIAN_POINT('Ctrl Pts',(7.06206135947415,-18.769269337643,25.0057124981866));
#50357=CARTESIAN_POINT('Ctrl Pts',(7.30169240156151,-18.7414755139896,25.0267879160898));
#50358=CARTESIAN_POINT('Ctrl Pts',(7.60367117597197,-18.7026852581207,25.0568363852838));
#50359=CARTESIAN_POINT('Ctrl Pts',(7.95860842859181,-18.6486868578601,25.0987594126722));
#50360=CARTESIAN_POINT('Ctrl Pts',(8.30731707317219,-18.5854728780161,25.1471442340964));
#50361=CARTESIAN_POINT('Ctrl Pts',(8.87310871284282,-18.4621240372099,25.2393106240003));
#50362=CARTESIAN_POINT('Ctrl Pts',(9.29618834699587,-18.3316544025768,25.3318189029734));
#50363=CARTESIAN_POINT('Ctrl Pts',(10.0462774324726,-18.0231260796766,25.5383575274243));
#50364=CARTESIAN_POINT('Ctrl Pts',(10.7405209602188,-17.6279994974315,25.8191221563898));
#50365=CARTESIAN_POINT('Ctrl Pts',(11.5482282528203,-17.0233084556598,26.2247579066847));
#50366=CARTESIAN_POINT('Ctrl Pts',(12.0041830503694,-16.6504133177635,26.461851751404));
#50367=CARTESIAN_POINT('Ctrl Pts',(12.2304159734591,-16.456510112927,26.579819767925));
#50368=CARTESIAN_POINT('Ctrl Pts',(12.5924547381801,-16.1405885621055,26.76669275901));
#50369=CARTESIAN_POINT('Ctrl Pts',(13.0427800388235,-15.7088357620631,27.0194118197174));
#50370=CARTESIAN_POINT('Ctrl Pts',(13.9385905427776,-14.7126468494779,27.5853829514202));
#50371=CARTESIAN_POINT('Ctrl Pts',(14.5670688438605,-13.8775476356544,28.0209529954987));
#50372=CARTESIAN_POINT('Ctrl Pts',(14.9853697475044,-13.2962000699107,28.2913742942891));
#50373=CARTESIAN_POINT('Ctrl Pts',(2.09999999999999,-23.6060521576384,31.0445410589243));
#50374=CARTESIAN_POINT('Ctrl Pts',(2.73333333333333,-23.6060521576384,31.0445410589243));
#50375=CARTESIAN_POINT('Ctrl Pts',(3.37020567578152,-23.6061012377393,31.0445167170057));
#50376=CARTESIAN_POINT('Ctrl Pts',(4.25712263390388,-23.6061528913754,31.0444834021622));
#50377=CARTESIAN_POINT('Ctrl Pts',(4.80402631037446,-23.6235140941777,31.0315658657309));
#50378=CARTESIAN_POINT('Ctrl Pts',(5.78813882280503,-23.6717259268289,30.9958965701794));
#50379=CARTESIAN_POINT('Ctrl Pts',(6.45445717224562,-23.6684510662632,30.9985176925269));
#50380=CARTESIAN_POINT('Ctrl Pts',(6.90691329160007,-23.6089092172418,31.0418757119288));
#50381=CARTESIAN_POINT('Ctrl Pts',(7.03214913606668,-23.5921060187484,31.0545103301399));
#50382=CARTESIAN_POINT('Ctrl Pts',(7.26849953702799,-23.5581710572885,31.0805561729954));
#50383=CARTESIAN_POINT('Ctrl Pts',(7.56683838895087,-23.5107754859076,31.1177364790289));
#50384=CARTESIAN_POINT('Ctrl Pts',(7.91605485564789,-23.4450675478998,31.1694113667199));
#50385=CARTESIAN_POINT('Ctrl Pts',(8.25885085470307,-23.3683245653721,31.2289290660225));
#50386=CARTESIAN_POINT('Ctrl Pts',(8.81427676356264,-23.2186216887375,31.3422506346006));
#50387=CARTESIAN_POINT('Ctrl Pts',(9.230541336078,-23.0603721928338,31.4559695174958));
#50388=CARTESIAN_POINT('Ctrl Pts',(9.97650378825299,-22.6805359674084,31.7141346440069));
#50389=CARTESIAN_POINT('Ctrl Pts',(10.6790242999544,-22.1835991752983,32.0727916994504));
#50390=CARTESIAN_POINT('Ctrl Pts',(11.4920909027962,-21.4251096839784,32.5885394149958));
#50391=CARTESIAN_POINT('Ctrl Pts',(11.9504434973868,-20.9585878216415,32.8891746503978));
#50392=CARTESIAN_POINT('Ctrl Pts',(12.1774732934021,-20.7164781036866,33.0384524243975));
#50393=CARTESIAN_POINT('Ctrl Pts',(12.5406734120574,-20.3222914406926,33.2747866829337));
#50394=CARTESIAN_POINT('Ctrl Pts',(12.997674080036,-19.7755003700753,33.5996747028483));
#50395=CARTESIAN_POINT('Ctrl Pts',(13.8994000182975,-18.5241058978638,34.319599884084));
#50396=CARTESIAN_POINT('Ctrl Pts',(14.5324532885843,-17.4781380681113,34.8718039257929));
#50397=CARTESIAN_POINT('Ctrl Pts',(14.9514110803021,-16.7529034957905,35.2133535056034));
#50398=CARTESIAN_POINT('',(3.2,-22.7328514723457,29.9495820327474));
#50399=CARTESIAN_POINT('Ctrl Pts',(3.2,-22.7328514723457,29.9495820327475));
#50400=CARTESIAN_POINT('Ctrl Pts',(3.56152274835438,-22.0367096350838,29.0766477794334));
#50401=CARTESIAN_POINT('Ctrl Pts',(3.9522458452542,-21.3272055238567,28.1962618480736));
#50402=CARTESIAN_POINT('Ctrl Pts',(4.78767430123817,-19.9404633926114,26.4217559391896));
#50403=CARTESIAN_POINT('Ctrl Pts',(5.21513946232189,-19.2889122016819,25.5627262762193));
#50404=CARTESIAN_POINT('Ctrl Pts',(6.79548775402795,-16.9877013184703,22.6232620424128));
#50405=CARTESIAN_POINT('Ctrl Pts',(7.94016295939784,-15.4537789500188,21.0097851802331));
#50406=CARTESIAN_POINT('Ctrl Pts',(9.46271935276271,-13.4835985568963,19.0493119701759));
#50407=CARTESIAN_POINT('Ctrl Pts',(10.1385443659171,-12.606358882668,18.3124599798231));
#50408=CARTESIAN_POINT('Ctrl Pts',(11.5967860400763,-10.6794699511535,16.973113867352));
#50409=CARTESIAN_POINT('Ctrl Pts',(12.3997356677094,-9.65410050721625,16.2944337889661));
#50410=CARTESIAN_POINT('Ctrl Pts',(13.6850585208088,-8.0445312444617,15.3094152086593));
#50411=CARTESIAN_POINT('Ctrl Pts',(14.3457395898605,-7.20959578890565,14.8600025739989));
#50412=CARTESIAN_POINT('Ctrl Pts',(15.,-6.43313341740755,14.4300655106231));
#50413=CARTESIAN_POINT('Ctrl Pts',(2.7981505262301,-23.3193787656373,30.685034966607));
#50414=CARTESIAN_POINT('Ctrl Pts',(2.93286079301997,-23.1239442315795,30.439958005238));
#50415=CARTESIAN_POINT('Ctrl Pts',(3.06772862158681,-22.9283859253528,30.1947241748125));
#50416=CARTESIAN_POINT('Ctrl Pts',(3.20258097292904,-22.7328862936894,29.94956342958));
#50417=CARTESIAN_POINT('Origin',(2.9,0.,0.));
#50418=CARTESIAN_POINT('',(3.2,-9.24182505978395,36.4465179346992));
#50419=CARTESIAN_POINT('Origin',(3.2,0.,0.));
#50420=CARTESIAN_POINT('Ctrl Pts',(3.19857330932923,-9.24172635305947,36.4465202813748));
#50421=CARTESIAN_POINT('Ctrl Pts',(3.06444826166183,-9.31155448788265,36.7523757023571));
#50422=CARTESIAN_POINT('Ctrl Pts',(2.93032536154112,-9.38136974531151,37.0581756374017));
#50423=CARTESIAN_POINT('Ctrl Pts',(2.79631258706843,-9.45110215575605,37.3636243084515));
#50424=CARTESIAN_POINT('Ctrl Pts',(2.1,2.6347947165568,15.5883531961151));
#50425=CARTESIAN_POINT('Ctrl Pts',(2.73333333333333,2.6347947165568,15.5883531961151));
#50426=CARTESIAN_POINT('Ctrl Pts',(3.36597092855911,2.63487877694595,15.5883248523788));
#50427=CARTESIAN_POINT('Ctrl Pts',(4.12348287006708,2.63490452868168,15.5883160613212));
#50428=CARTESIAN_POINT('Ctrl Pts',(4.36307655407023,2.63298541566169,15.5886609732488));
#50429=CARTESIAN_POINT('Ctrl Pts',(4.85756224330648,2.62413456290923,15.5902643440359));
#50430=CARTESIAN_POINT('Ctrl Pts',(5.73898260168751,2.60307954294172,15.5940979332686));
#50431=CARTESIAN_POINT('Ctrl Pts',(6.52604985398505,2.60248787292251,15.5942198385231));
#50432=CARTESIAN_POINT('Ctrl Pts',(7.12756040848415,2.64154082328796,15.5869612993371));
#50433=CARTESIAN_POINT('Ctrl Pts',(7.25505573466752,2.65010896186311,15.5854615937326));
#50434=CARTESIAN_POINT('Ctrl Pts',(7.51731445119969,2.66907640732711,15.5823205204395));
#50435=CARTESIAN_POINT('Ctrl Pts',(7.84588191847868,2.69580726019365,15.5781391720899));
#50436=CARTESIAN_POINT('Ctrl Pts',(8.24416069925083,2.7339827985819,15.5721834308337));
#50437=CARTESIAN_POINT('Ctrl Pts',(8.77646064332894,2.7945696858706,15.5622777615526));
#50438=CARTESIAN_POINT('Ctrl Pts',(9.44113113319551,2.89127679751306,15.5449472038089));
#50439=CARTESIAN_POINT('Ctrl Pts',(9.96388158672623,2.99801240629933,15.5227349400434));
#50440=CARTESIAN_POINT('Ctrl Pts',(11.1189097708078,3.27995384619542,15.4595842505362));
#50441=CARTESIAN_POINT('Ctrl Pts',(12.0804504807078,3.67510301631977,15.378715156088));
#50442=CARTESIAN_POINT('Ctrl Pts',(13.0008381113228,4.11170193500177,15.2621541211597));
#50443=CARTESIAN_POINT('Ctrl Pts',(13.2108148630541,4.21340285849752,15.2334087107959));
#50444=CARTESIAN_POINT('Ctrl Pts',(13.3144380484095,4.26396100854989,15.218663366468));
#50445=CARTESIAN_POINT('Ctrl Pts',(13.3733179522989,4.2927766528207,15.2101247620612));
#50446=CARTESIAN_POINT('Ctrl Pts',(13.4025971758006,4.3071312344584,15.2058253366162));
#50447=CARTESIAN_POINT('Ctrl Pts',(13.6877891557158,4.44705188898038,15.1636603735762));
#50448=CARTESIAN_POINT('Ctrl Pts',(14.2465840714085,4.74847969800923,15.0703686144057));
#50449=CARTESIAN_POINT('Ctrl Pts',(14.7537307590314,5.06401626322089,14.9659520583603));
#50450=CARTESIAN_POINT('Ctrl Pts',(14.9999999999997,5.22423077688621,14.9103792371774));
#50451=CARTESIAN_POINT('Ctrl Pts',(2.1,4.35606337899725,23.1297239496034));
#50452=CARTESIAN_POINT('Ctrl Pts',(2.73333333333333,4.35606337899725,23.1297239496034));
#50453=CARTESIAN_POINT('Ctrl Pts',(3.36558543190671,4.35612716337005,23.1297057293561));
#50454=CARTESIAN_POINT('Ctrl Pts',(4.12268142832915,4.35614521108889,23.1297004979493));
#50455=CARTESIAN_POINT('Ctrl Pts',(4.3569949475632,4.35333162406734,23.1302630191334));
#50456=CARTESIAN_POINT('Ctrl Pts',(4.84799859005213,4.34026118051108,23.1328902028501));
#50457=CARTESIAN_POINT('Ctrl Pts',(5.73068431571993,4.30898508319672,23.1391950484359));
#50458=CARTESIAN_POINT('Ctrl Pts',(6.53594452799194,4.30765093285249,23.1394978970553));
#50459=CARTESIAN_POINT('Ctrl Pts',(7.15869704281812,4.36693709747872,23.1273835845108));
#50460=CARTESIAN_POINT('Ctrl Pts',(7.28652199655925,4.37967250394112,23.1249084995651));
#50461=CARTESIAN_POINT('Ctrl Pts',(7.55248595534259,4.40807408785084,23.1196613579342));
#50462=CARTESIAN_POINT('Ctrl Pts',(7.88541191425088,4.44806281423684,23.1126458361116));
#50463=CARTESIAN_POINT('Ctrl Pts',(8.29076639755633,4.50536019693898,23.1026065558361));
#50464=CARTESIAN_POINT('Ctrl Pts',(8.83403708716025,4.59642126151075,23.0859814745868));
#50465=CARTESIAN_POINT('Ctrl Pts',(9.51598213434279,4.74226276135199,23.0570627188072));
#50466=CARTESIAN_POINT('Ctrl Pts',(10.0563030846795,4.9039414957736,23.0203780338792));
#50467=CARTESIAN_POINT('Ctrl Pts',(11.2545308253523,5.33249726135678,22.9164305886563));
#50468=CARTESIAN_POINT('Ctrl Pts',(12.2341926884871,5.92719043165041,22.7829833102729));
#50469=CARTESIAN_POINT('Ctrl Pts',(13.1607878864896,6.5769705088875,22.5957624671674));
#50470=CARTESIAN_POINT('Ctrl Pts',(13.3718883884894,6.72817198515924,22.5497929772012));
#50471=CARTESIAN_POINT('Ctrl Pts',(13.4759366022101,6.80326365911736,22.5262671163551));
#50472=CARTESIAN_POINT('Ctrl Pts',(13.5350403600778,6.84604972260816,22.5126594542453));
#50473=CARTESIAN_POINT('Ctrl Pts',(13.5644102208465,6.86735671317708,22.5058120913436));
#50474=CARTESIAN_POINT('Ctrl Pts',(13.850899789237,7.0750356041283,22.4387270236514));
#50475=CARTESIAN_POINT('Ctrl Pts',(14.4159087057268,7.52542850338841,22.2899969175317));
#50476=CARTESIAN_POINT('Ctrl Pts',(14.9236315787721,7.99260139788206,22.1252578594855));
#50477=CARTESIAN_POINT('Ctrl Pts',(15.169681381964,8.22967258714631,22.0377861434561));
#50478=CARTESIAN_POINT('Ctrl Pts',(2.1,6.0773320414377,30.6710947030918));
#50479=CARTESIAN_POINT('Ctrl Pts',(2.73333333333333,6.0773320414377,30.6710947030918));
#50480=CARTESIAN_POINT('Ctrl Pts',(3.36511575592128,6.07744159234164,30.6710578689652));
#50481=CARTESIAN_POINT('Ctrl Pts',(4.12177085956525,6.07747238314756,30.6710471580155));
#50482=CARTESIAN_POINT('Ctrl Pts',(4.35079193747223,6.0738258616781,30.6718120759031));
#50483=CARTESIAN_POINT('Ctrl Pts',(4.83832804865265,6.05666008100118,30.6754320523652));
#50484=CARTESIAN_POINT('Ctrl Pts',(5.72216713207848,6.01515261534281,30.6842063322053));
#50485=CARTESIAN_POINT('Ctrl Pts',(6.5457137878836,6.01267406596902,30.6847605261392));
#50486=CARTESIAN_POINT('Ctrl Pts',(7.18903047452237,6.09423426265411,30.6673127811817));
#50487=CARTESIAN_POINT('Ctrl Pts',(7.31716860740305,6.11117475734039,30.6638523057514));
#50488=CARTESIAN_POINT('Ctrl Pts',(7.58670048132759,6.14939432722339,30.6564081566631));
#50489=CARTESIAN_POINT('Ctrl Pts',(7.92373137203068,6.20318983887758,30.6464213526081));
#50490=CARTESIAN_POINT('Ctrl Pts',(8.33570341698837,6.2805651510717,30.6320677369574));
#50491=CARTESIAN_POINT('Ctrl Pts',(8.88881689288255,6.40391068085729,30.608268282651));
#50492=CARTESIAN_POINT('Ctrl Pts',(9.58536674245199,6.60229784679161,30.5668946362938));
#50493=CARTESIAN_POINT('Ctrl Pts',(10.1375545224602,6.82322181666221,30.5145715779978));
#50494=CARTESIAN_POINT('Ctrl Pts',(11.3565317171601,7.40826014599771,30.3669503054083));
#50495=CARTESIAN_POINT('Ctrl Pts',(12.3228165107166,8.19747637375704,30.1814726492943));
#50496=CARTESIAN_POINT('Ctrl Pts',(13.243836087323,9.05463748545945,29.9251367893499));
#50497=CARTESIAN_POINT('Ctrl Pts',(13.4536824685161,9.25433833928729,29.862197970734));
#50498=CARTESIAN_POINT('Ctrl Pts',(13.5572461322348,9.35350089827159,29.8300142987523));
#50499=CARTESIAN_POINT('Ctrl Pts',(13.6160854542733,9.41001813369078,29.8113998859174));
#50500=CARTESIAN_POINT('Ctrl Pts',(13.6453425809554,9.43816529738583,29.8020343960706));
#50501=CARTESIAN_POINT('Ctrl Pts',(13.9304319363095,9.71252849392874,29.710286783206));
#50502=CARTESIAN_POINT('Ctrl Pts',(14.4834738667375,10.3003159989071,29.5100957209417));
#50503=CARTESIAN_POINT('Ctrl Pts',(14.98335392639,10.9107138228419,29.288560902014));
#50504=CARTESIAN_POINT('Ctrl Pts',(15.2260186760796,11.2206073397433,29.1710541261593));
#50505=CARTESIAN_POINT('Ctrl Pts',(2.1,7.79860070387815,38.2124654565801));
#50506=CARTESIAN_POINT('Ctrl Pts',(2.73333333333333,7.79860070387815,38.2124654565801));
#50507=CARTESIAN_POINT('Ctrl Pts',(3.36463751436128,7.79872338061474,38.2124179470539));
#50508=CARTESIAN_POINT('Ctrl Pts',(4.12085370601274,7.79875679292426,38.2124042468681));
#50509=CARTESIAN_POINT('Ctrl Pts',(4.34456960184645,7.79432734686382,38.2133601111439));
#50510=CARTESIAN_POINT('Ctrl Pts',(4.82871214417148,7.77317894546784,38.2179475900756));
#50511=CARTESIAN_POINT('Ctrl Pts',(5.71350064499196,7.72135905324094,38.2292093593782));
#50512=CARTESIAN_POINT('Ctrl Pts',(6.55583686528122,7.71731376425226,38.2301136297106));
#50513=CARTESIAN_POINT('Ctrl Pts',(7.21832683560861,7.82275706013742,38.2069626157521));
#50514=CARTESIAN_POINT('Ctrl Pts',(7.3467488661425,7.84392828956102,38.2025101244878));
#50515=CARTESIAN_POINT('Ctrl Pts',(7.61956039329437,7.89225983243226,38.1927997302842));
#50516=CARTESIAN_POINT('Ctrl Pts',(7.96024872021727,7.96021416603579,38.1797574416493));
#50517=CARTESIAN_POINT('Ctrl Pts',(8.37793113671827,8.05826993943243,38.1609432159692));
#50518=CARTESIAN_POINT('Ctrl Pts',(8.93896644082855,8.21472997667767,38.1297626383333));
#50519=CARTESIAN_POINT('Ctrl Pts',(9.6458827308017,8.46659482431919,38.0756832340632));
#50520=CARTESIAN_POINT('Ctrl Pts',(10.2035693459978,8.745644125101,38.0079664066119));
#50521=CARTESIAN_POINT('Ctrl Pts',(11.4269635730292,9.47832897311608,37.8188801486782));
#50522=CARTESIAN_POINT('Ctrl Pts',(12.3794496835402,10.4472805414767,37.5858346075197));
#50523=CARTESIAN_POINT('Ctrl Pts',(13.297269717393,11.5084412735018,37.2622699611218));
#50524=CARTESIAN_POINT('Ctrl Pts',(13.5062391671476,11.7558332723801,37.1827925479603));
#50525=CARTESIAN_POINT('Ctrl Pts',(13.609511794127,11.8787985987299,37.1421314651239));
#50526=CARTESIAN_POINT('Ctrl Pts',(13.668184860874,11.9488983329783,37.1186112363832));
#50527=CARTESIAN_POINT('Ctrl Pts',(13.6973773248548,11.9838264461449,37.106773618565));
#50528=CARTESIAN_POINT('Ctrl Pts',(13.9814744041932,12.3240718432943,36.9908828203732));
#50529=CARTESIAN_POINT('Ctrl Pts',(14.5280894908559,13.0445097705752,36.7414946448057));
#50530=CARTESIAN_POINT('Ctrl Pts',(15.0243070371674,13.797534545931,36.464130441338));
#50531=CARTESIAN_POINT('Ctrl Pts',(15.2656150130537,14.1802216087483,36.3169760702825));
#50532=CARTESIAN_POINT('',(3.2,7.48695481785667,36.8470556158206));
#50533=CARTESIAN_POINT('Ctrl Pts',(3.19847028779066,7.48703421002627,36.8470253949768));
#50534=CARTESIAN_POINT('Ctrl Pts',(3.06436324509112,7.55683027125151,37.1528880888971));
#50535=CARTESIAN_POINT('Ctrl Pts',(2.93025906836479,7.6266128911633,37.4586939150269));
#50536=CARTESIAN_POINT('Ctrl Pts',(2.79626331616334,7.69631666193415,37.7641461193963));
#50537=CARTESIAN_POINT('',(15.,5.22423077689144,14.9103792371898));
#50538=CARTESIAN_POINT('Ctrl Pts',(15.,5.22423077689144,14.9103792371898));
#50539=CARTESIAN_POINT('Ctrl Pts',(14.4897165779514,5.09999693117215,15.5397159770542));
#50540=CARTESIAN_POINT('Ctrl Pts',(13.9833803026614,4.98878064338043,16.1885993141875));
#50541=CARTESIAN_POINT('Ctrl Pts',(13.4460287676664,4.9079979567178,16.9049907761367));
#50542=CARTESIAN_POINT('Ctrl Pts',(12.8282655681041,4.81512659089501,17.728586230604));
#50543=CARTESIAN_POINT('Ctrl Pts',(12.155541408949,4.70804591508919,18.6860507311911));
#50544=CARTESIAN_POINT('Ctrl Pts',(11.5904908073611,4.65658883211823,19.5292784359842));
#50545=CARTESIAN_POINT('Ctrl Pts',(11.1143368259633,4.61322723784883,20.2398452909418));
#50546=CARTESIAN_POINT('Ctrl Pts',(10.6953158949599,4.60176573657917,20.8918050007962));
#50547=CARTESIAN_POINT('Ctrl Pts',(10.2957959918397,4.62202135570262,21.5329760085416));
#50548=CARTESIAN_POINT('Ctrl Pts',(10.0450888109446,4.63473218469528,21.935324363575));
#50549=CARTESIAN_POINT('Ctrl Pts',(9.8023530558227,4.6591022660215,22.3335775072864));
#50550=CARTESIAN_POINT('Ctrl Pts',(9.56010106234469,4.69257029287764,22.740811302168));
#50551=CARTESIAN_POINT('Ctrl Pts',(9.36613602941621,4.71936729395905,23.0668730831249));
#50552=CARTESIAN_POINT('Ctrl Pts',(9.15248571297353,4.75430007716532,23.4313132092381));
#50553=CARTESIAN_POINT('Ctrl Pts',(8.8902235982873,4.80813131550359,23.8935070279378));
#50554=CARTESIAN_POINT('Ctrl Pts',(8.39222406109597,4.91034940297294,24.7711492603301));
#50555=CARTESIAN_POINT('Ctrl Pts',(7.76643777375998,5.07885121123793,25.924274985688));
#50556=CARTESIAN_POINT('Ctrl Pts',(7.10363554123529,5.30796452320538,27.2733711088097));
#50557=CARTESIAN_POINT('Ctrl Pts',(6.23550018248759,5.60805610032957,29.0404110935273));
#50558=CARTESIAN_POINT('Ctrl Pts',(5.31040885822732,6.14033332093044,31.1166409635101));
#50559=CARTESIAN_POINT('Ctrl Pts',(4.46416616904365,6.67123676571769,33.3136215324547));
#50560=CARTESIAN_POINT('Ctrl Pts',(4.30741751124502,6.76957546152532,33.7205659702542));
#50561=CARTESIAN_POINT('Ctrl Pts',(4.15262292089048,6.86748895430781,34.1329983346473));
#50562=CARTESIAN_POINT('Ctrl Pts',(4.,6.96288805731186,34.5509691145741));
#50563=CARTESIAN_POINT('Ctrl Pts',(3.72434973283387,7.13518713321112,35.3058606897205));
#50564=CARTESIAN_POINT('Ctrl Pts',(3.45587123478811,7.31111181566301,36.0766370850674));
#50565=CARTESIAN_POINT('Ctrl Pts',(3.2,7.48695481785667,36.8470556158205));
#50566=CARTESIAN_POINT('',(15.,10.7022283756421,28.6674433425027));
#50567=CARTESIAN_POINT('Ctrl Pts',(15.,10.7022283756421,28.6674433425027));
#50568=CARTESIAN_POINT('Ctrl Pts',(15.,9.08413080697444,24.5602410457909));
#50569=CARTESIAN_POINT('Ctrl Pts',(15.,7.15455445431742,19.6882246137983));
#50570=CARTESIAN_POINT('Ctrl Pts',(15.,5.22423077689144,14.9103792371898));
#50571=CARTESIAN_POINT('Ctrl Pts',(6.,7.72847464911697,38.226570335278));
#50572=CARTESIAN_POINT('Ctrl Pts',(6.38595465246565,7.60981276318642,37.7031111655031));
#50573=CARTESIAN_POINT('Ctrl Pts',(6.77023648668261,7.52118446376145,37.2078421022651));
#50574=CARTESIAN_POINT('Ctrl Pts',(7.13915213286207,7.47558077173047,36.7485869352853));
#50575=CARTESIAN_POINT('Ctrl Pts',(8.10667920093242,7.35597942952432,35.5441332619163));
#50576=CARTESIAN_POINT('Ctrl Pts',(8.98019888747381,7.3811062193398,34.6149583776291));
#50577=CARTESIAN_POINT('Ctrl Pts',(9.46656009721084,7.44346431686218,34.1099258931473));
#50578=CARTESIAN_POINT('Ctrl Pts',(9.65648624874921,7.46781542308235,33.9127085282358));
#50579=CARTESIAN_POINT('Ctrl Pts',(9.79228848853741,7.49157501764555,33.7743917604516));
#50580=CARTESIAN_POINT('Ctrl Pts',(9.94593825727831,7.52350831636315,33.6191627883852));
#50581=CARTESIAN_POINT('Ctrl Pts',(10.106574086601,7.55689354020401,33.4568759534155));
#50582=CARTESIAN_POINT('Ctrl Pts',(10.2660951669676,7.59692465594275,33.2976914686953));
#50583=CARTESIAN_POINT('Ctrl Pts',(10.4261869573617,7.64527487070543,33.1391702786004));
#50584=CARTESIAN_POINT('Ctrl Pts',(10.8065549509411,7.76015193050434,32.7625339322407));
#50585=CARTESIAN_POINT('Ctrl Pts',(11.1894211925257,7.92309376200424,32.3896533653038));
#50586=CARTESIAN_POINT('Ctrl Pts',(11.6023503255242,8.14562079728536,31.9897858937717));
#50587=CARTESIAN_POINT('Ctrl Pts',(11.7531893954247,8.22690779872745,31.8437181241004));
#50588=CARTESIAN_POINT('Ctrl Pts',(11.9080270687775,8.31629347191557,31.6940743231629));
#50589=CARTESIAN_POINT('Ctrl Pts',(12.0681766131679,8.41459776815341,31.5394274952415));
#50590=CARTESIAN_POINT('Ctrl Pts',(12.1838435903474,8.48559741309695,31.4277348195979));
#50591=CARTESIAN_POINT('Ctrl Pts',(12.310086541016,8.56473913921171,31.3058885417699));
#50592=CARTESIAN_POINT('Ctrl Pts',(12.5127093730712,8.70102023533918,31.1103924050491));
#50593=CARTESIAN_POINT('Ctrl Pts',(12.7975492664042,8.89259930118548,30.8355709638236));
#50594=CARTESIAN_POINT('Ctrl Pts',(13.1874566943566,9.17392611297301,30.458814494586));
#50595=CARTESIAN_POINT('Ctrl Pts',(13.6431584568239,9.51695089116758,30.0207695274047));
#50596=CARTESIAN_POINT('Ctrl Pts',(14.069523646534,9.83789286830266,29.6109244468797));
#50597=CARTESIAN_POINT('Ctrl Pts',(14.53311408767,10.2442407770738,29.151991088712));
#50598=CARTESIAN_POINT('Ctrl Pts',(15.,10.7022283756421,28.6674433425027));
#50599=CARTESIAN_POINT('Origin',(15.,5.29966331579924,6.64556760097825));
#50600=CARTESIAN_POINT('',(15.,7.27088643053102,14.0266249226733));
#50601=CARTESIAN_POINT('Ctrl Pts',(15.,7.27088643053101,14.0266249226733));
#50602=CARTESIAN_POINT('Ctrl Pts',(15.,6.61162657474121,14.3683609829217));
#50603=CARTESIAN_POINT('Ctrl Pts',(15.,5.92779573167863,14.6638673522892));
#50604=CARTESIAN_POINT('Ctrl Pts',(15.,5.22423077689144,14.9103792371898));
#50605=CARTESIAN_POINT('',(15.,13.5614880461774,27.4307499345787));
#50606=CARTESIAN_POINT('Ctrl Pts',(15.,7.27088643053102,14.0266249226733));
#50607=CARTESIAN_POINT('Ctrl Pts',(15.,9.49405625509847,18.8359534995712));
#50608=CARTESIAN_POINT('Ctrl Pts',(15.,11.776224358769,23.666422827049));
#50609=CARTESIAN_POINT('Ctrl Pts',(15.,13.5614880461774,27.4307499345787));
#50610=CARTESIAN_POINT('Origin',(15.,0.,0.));
#50611=CARTESIAN_POINT('Ctrl Pts',(15.,19.0787879368772,23.9240433635217));
#50612=CARTESIAN_POINT('Ctrl Pts',(15.,-4.84525542664446,43.0028313003989));
#50613=CARTESIAN_POINT('Ctrl Pts',(15.,-23.9240433635217,19.0787879368772));
#50614=CARTESIAN_POINT('Ctrl Pts',(15.,-43.0028313003989,-4.84525542664446));
#50615=CARTESIAN_POINT('Ctrl Pts',(15.,-19.0787879368772,-23.9240433635217));
#50616=CARTESIAN_POINT('Ctrl Pts',(15.,4.84525542664446,-43.0028313003989));
#50617=CARTESIAN_POINT('Ctrl Pts',(15.,23.9240433635217,-19.0787879368772));
#50618=CARTESIAN_POINT('Ctrl Pts',(15.,43.0028313003989,4.84525542664446));
#50619=CARTESIAN_POINT('Ctrl Pts',(15.,19.0787879368772,23.9240433635217));
#50620=CARTESIAN_POINT('Ctrl Pts',(14.7843073131059,19.1634046954076,24.0301494226203));
#50621=CARTESIAN_POINT('Ctrl Pts',(14.7843073131059,-4.86674472721275,43.1935541180279));
#50622=CARTESIAN_POINT('Ctrl Pts',(14.7843073131059,-24.0301494226203,19.1634046954076));
#50623=CARTESIAN_POINT('Ctrl Pts',(14.7843073131059,-43.1935541180279,-4.86674472721275));
#50624=CARTESIAN_POINT('Ctrl Pts',(14.7843073131059,-19.1634046954076,-24.0301494226203));
#50625=CARTESIAN_POINT('Ctrl Pts',(14.7843073131059,4.86674472721275,-43.1935541180279));
#50626=CARTESIAN_POINT('Ctrl Pts',(14.7843073131059,24.0301494226203,-19.1634046954076));
#50627=CARTESIAN_POINT('Ctrl Pts',(14.7843073131059,43.1935541180279,4.86674472721275));
#50628=CARTESIAN_POINT('Ctrl Pts',(14.7843073131059,19.1634046954076,24.0301494226203));
#50629=CARTESIAN_POINT('Ctrl Pts',(14.3560298066371,19.3343909497437,24.2445594038433));
#50630=CARTESIAN_POINT('Ctrl Pts',(14.3560298066371,-4.91016845409963,43.578950353587));
#50631=CARTESIAN_POINT('Ctrl Pts',(14.3560298066371,-24.2445594038433,19.3343909497437));
#50632=CARTESIAN_POINT('Ctrl Pts',(14.3560298066371,-43.578950353587,-4.91016845409963));
#50633=CARTESIAN_POINT('Ctrl Pts',(14.3560298066371,-19.3343909497437,-24.2445594038433));
#50634=CARTESIAN_POINT('Ctrl Pts',(14.3560298066371,4.91016845409963,-43.578950353587));
#50635=CARTESIAN_POINT('Ctrl Pts',(14.3560298066371,24.2445594038433,-19.3343909497437));
#50636=CARTESIAN_POINT('Ctrl Pts',(14.3560298066371,43.578950353587,4.91016845409963));
#50637=CARTESIAN_POINT('Ctrl Pts',(14.3560298066371,19.3343909497437,24.2445594038433));
#50638=CARTESIAN_POINT('Ctrl Pts',(13.722936818686,19.5961283568486,24.5727677312355));
#50639=CARTESIAN_POINT('Ctrl Pts',(13.722936818686,-4.97663937438694,44.1688960880841));
#50640=CARTESIAN_POINT('Ctrl Pts',(13.722936818686,-24.5727677312355,19.5961283568486));
#50641=CARTESIAN_POINT('Ctrl Pts',(13.722936818686,-44.1688960880841,-4.97663937438694));
#50642=CARTESIAN_POINT('Ctrl Pts',(13.722936818686,-19.5961283568486,-24.5727677312355));
#50643=CARTESIAN_POINT('Ctrl Pts',(13.722936818686,4.97663937438694,-44.1688960880841));
#50644=CARTESIAN_POINT('Ctrl Pts',(13.722936818686,24.5727677312355,-19.5961283568486));
#50645=CARTESIAN_POINT('Ctrl Pts',(13.722936818686,44.1688960880841,4.97663937438694));
#50646=CARTESIAN_POINT('Ctrl Pts',(13.722936818686,19.5961283568486,24.5727677312355));
#50647=CARTESIAN_POINT('Ctrl Pts',(12.8977690042853,19.9558022366521,25.0237845110024));
#50648=CARTESIAN_POINT('Ctrl Pts',(12.8977690042853,-5.0679822743503,44.9795867476544));
#50649=CARTESIAN_POINT('Ctrl Pts',(12.8977690042853,-25.0237845110024,19.9558022366521));
#50650=CARTESIAN_POINT('Ctrl Pts',(12.8977690042853,-44.9795867476544,-5.0679822743503));
#50651=CARTESIAN_POINT('Ctrl Pts',(12.8977690042853,-19.9558022366521,-25.0237845110024));
#50652=CARTESIAN_POINT('Ctrl Pts',(12.8977690042853,5.0679822743503,-44.9795867476544));
#50653=CARTESIAN_POINT('Ctrl Pts',(12.8977690042853,25.0237845110024,-19.9558022366521));
#50654=CARTESIAN_POINT('Ctrl Pts',(12.8977690042853,44.9795867476544,5.0679822743503));
#50655=CARTESIAN_POINT('Ctrl Pts',(12.8977690042853,19.9558022366521,25.0237845110024));
#50656=CARTESIAN_POINT('Ctrl Pts',(11.9000549946031,20.4244261094473,25.6114202607695));
#50657=CARTESIAN_POINT('Ctrl Pts',(11.9000549946031,-5.18699415132218,46.0358463702168));
#50658=CARTESIAN_POINT('Ctrl Pts',(11.9000549946031,-25.6114202607695,20.4244261094473));
#50659=CARTESIAN_POINT('Ctrl Pts',(11.9000549946031,-46.0358463702168,-5.18699415132218));
#50660=CARTESIAN_POINT('Ctrl Pts',(11.9000549946031,-20.4244261094473,-25.6114202607695));
#50661=CARTESIAN_POINT('Ctrl Pts',(11.9000549946031,5.18699415132218,-46.0358463702168));
#50662=CARTESIAN_POINT('Ctrl Pts',(11.9000549946031,25.6114202607695,-20.4244261094473));
#50663=CARTESIAN_POINT('Ctrl Pts',(11.9000549946031,46.0358463702168,5.18699415132218));
#50664=CARTESIAN_POINT('Ctrl Pts',(11.9000549946031,20.4244261094473,25.6114202607695));
#50665=CARTESIAN_POINT('Ctrl Pts',(10.9391333834985,20.9137997124663,26.2250753492544));
#50666=CARTESIAN_POINT('Ctrl Pts',(10.9391333834985,-5.3112756367881,47.1388750617207));
#50667=CARTESIAN_POINT('Ctrl Pts',(10.9391333834985,-26.2250753492544,20.9137997124663));
#50668=CARTESIAN_POINT('Ctrl Pts',(10.9391333834985,-47.1388750617207,-5.3112756367881));
#50669=CARTESIAN_POINT('Ctrl Pts',(10.9391333834985,-20.9137997124663,-26.2250753492544));
#50670=CARTESIAN_POINT('Ctrl Pts',(10.9391333834985,5.3112756367881,-47.1388750617207));
#50671=CARTESIAN_POINT('Ctrl Pts',(10.9391333834985,26.2250753492544,-20.9137997124663));
#50672=CARTESIAN_POINT('Ctrl Pts',(10.9391333834985,47.1388750617207,5.3112756367881));
#50673=CARTESIAN_POINT('Ctrl Pts',(10.9391333834985,20.9137997124663,26.2250753492544));
#50674=CARTESIAN_POINT('Ctrl Pts',(10.0180552497783,21.4256437560905,26.8669074790281));
#50675=CARTESIAN_POINT('Ctrl Pts',(10.0180552497783,-5.44126372293754,48.2925512351186));
#50676=CARTESIAN_POINT('Ctrl Pts',(10.0180552497783,-26.8669074790281,21.4256437560905));
#50677=CARTESIAN_POINT('Ctrl Pts',(10.0180552497783,-48.2925512351186,-5.44126372293754));
#50678=CARTESIAN_POINT('Ctrl Pts',(10.0180552497783,-21.4256437560905,-26.8669074790281));
#50679=CARTESIAN_POINT('Ctrl Pts',(10.0180552497783,5.44126372293754,-48.2925512351186));
#50680=CARTESIAN_POINT('Ctrl Pts',(10.0180552497783,26.8669074790281,-21.4256437560905));
#50681=CARTESIAN_POINT('Ctrl Pts',(10.0180552497783,48.2925512351186,5.44126372293754));
#50682=CARTESIAN_POINT('Ctrl Pts',(10.0180552497783,21.4256437560905,26.8669074790281));
#50683=CARTESIAN_POINT('Ctrl Pts',(9.13857394886632,21.9609470764246,27.5381566113461));
#50684=CARTESIAN_POINT('Ctrl Pts',(9.13857394886632,-5.57720953492155,49.4991036877707));
#50685=CARTESIAN_POINT('Ctrl Pts',(9.13857394886632,-27.5381566113461,21.9609470764246));
#50686=CARTESIAN_POINT('Ctrl Pts',(9.13857394886632,-49.4991036877707,-5.57720953492155));
#50687=CARTESIAN_POINT('Ctrl Pts',(9.13857394886632,-21.9609470764246,-27.5381566113461));
#50688=CARTESIAN_POINT('Ctrl Pts',(9.13857394886632,5.57720953492155,-49.4991036877707));
#50689=CARTESIAN_POINT('Ctrl Pts',(9.13857394886632,27.5381566113461,-21.9609470764246));
#50690=CARTESIAN_POINT('Ctrl Pts',(9.13857394886632,49.4991036877707,5.57720953492155));
#50691=CARTESIAN_POINT('Ctrl Pts',(9.13857394886632,21.9609470764246,27.5381566113461));
#50692=CARTESIAN_POINT('Ctrl Pts',(8.29915429043693,22.5188438754702,28.2377370698584));
#50693=CARTESIAN_POINT('Ctrl Pts',(8.29915429043693,-5.71889319438813,50.7565809453286));
#50694=CARTESIAN_POINT('Ctrl Pts',(8.29915429043693,-28.2377370698584,22.5188438754702));
#50695=CARTESIAN_POINT('Ctrl Pts',(8.29915429043693,-50.7565809453286,-5.71889319438813));
#50696=CARTESIAN_POINT('Ctrl Pts',(8.29915429043693,-22.5188438754702,-28.2377370698584));
#50697=CARTESIAN_POINT('Ctrl Pts',(8.29915429043693,5.71889319438813,-50.7565809453286));
#50698=CARTESIAN_POINT('Ctrl Pts',(8.29915429043693,28.2377370698584,-22.5188438754702));
#50699=CARTESIAN_POINT('Ctrl Pts',(8.29915429043693,50.7565809453286,5.71889319438813));
#50700=CARTESIAN_POINT('Ctrl Pts',(8.29915429043693,22.5188438754702,28.2377370698584));
#50701=CARTESIAN_POINT('Ctrl Pts',(7.4968190344241,23.0976550855257,28.9635433702624));
#50702=CARTESIAN_POINT('Ctrl Pts',(7.4968190344241,-5.86588828473676,52.0611984557881));
#50703=CARTESIAN_POINT('Ctrl Pts',(7.4968190344241,-28.9635433702624,23.0976550855257));
#50704=CARTESIAN_POINT('Ctrl Pts',(7.4968190344241,-52.0611984557881,-5.86588828473676));
#50705=CARTESIAN_POINT('Ctrl Pts',(7.4968190344241,-23.0976550855257,-28.9635433702624));
#50706=CARTESIAN_POINT('Ctrl Pts',(7.4968190344241,5.86588828473676,-52.0611984557881));
#50707=CARTESIAN_POINT('Ctrl Pts',(7.4968190344241,28.9635433702624,-23.0976550855257));
#50708=CARTESIAN_POINT('Ctrl Pts',(7.4968190344241,52.0611984557881,5.86588828473676));
#50709=CARTESIAN_POINT('Ctrl Pts',(7.4968190344241,23.0976550855257,28.9635433702624));
#50710=CARTESIAN_POINT('Ctrl Pts',(6.88220761950379,23.5760760069919,29.5634642304892));
#50711=CARTESIAN_POINT('Ctrl Pts',(6.88220761950379,-5.98738822349723,53.1395402374811));
#50712=CARTESIAN_POINT('Ctrl Pts',(6.88220761950379,-29.5634642304892,23.5760760069919));
#50713=CARTESIAN_POINT('Ctrl Pts',(6.88220761950379,-53.1395402374811,-5.98738822349723));
#50714=CARTESIAN_POINT('Ctrl Pts',(6.88220761950379,-23.5760760069919,-29.5634642304892));
#50715=CARTESIAN_POINT('Ctrl Pts',(6.88220761950379,5.98738822349723,-53.1395402374811));
#50716=CARTESIAN_POINT('Ctrl Pts',(6.88220761950379,29.5634642304892,-23.5760760069919));
#50717=CARTESIAN_POINT('Ctrl Pts',(6.88220761950379,53.1395402374811,5.98738822349723));
#50718=CARTESIAN_POINT('Ctrl Pts',(6.88220761950379,23.5760760069919,29.5634642304892));
#50719=CARTESIAN_POINT('Ctrl Pts',(6.43560997955544,23.9429907960904,30.0235608233205));
#50720=CARTESIAN_POINT('Ctrl Pts',(6.43560997955544,-6.08057002723012,53.9665516194108));
#50721=CARTESIAN_POINT('Ctrl Pts',(6.43560997955544,-30.0235608233205,23.9429907960904));
#50722=CARTESIAN_POINT('Ctrl Pts',(6.43560997955544,-53.9665516194108,-6.08057002723012));
#50723=CARTESIAN_POINT('Ctrl Pts',(6.43560997955544,-23.9429907960904,-30.0235608233205));
#50724=CARTESIAN_POINT('Ctrl Pts',(6.43560997955544,6.08057002723012,-53.9665516194108));
#50725=CARTESIAN_POINT('Ctrl Pts',(6.43560997955544,30.0235608233205,-23.9429907960904));
#50726=CARTESIAN_POINT('Ctrl Pts',(6.43560997955544,53.9665516194108,6.08057002723012));
#50727=CARTESIAN_POINT('Ctrl Pts',(6.43560997955544,23.9429907960904,30.0235608233205));
#50728=CARTESIAN_POINT('Ctrl Pts',(6.14415685965718,24.1911416066824,30.3347320975618));
#50729=CARTESIAN_POINT('Ctrl Pts',(6.14415685965718,-6.14359049087935,54.5258737042442));
#50730=CARTESIAN_POINT('Ctrl Pts',(6.14415685965718,-30.3347320975618,24.1911416066824));
#50731=CARTESIAN_POINT('Ctrl Pts',(6.14415685965718,-54.5258737042442,-6.14359049087935));
#50732=CARTESIAN_POINT('Ctrl Pts',(6.14415685965718,-24.1911416066824,-30.3347320975618));
#50733=CARTESIAN_POINT('Ctrl Pts',(6.14415685965718,6.14359049087935,-54.5258737042442));
#50734=CARTESIAN_POINT('Ctrl Pts',(6.14415685965718,30.3347320975618,-24.1911416066824));
#50735=CARTESIAN_POINT('Ctrl Pts',(6.14415685965718,54.5258737042442,6.14359049087935));
#50736=CARTESIAN_POINT('Ctrl Pts',(6.14415685965718,24.1911416066824,30.3347320975618));
#50737=CARTESIAN_POINT('Ctrl Pts',(6.,24.3161022724906,30.4914278162532));
#50738=CARTESIAN_POINT('Ctrl Pts',(6.,-6.17532554376255,54.8075300887438));
#50739=CARTESIAN_POINT('Ctrl Pts',(6.,-30.4914278162532,24.3161022724906));
#50740=CARTESIAN_POINT('Ctrl Pts',(6.,-54.8075300887438,-6.17532554376255));
#50741=CARTESIAN_POINT('Ctrl Pts',(6.,-24.3161022724906,-30.4914278162532));
#50742=CARTESIAN_POINT('Ctrl Pts',(6.,6.17532554376255,-54.8075300887438));
#50743=CARTESIAN_POINT('Ctrl Pts',(6.,30.4914278162532,-24.3161022724906));
#50744=CARTESIAN_POINT('Ctrl Pts',(6.,54.8075300887438,6.17532554376255));
#50745=CARTESIAN_POINT('Ctrl Pts',(6.,24.3161022724906,30.4914278162532));
#50746=CARTESIAN_POINT('Ctrl Pts',(15.,13.5614880461774,27.4307499345787));
#50747=CARTESIAN_POINT('Ctrl Pts',(14.0108432136945,12.4969221179203,28.6513499963111));
#50748=CARTESIAN_POINT('Ctrl Pts',(13.3692319443824,11.7633381143331,29.4077674850275));
#50749=CARTESIAN_POINT('Ctrl Pts',(12.3476991724842,11.0009106836133,30.5055001671566));
#50750=CARTESIAN_POINT('Ctrl Pts',(12.0250187050191,10.7600760804358,30.8522505649563));
#50751=CARTESIAN_POINT('Ctrl Pts',(11.666631757071,10.497479920601,31.2404168505702));
#50752=CARTESIAN_POINT('Ctrl Pts',(11.3593868751766,10.2901330191653,31.573824809279));
#50753=CARTESIAN_POINT('Ctrl Pts',(10.6767716809131,9.82946417244362,32.3145672981358));
#50754=CARTESIAN_POINT('Ctrl Pts',(10.1321636914397,9.53982175368366,32.908348900279));
#50755=CARTESIAN_POINT('Ctrl Pts',(9.56604173138328,9.37660968812532,33.5284683378389));
#50756=CARTESIAN_POINT('Ctrl Pts',(9.3456307858919,9.3130655611995,33.7699023771341));
#50757=CARTESIAN_POINT('Ctrl Pts',(9.12222951098702,9.26933558002086,34.0154794389242));
#50758=CARTESIAN_POINT('Ctrl Pts',(8.88860711505289,9.24004324040524,34.2766867816041));
#50759=CARTESIAN_POINT('Ctrl Pts',(8.7583060070075,9.22370566157897,34.4223731831355));
#50760=CARTESIAN_POINT('Ctrl Pts',(8.62340343546557,9.209707571039,34.5735952627387));
#50761=CARTESIAN_POINT('Ctrl Pts',(8.40819516300421,9.20095382247576,34.8205073252293));
#50762=CARTESIAN_POINT('Ctrl Pts',(8.02443006829131,9.18534390605366,35.2608074585084));
#50763=CARTESIAN_POINT('Ctrl Pts',(7.46417034513342,9.20821248841079,35.9195836189444));
#50764=CARTESIAN_POINT('Ctrl Pts',(6.85957019142019,9.2876548102706,36.6968497152622));
#50765=CARTESIAN_POINT('Ctrl Pts',(6.58024553736738,9.32435708190311,37.0559458586018));
#50766=CARTESIAN_POINT('Ctrl Pts',(6.28976782192772,9.39495954165252,37.4362618349962));
#50767=CARTESIAN_POINT('Ctrl Pts',(6.,9.48407679455224,37.8292517419395));
#50768=CARTESIAN_POINT('Ctrl Pts',(2.09999999999999,4.3891074818719,15.1853730503683));
#50769=CARTESIAN_POINT('Ctrl Pts',(2.73333333333333,4.3891074818719,15.1853730503683));
#50770=CARTESIAN_POINT('Ctrl Pts',(3.36803488963027,4.38906293639893,15.1853891480969));
#50771=CARTESIAN_POINT('Ctrl Pts',(4.25277181297707,4.38903510934131,15.1853984318492));
#50772=CARTESIAN_POINT('Ctrl Pts',(4.77266992155204,4.38096760094831,15.1878257280945));
#50773=CARTESIAN_POINT('Ctrl Pts',(5.76857034429174,4.35758589293773,15.1949135576046));
#50774=CARTESIAN_POINT('Ctrl Pts',(6.4850861707799,4.35822862174715,15.1947749329422));
#50775=CARTESIAN_POINT('Ctrl Pts',(6.9986641671015,4.39061489150108,15.1847594251365));
#50776=CARTESIAN_POINT('Ctrl Pts',(7.12480344747274,4.39885659944923,15.1823276020454));
#50777=CARTESIAN_POINT('Ctrl Pts',(7.37170623914911,4.4162608941154,15.177371808595));
#50778=CARTESIAN_POINT('Ctrl Pts',(7.68211418916856,4.440773054857,15.1706560971746));
#50779=CARTESIAN_POINT('Ctrl Pts',(8.0507418084214,4.47522277126092,15.1612435681501));
#50780=CARTESIAN_POINT('Ctrl Pts',(8.41504100892412,4.51550554400247,15.1499364273002));
#50781=CARTESIAN_POINT('Ctrl Pts',(9.01074910230582,4.59375299963977,15.1269946547022));
#50782=CARTESIAN_POINT('Ctrl Pts',(9.46309896700665,4.67554497516132,15.1008422997988));
#50783=CARTESIAN_POINT('Ctrl Pts',(10.2678495141822,4.86554628727075,15.0344005222421));
#50784=CARTESIAN_POINT('Ctrl Pts',(10.9804938765534,5.10715483420763,14.9562757133094));
#50785=CARTESIAN_POINT('Ctrl Pts',(11.7910258900602,5.45630749934349,14.833110998574));
#50786=CARTESIAN_POINT('Ctrl Pts',(12.2471544524677,5.66565497142133,14.7535780631897));
#50787=CARTESIAN_POINT('Ctrl Pts',(12.4732504394558,5.77217429860475,14.7107195079034));
#50788=CARTESIAN_POINT('Ctrl Pts',(12.8351209164145,5.94360272017494,14.6392957979959));
#50789=CARTESIAN_POINT('Ctrl Pts',(13.2802518542094,6.17499175205375,14.5408686766578));
#50790=CARTESIAN_POINT('Ctrl Pts',(14.161256864772,6.69818327390388,14.3113175847781));
#50791=CARTESIAN_POINT('Ctrl Pts',(14.7820737708942,7.12182950163928,14.1077824544514));
#50792=CARTESIAN_POINT('Ctrl Pts',(15.1979896574214,7.40598969975549,13.9553299864943));
#50793=CARTESIAN_POINT('Ctrl Pts',(2.09999999999999,6.11056057998312,22.7275518693282));
#50794=CARTESIAN_POINT('Ctrl Pts',(2.73333333333333,6.11056057998312,22.7275518693282));
#50795=CARTESIAN_POINT('Ctrl Pts',(3.36872139010523,6.11055911614926,22.7275501174862));
#50796=CARTESIAN_POINT('Ctrl Pts',(4.25415709201328,6.11054559328987,22.7275524283132));
#50797=CARTESIAN_POINT('Ctrl Pts',(4.7831009051333,6.09839208015139,22.7309599500369));
#50798=CARTESIAN_POINT('Ctrl Pts',(5.77494051300236,6.06343326294559,22.740847682661));
#50799=CARTESIAN_POINT('Ctrl Pts',(6.4749722897255,6.06484508260633,22.7405177238962));
#50800=CARTESIAN_POINT('Ctrl Pts',(6.96727417314943,6.11201313509931,22.726891120736));
#50801=CARTESIAN_POINT('Ctrl Pts',(7.09309213456251,6.12432705592286,22.7235075398897));
#50802=CARTESIAN_POINT('Ctrl Pts',(7.33629159574246,6.15012383123003,22.7166894865964));
#50803=CARTESIAN_POINT('Ctrl Pts',(7.64236714688785,6.18649753874622,22.7074653368708));
#50804=CARTESIAN_POINT('Ctrl Pts',(8.00392257679634,6.237416056974,22.6946063739332));
#50805=CARTESIAN_POINT('Ctrl Pts',(8.36001575867264,6.29687420312726,22.6791486280887));
#50806=CARTESIAN_POINT('Ctrl Pts',(8.93968276887491,6.4119109021405,22.6478374700045));
#50807=CARTESIAN_POINT('Ctrl Pts',(9.37529806425592,6.53175739185493,22.6120247145612));
#50808=CARTESIAN_POINT('Ctrl Pts',(10.1434048645354,6.80789230240586,22.5213547453348));
#50809=CARTESIAN_POINT('Ctrl Pts',(10.8342970263929,7.16164219057595,22.4150634069346));
#50810=CARTESIAN_POINT('Ctrl Pts',(11.6346844994435,7.68020478527314,22.2442660982912));
#50811=CARTESIAN_POINT('Ctrl Pts',(12.0872580001815,7.99240455061643,22.1329978262207));
#50812=CARTESIAN_POINT('Ctrl Pts',(12.3122495048507,8.15169147256195,22.0726789031247));
#50813=CARTESIAN_POINT('Ctrl Pts',(12.6725882088788,8.40825142471423,21.9718916318112));
#50814=CARTESIAN_POINT('Ctrl Pts',(13.1110153447534,8.75180009316219,21.8345430981404));
#50815=CARTESIAN_POINT('Ctrl Pts',(13.992134418419,9.5365949967812,21.5103916607701));
#50816=CARTESIAN_POINT('Ctrl Pts',(14.6125773377935,10.1751048259157,21.2201485554486));
#50817=CARTESIAN_POINT('Ctrl Pts',(15.0291266285127,10.603144101066,21.0018664882136));
#50818=CARTESIAN_POINT('Ctrl Pts',(2.09999999999999,7.83201367809433,30.2697306882881));
#50819=CARTESIAN_POINT('Ctrl Pts',(2.73333333333333,7.83201367809433,30.2697306882881));
#50820=CARTESIAN_POINT('Ctrl Pts',(3.36945654347763,7.83198149032742,30.2697430182653));
#50821=CARTESIAN_POINT('Ctrl Pts',(4.25562154880783,7.83194277590752,30.2697546322492));
#50822=CARTESIAN_POINT('Ctrl Pts',(4.79359271386228,7.81549328468654,30.2741980639674));
#50823=CARTESIAN_POINT('Ctrl Pts',(5.7814667007226,7.76899455850239,30.2868791804613));
#50824=CARTESIAN_POINT('Ctrl Pts',(6.46487450280797,7.77155275140848,30.2862961028278));
#50825=CARTESIAN_POINT('Ctrl Pts',(6.93655488526515,7.83145888919768,30.269537124378));
#50826=CARTESIAN_POINT('Ctrl Pts',(7.06206674963109,7.84780648351963,30.2652120527099));
#50827=CARTESIAN_POINT('Ctrl Pts',(7.30169782506139,7.88161308928391,30.2566222703851));
#50828=CARTESIAN_POINT('Ctrl Pts',(7.60367667602142,7.92929132068129,30.2450297222388));
#50829=CARTESIAN_POINT('Ctrl Pts',(7.9586139633519,7.99573552796043,30.2289506497327));
#50830=CARTESIAN_POINT('Ctrl Pts',(8.30732259385584,8.07297763461527,30.2096953931838));
#50831=CARTESIAN_POINT('Ctrl Pts',(8.87311432258292,8.22194296928411,30.1707221913514));
#50832=CARTESIAN_POINT('Ctrl Pts',(9.29619366695843,8.37561549009779,30.1263948339446));
#50833=CARTESIAN_POINT('Ctrl Pts',(10.0462821922003,8.72945832787965,30.0139523275426));
#50834=CARTESIAN_POINT('Ctrl Pts',(10.7405250303565,9.19532650893385,29.880083738196));
#50835=CARTESIAN_POINT('Ctrl Pts',(11.5482319135987,9.88948391526171,29.6602270293575));
#50836=CARTESIAN_POINT('Ctrl Pts',(12.0041864194649,10.3073475275797,29.5165115073217));
#50837=CARTESIAN_POINT('Ctrl Pts',(12.2304191147553,10.5204751681415,29.4384637783906));
#50838=CARTESIAN_POINT('Ctrl Pts',(12.5924573698282,10.8635518683441,29.3079798844092));
#50839=CARTESIAN_POINT('Ctrl Pts',(13.0427811260593,11.3303280696709,29.1279900325959));
#50840=CARTESIAN_POINT('Ctrl Pts',(13.9385914588617,12.3939356634149,28.7020154314488));
#50841=CARTESIAN_POINT('Ctrl Pts',(14.5670688438605,13.2551537949985,28.3206820720608));
#50842=CARTESIAN_POINT('Ctrl Pts',(14.9853697475044,13.8290419584993,28.0347711649074));
#50843=CARTESIAN_POINT('Ctrl Pts',(2.09999999999999,9.55346677620554,37.8119095072481));
#50844=CARTESIAN_POINT('Ctrl Pts',(2.73333333333333,9.55346677620554,37.8119095072481));
#50845=CARTESIAN_POINT('Ctrl Pts',(3.37020742035998,9.55341753387,37.8119325809509));
#50846=CARTESIAN_POINT('Ctrl Pts',(4.25712565984989,9.55335946206722,37.8119521381032));
#50847=CARTESIAN_POINT('Ctrl Pts',(4.80403043076164,9.53243579429088,37.8174716594016));
#50848=CARTESIAN_POINT('Ctrl Pts',(5.7881431164665,9.47448886427121,37.8329257348436));
#50849=CARTESIAN_POINT('Ctrl Pts',(6.45446254072639,9.47858058983615,37.8319994104911));
#50850=CARTESIAN_POINT('Ctrl Pts',(6.9069189360726,9.5496032041587,37.8124809392428));
#50851=CARTESIAN_POINT('Ctrl Pts',(7.03215479329302,9.56995797627607,37.8072212231688));
#50852=CARTESIAN_POINT('Ctrl Pts',(7.26850522383847,9.61147955883885,37.7969291135373));
#50853=CARTESIAN_POINT('Ctrl Pts',(7.56684411441826,9.67009901821235,37.7830552828907));
#50854=CARTESIAN_POINT('Ctrl Pts',(7.91606061411963,9.75146832226317,37.7639015082074));
#50855=CARTESIAN_POINT('Ctrl Pts',(8.25885653597654,9.84584964259562,37.7410100895783));
#50856=CARTESIAN_POINT('Ctrl Pts',(8.81428255427399,10.0277862636405,37.6946225034532));
#50857=CARTESIAN_POINT('Ctrl Pts',(9.23054659804177,10.2153622393428,37.6418005979312));
#50858=CARTESIAN_POINT('Ctrl Pts',(9.97650814168219,10.6540278309757,37.5057959766103));
#50859=CARTESIAN_POINT('Ctrl Pts',(10.6790276368305,11.2442721267542,37.3408941588814));
#50860=CARTESIAN_POINT('Ctrl Pts',(11.4920938550392,12.1204102224677,37.0694466964272));
#50861=CARTESIAN_POINT('Ctrl Pts',(11.9504461727733,12.6463277688412,36.8921482749081));
#50862=CARTESIAN_POINT('Ctrl Pts',(12.1774757766432,12.9139906211525,36.7959324971495));
#50863=CARTESIAN_POINT('Ctrl Pts',(12.5406754666789,13.3445351774205,36.6350970810471));
#50864=CARTESIAN_POINT('Ctrl Pts',(12.997674859905,13.9394605109857,36.410163322069));
#50865=CARTESIAN_POINT('Ctrl Pts',(13.8994007067086,15.2825523021509,35.8806497606637));
#50866=CARTESIAN_POINT('Ctrl Pts',(14.5324532885843,16.3664333186909,35.4071727167216));
#50867=CARTESIAN_POINT('Ctrl Pts',(14.9514110803021,17.0856438928078,35.0531141757479));
#50868=CARTESIAN_POINT('',(3.2,9.24182505978396,36.4465179346992));
#50869=CARTESIAN_POINT('Ctrl Pts',(3.2,9.24182505978395,36.4465179346992));
#50870=CARTESIAN_POINT('Ctrl Pts',(3.56152274835423,8.9933749145984,35.3579867254307));
#50871=CARTESIAN_POINT('Ctrl Pts',(3.95224584525383,8.7474300544665,34.2543624244307));
#50872=CARTESIAN_POINT('Ctrl Pts',(4.78767430123771,8.22468504571474,32.0637774306311));
#50873=CARTESIAN_POINT('Ctrl Pts',(5.21513946232109,7.95930413376433,31.0187779627676));
#50874=CARTESIAN_POINT('Ctrl Pts',(6.79548775402598,7.09591997179492,27.3868928737702));
#50875=CARTESIAN_POINT('Ctrl Pts',(7.94016295939418,6.79083791828153,25.1816377053514));
#50876=CARTESIAN_POINT('Ctrl Pts',(9.46271935275874,6.48646562505714,22.4189535945791));
#50877=CARTESIAN_POINT('Ctrl Pts',(10.1385443659107,6.45732153174645,21.2736802981369));
#50878=CARTESIAN_POINT('Ctrl Pts',(11.5967860400751,6.61157417320919,18.9321092259658));
#50879=CARTESIAN_POINT('Ctrl Pts',(12.3997356677092,6.72026811283589,17.7072930059352));
#50880=CARTESIAN_POINT('Ctrl Pts',(13.6850585208092,6.95369959664903,15.8347320436374));
#50881=CARTESIAN_POINT('Ctrl Pts',(14.3457395898607,7.12290839200202,14.9017490241179));
#50882=CARTESIAN_POINT('Ctrl Pts',(15.,7.27088643053102,14.0266249226733));
#50883=CARTESIAN_POINT('Ctrl Pts',(2.79815110085753,9.45113165484999,37.3636308035525));
#50884=CARTESIAN_POINT('Ctrl Pts',(2.93286156280202,9.38137424991818,37.0580309336991));
#50885=CARTESIAN_POINT('Ctrl Pts',(3.06772962045781,9.31157137579472,36.7522364869069));
#50886=CARTESIAN_POINT('Ctrl Pts',(3.20258220903908,9.2417890578256,36.4465334820215));
#50887=CARTESIAN_POINT('Origin',(2.9,0.,0.));
#50888=CARTESIAN_POINT('',(3.2,22.7328514723457,29.9495820327474));
#50889=CARTESIAN_POINT('Origin',(3.2,0.,0.));
#50890=CARTESIAN_POINT('Ctrl Pts',(3.19853733010153,22.732905589146,29.9495159265607));
#50891=CARTESIAN_POINT('Ctrl Pts',(3.06441888114801,22.9284975216313,30.1948057550582));
#50892=CARTESIAN_POINT('Ctrl Pts',(2.93030256786884,23.1240541237703,30.4400509061236));
#50893=CARTESIAN_POINT('Ctrl Pts',(2.79629549285327,23.3193875333591,30.685012507583));
#50894=CARTESIAN_POINT('Ctrl Pts',(2.09999999999999,13.8302329243183,7.6592137863052));
#50895=CARTESIAN_POINT('Ctrl Pts',(2.73333333333332,13.8302329243183,7.6592137863052));
#50896=CARTESIAN_POINT('Ctrl Pts',(3.3659678189539,13.8302628375624,7.65913128553974));
#50897=CARTESIAN_POINT('Ctrl Pts',(4.12347856757956,13.8302719183902,7.65910593972428));
#50898=CARTESIAN_POINT('Ctrl Pts',(4.36307193792893,13.829345007715,7.66082148123924));
#50899=CARTESIAN_POINT('Ctrl Pts',(4.85755706347495,13.8250800963554,7.66874120057285));
#50900=CARTESIAN_POINT('Ctrl Pts',(5.73897676214029,13.81494964431,7.68759310001621));
#50901=CARTESIAN_POINT('Ctrl Pts',(6.5260410124842,13.8146756387459,7.68813277015824));
#50902=CARTESIAN_POINT('Ctrl Pts',(7.12755042026095,13.8333496467612,7.65307471747093));
#50903=CARTESIAN_POINT('Ctrl Pts',(7.25504570216537,13.8375192712337,7.64544084036889));
#50904=CARTESIAN_POINT('Ctrl Pts',(7.51730430878851,13.8468894755058,7.62865310498325));
#50905=CARTESIAN_POINT('Ctrl Pts',(7.84587135530479,13.8602867128817,7.60514723495773));
#50906=CARTESIAN_POINT('Ctrl Pts',(8.24415002878778,13.8794323696111,7.5715870957123));
#50907=CARTESIAN_POINT('Ctrl Pts',(8.77644954625804,13.9094630260358,7.51804251641122));
#50908=CARTESIAN_POINT('Ctrl Pts',(9.4411196057495,13.9562092623828,7.43162866581977));
#50909=CARTESIAN_POINT('Ctrl Pts',(9.96386966585737,14.0053914713958,7.33433060678515));
#50910=CARTESIAN_POINT('Ctrl Pts',(11.1188970074167,14.1318056158801,7.07452696639597));
#50911=CARTESIAN_POINT('Ctrl Pts',(12.0804360933392,14.3149505401524,6.71516750612135));
#50912=CARTESIAN_POINT('Ctrl Pts',(13.0008252351436,14.4960346678446,6.30114540183651));
#50913=CARTESIAN_POINT('Ctrl Pts',(13.2108022543453,14.5369701280712,6.20370984482182));
#50914=CARTESIAN_POINT('Ctrl Pts',(13.3144255310506,14.5569642596936,6.15498827691463));
#50915=CARTESIAN_POINT('Ctrl Pts',(13.3733054984755,14.5682547807254,6.1271355373132));
#50916=CARTESIAN_POINT('Ctrl Pts',(13.4025846876148,14.5738432840613,6.11323204156111));
#50917=CARTESIAN_POINT('Ctrl Pts',(13.6877790496802,14.6281168885643,5.97754713224256));
#50918=CARTESIAN_POINT('Ctrl Pts',(14.2465793638156,14.7431165252461,5.68371239772979));
#50919=CARTESIAN_POINT('Ctrl Pts',(14.7537307590314,14.8582149808983,5.37191114117815));
#50920=CARTESIAN_POINT('Ctrl Pts',(14.9999999999997,14.914658515108,5.21200130317825));
#50921=CARTESIAN_POINT('Ctrl Pts',(2.09999999999999,20.7995074576498,11.0154395130593));
#50922=CARTESIAN_POINT('Ctrl Pts',(2.73333333333333,20.7995074576498,11.0154395130593));
#50923=CARTESIAN_POINT('Ctrl Pts',(3.36558111194426,20.7995325669748,11.0153792642041));
#50924=CARTESIAN_POINT('Ctrl Pts',(4.12267542201538,20.7995396015868,11.0153621943559));
#50925=CARTESIAN_POINT('Ctrl Pts',(4.35698849797995,20.7982251231441,11.0179127481155));
#50926=CARTESIAN_POINT('Ctrl Pts',(4.84799134950577,20.7921297696213,11.0297698437277));
#50927=CARTESIAN_POINT('Ctrl Pts',(5.73067616595878,20.7775586661749,11.0581537306883));
#50928=CARTESIAN_POINT('Ctrl Pts',(6.53593220712833,20.776963041793,11.0593869811326));
#50929=CARTESIAN_POINT('Ctrl Pts',(7.15868312259406,20.8044557954121,11.0054825453739));
#50930=CARTESIAN_POINT('Ctrl Pts',(7.28650801289721,20.810461084153,10.9939824326641));
#50931=CARTESIAN_POINT('Ctrl Pts',(7.55247181782137,20.8240667812859,10.9685056887052));
#50932=CARTESIAN_POINT('Ctrl Pts',(7.8853971788604,20.8435142926672,10.9328673721134));
#50933=CARTESIAN_POINT('Ctrl Pts',(8.29075151198502,20.871389579138,10.8818111380178));
#50934=CARTESIAN_POINT('Ctrl Pts',(8.83402157842737,20.915167083861,10.8002514899699));
#50935=CARTESIAN_POINT('Ctrl Pts',(9.51596599837448,20.9834880538297,10.6681977805184));
#50936=CARTESIAN_POINT('Ctrl Pts',(10.0562863332648,21.0556116709674,10.5189202217359));
#50937=CARTESIAN_POINT('Ctrl Pts',(11.2545127308448,21.2415419513394,10.1190530365671));
#50938=CARTESIAN_POINT('Ctrl Pts',(12.2341721931925,21.5079926455151,9.57090330100297));
#50939=CARTESIAN_POINT('Ctrl Pts',(13.1607695825083,21.7667490771537,8.9461536326231));
#50940=CARTESIAN_POINT('Ctrl Pts',(13.3718704518382,21.825081315333,8.79927791727695));
#50941=CARTESIAN_POINT('Ctrl Pts',(13.4759187928771,21.8535069727006,8.72590068814449));
#50942=CARTESIAN_POINT('Ctrl Pts',(13.5350226376953,21.8695447648399,8.68396491535917));
#50943=CARTESIAN_POINT('Ctrl Pts',(13.5643924514481,21.8774759629775,8.66303720261835));
#50944=CARTESIAN_POINT('Ctrl Pts',(13.8508852807691,21.9545130564942,8.45883878182458));
#50945=CARTESIAN_POINT('Ctrl Pts',(14.4159013980166,22.1190480003223,8.01397192202503));
#50946=CARTESIAN_POINT('Ctrl Pts',(14.9236315787721,22.2815286141703,7.54600523920185));
#50947=CARTESIAN_POINT('Ctrl Pts',(15.169681381964,22.3609519415738,7.30611779695347));
#50948=CARTESIAN_POINT('Ctrl Pts',(2.09999999999999,27.7687819909813,14.3716652398135));
#50949=CARTESIAN_POINT('Ctrl Pts',(2.73333333333332,27.7687819909813,14.3716652398135));
#50950=CARTESIAN_POINT('Ctrl Pts',(3.36511119330026,27.7688208479248,14.3715582517052));
#50951=CARTESIAN_POINT('Ctrl Pts',(4.12176441016776,27.7688314711666,14.3715280007939));
#50952=CARTESIAN_POINT('Ctrl Pts',(4.3507849905463,27.7671558884117,14.3748560117099));
#50953=CARTESIAN_POINT('Ctrl Pts',(4.83832025888307,27.7592832848126,14.3905340890695));
#50954=CARTESIAN_POINT('Ctrl Pts',(5.72215842021101,27.7402636513287,14.4284570078183));
#50955=CARTESIAN_POINT('Ctrl Pts',(6.54570094113893,27.7391506882908,14.4307425531356));
#50956=CARTESIAN_POINT('Ctrl Pts',(7.1890160219809,27.7763611050952,14.3560985578327));
#50957=CARTESIAN_POINT('Ctrl Pts',(7.31715408996789,27.7842178101884,14.3406964044614));
#50958=CARTESIAN_POINT('Ctrl Pts',(7.58668580864389,27.8022272202947,14.3061738683707));
#50959=CARTESIAN_POINT('Ctrl Pts',(7.92371615677765,27.8279600361707,14.2578885292085));
#50960=CARTESIAN_POINT('Ctrl Pts',(8.33568805882525,27.8649806117798,14.1884448255293));
#50961=CARTESIAN_POINT('Ctrl Pts',(8.88880106775738,27.9232779595706,14.0771711465573));
#50962=CARTESIAN_POINT('Ctrl Pts',(9.58535043882608,28.01462294777,13.896270217051));
#50963=CARTESIAN_POINT('Ctrl Pts',(10.137537931292,28.1114587716087,13.6909226061858));
#50964=CARTESIAN_POINT('Ctrl Pts',(11.3565147873056,28.3608087900239,13.141482355084));
#50965=CARTESIAN_POINT('Ctrl Pts',(12.3227992560538,28.7078636311036,12.408808264513));
#50966=CARTESIAN_POINT('Ctrl Pts',(13.2438207447798,29.0418838222233,11.5788287297239));
#50967=CARTESIAN_POINT('Ctrl Pts',(13.4536674751769,29.1171877957502,11.3834544055582));
#50968=CARTESIAN_POINT('Ctrl Pts',(13.5572312471348,29.1538524613806,11.2858597235973));
#50969=CARTESIAN_POINT('Ctrl Pts',(13.6160706434025,29.1745370684473,11.2300668162362));
#50970=CARTESIAN_POINT('Ctrl Pts',(13.6453277307064,29.1847642914313,11.202221221814));
#50971=CARTESIAN_POINT('Ctrl Pts',(13.9304198199502,29.2840965816901,10.9305095482656));
#50972=CARTESIAN_POINT('Ctrl Pts',(14.4834678155218,29.4940622370905,10.3461367513705));
#50973=CARTESIAN_POINT('Ctrl Pts',(14.98335392639,29.7014377889178,9.73077947062731));
#50974=CARTESIAN_POINT('Ctrl Pts',(15.2260186760796,29.8027827396015,9.41523068650629));
#50975=CARTESIAN_POINT('Ctrl Pts',(2.09999999999999,34.7380565243128,17.7278909665676));
#50976=CARTESIAN_POINT('Ctrl Pts',(2.73333333333332,34.7380565243128,17.7278909665676));
#50977=CARTESIAN_POINT('Ctrl Pts',(3.36463301569964,34.7380950962072,17.7277674494899));
#50978=CARTESIAN_POINT('Ctrl Pts',(4.12084721759174,34.7381049772718,17.7277334070115));
#50979=CARTESIAN_POINT('Ctrl Pts',(4.34456258524319,34.7360905272795,17.731792616583));
#50980=CARTESIAN_POINT('Ctrl Pts',(4.82870429948491,34.7264911965689,17.7511877392265));
#50981=CARTESIAN_POINT('Ctrl Pts',(5.71349193736137,34.702986637018,17.7987242584056));
#50982=CARTESIAN_POINT('Ctrl Pts',(6.55582455797101,34.7011703174735,17.8024535759284));
#50983=CARTESIAN_POINT('Ctrl Pts',(7.21831310628172,34.7488125263721,17.7055813111283));
#50984=CARTESIAN_POINT('Ctrl Pts',(7.34673507590046,34.7585314597734,17.6862529310369));
#50985=CARTESIAN_POINT('Ctrl Pts',(7.61954646390551,34.7810737524572,17.6424115760599));
#50986=CARTESIAN_POINT('Ctrl Pts',(7.96023436813318,34.8132455546453,17.5811514236554));
#50987=CARTESIAN_POINT('Ctrl Pts',(8.37791666755937,34.8596727342253,17.4927579600399));
#50988=CARTESIAN_POINT('Ctrl Pts',(8.93895172116899,34.9328458405683,17.3509922932392));
#50989=CARTESIAN_POINT('Ctrl Pts',(9.64586775066713,35.0475998470716,17.1203589614845));
#50990=CARTESIAN_POINT('Ctrl Pts',(10.2035544184636,35.1686409304077,16.8599692096752));
#50991=CARTESIAN_POINT('Ctrl Pts',(11.4269491626946,35.4776285918087,16.1692409322816));
#50992=CARTESIAN_POINT('Ctrl Pts',(12.379436542279,35.8995568801641,15.2663852248503));
#50993=CARTESIAN_POINT('Ctrl Pts',(13.2972580417114,36.308207182279,14.2349957870837));
#50994=CARTESIAN_POINT('Ctrl Pts',(13.5062277931751,36.4003157142188,13.9920233463097));
#50995=CARTESIAN_POINT('Ctrl Pts',(13.6095005039641,36.4451932562173,13.8705333276639));
#50996=CARTESIAN_POINT('Ctrl Pts',(13.6681736295282,36.4705108919158,13.8010624659116));
#50997=CARTESIAN_POINT('Ctrl Pts',(13.6973660627842,36.4830331801897,13.7663739662738));
#50998=CARTESIAN_POINT('Ctrl Pts',(13.9814652731774,36.6045664539301,13.4281004008165));
#50999=CARTESIAN_POINT('Ctrl Pts',(14.5280851725163,36.8587744770471,12.7093432028732));
#51000=CARTESIAN_POINT('Ctrl Pts',(15.0243070371674,37.1114272400404,11.9476665753718));
#51001=CARTESIAN_POINT('Ctrl Pts',(15.2656150130537,37.2349788009363,11.5567205320759));
#51002=CARTESIAN_POINT('Ctrl Pts',(3.19846718588995,33.4762534656926,17.1201468043523));
#51003=CARTESIAN_POINT('Ctrl Pts',(3.06436072639559,33.7589037690507,17.2562800913157));
#51004=CARTESIAN_POINT('Ctrl Pts',(2.93025712268473,34.0415012332836,17.3923884232182));
#51005=CARTESIAN_POINT('Ctrl Pts',(2.79626186145775,34.3237730524972,17.5283379493497));
#51006=CARTESIAN_POINT('',(15.,29.0858399764131,9.50651949277382));
#51007=CARTESIAN_POINT('Ctrl Pts',(15.,29.0858399764131,9.50651949277382));
#51008=CARTESIAN_POINT('Ctrl Pts',(15.,24.8658325835021,8.21080036749256));
#51009=CARTESIAN_POINT('Ctrl Pts',(15.,19.8536655760794,6.68175134799012));
#51010=CARTESIAN_POINT('Ctrl Pts',(15.,14.914658515121,5.2120013031819));
#51011=CARTESIAN_POINT('Ctrl Pts',(6.,34.705361282547,17.7915119719457));
#51012=CARTESIAN_POINT('Ctrl Pts',(6.38595465246567,34.2221199480834,17.5579141160912));
#51013=CARTESIAN_POINT('Ctrl Pts',(6.77023648668261,33.7796441613039,17.3184113007142));
#51014=CARTESIAN_POINT('Ctrl Pts',(7.13915213286207,33.3921505763645,17.0677247897979));
#51015=CARTESIAN_POINT('Ctrl Pts',(8.10667920093239,32.3759005581963,16.4102683023233));
#51016=CARTESIAN_POINT('Ctrl Pts',(8.98019888747373,31.6651086781454,15.8112923224959));
#51017=CARTESIAN_POINT('Ctrl Pts',(9.46656009721078,31.309138019977,15.4476561949843));
#51018=CARTESIAN_POINT('Ctrl Pts',(9.65648624874914,31.1701299415921,15.3056547177367));
#51019=CARTESIAN_POINT('Ctrl Pts',(9.79228848853732,31.0768034028916,15.200839624557));
#51020=CARTESIAN_POINT('Ctrl Pts',(9.9459382572782,30.9753505916291,15.0790894852441));
#51021=CARTESIAN_POINT('Ctrl Pts',(10.1065740866009,30.8692849814572,14.9518036796165));
#51022=CARTESIAN_POINT('Ctrl Pts',(10.2660951669675,30.7697885322026,14.8212561902164));
#51023=CARTESIAN_POINT('Ctrl Pts',(10.4261869573617,30.6759975409703,14.6846181247282));
#51024=CARTESIAN_POINT('Ctrl Pts',(10.8065549509411,30.4531560631967,14.3599747017995));
#51025=CARTESIAN_POINT('Ctrl Pts',(11.1894211925257,30.2632188670013,14.0000944173254));
#51026=CARTESIAN_POINT('Ctrl Pts',(11.6023503255242,30.0893332260782,13.576802484847));
#51027=CARTESIAN_POINT('Ctrl Pts',(11.7531893954247,30.0258144615982,13.4221779832339));
#51028=CARTESIAN_POINT('Ctrl Pts',(11.9080270687775,29.9645492825341,13.2589920660579));
#51029=CARTESIAN_POINT('Ctrl Pts',(12.0681766131679,29.9049332499845,13.0857139522985));
#51030=CARTESIAN_POINT('Ctrl Pts',(12.1838435903474,29.8618759543631,12.9605649504314));
#51031=CARTESIAN_POINT('Ctrl Pts',(12.310086541016,29.8159567574697,12.8227195457579));
#51032=CARTESIAN_POINT('Ctrl Pts',(12.5127093730712,29.7480815967021,12.594280846792));
#51033=CARTESIAN_POINT('Ctrl Pts',(12.7975492664042,29.6526651356996,12.2731499357953));
#51034=CARTESIAN_POINT('Ctrl Pts',(13.1874566943566,29.5335094649651,11.8182959611235));
#51035=CARTESIAN_POINT('Ctrl Pts',(13.6431584568239,29.4049045698753,11.2769918204713));
#51036=CARTESIAN_POINT('Ctrl Pts',(14.069523646534,29.2845788327183,10.7705350506522));
#51037=CARTESIAN_POINT('Ctrl Pts',(14.53311408767,29.1791240620733,10.1666991941896));
#51038=CARTESIAN_POINT('Ctrl Pts',(15.,29.0858399764131,9.50651949277382));
#51039=CARTESIAN_POINT('Origin',(15.,8.5,0.));
#51040=CARTESIAN_POINT('',(15.,29.9016733813822,6.49999453793157));
#51041=CARTESIAN_POINT('Ctrl Pts',(15.,15.4997804972258,3.0608496769456));
#51042=CARTESIAN_POINT('Ctrl Pts',(15.,20.6459887015956,4.32127283870946));
#51043=CARTESIAN_POINT('Ctrl Pts',(15.,25.8455102356798,5.54875033084932));
#51044=CARTESIAN_POINT('Ctrl Pts',(15.,29.9016733813822,6.49999453793159));
#51045=CARTESIAN_POINT('Origin',(15.,0.,0.));
#51046=CARTESIAN_POINT('Ctrl Pts',(15.,30.6,0.));
#51047=CARTESIAN_POINT('Ctrl Pts',(15.,30.6,30.6));
#51048=CARTESIAN_POINT('Ctrl Pts',(15.,0.,30.6));
#51049=CARTESIAN_POINT('Ctrl Pts',(15.,-30.6,30.6));
#51050=CARTESIAN_POINT('Ctrl Pts',(15.,-30.6,0.));
#51051=CARTESIAN_POINT('Ctrl Pts',(15.,-30.6,-30.6));
#51052=CARTESIAN_POINT('Ctrl Pts',(15.,0.,-30.6));
#51053=CARTESIAN_POINT('Ctrl Pts',(15.,30.6,-30.6));
#51054=CARTESIAN_POINT('Ctrl Pts',(15.,30.6,0.));
#51055=CARTESIAN_POINT('Ctrl Pts',(14.7843073131059,30.7357147434939,0.));
#51056=CARTESIAN_POINT('Ctrl Pts',(14.7843073131059,30.7357147434939,30.7357147434939));
#51057=CARTESIAN_POINT('Ctrl Pts',(14.7843073131059,0.,30.7357147434939));
#51058=CARTESIAN_POINT('Ctrl Pts',(14.7843073131059,-30.7357147434939,30.7357147434939));
#51059=CARTESIAN_POINT('Ctrl Pts',(14.7843073131059,-30.7357147434939,0.));
#51060=CARTESIAN_POINT('Ctrl Pts',(14.7843073131059,-30.7357147434939,-30.7357147434939));
#51061=CARTESIAN_POINT('Ctrl Pts',(14.7843073131059,0.,-30.7357147434939));
#51062=CARTESIAN_POINT('Ctrl Pts',(14.7843073131059,30.7357147434939,-30.7357147434939));
#51063=CARTESIAN_POINT('Ctrl Pts',(14.7843073131059,30.7357147434939,0.));
#51064=CARTESIAN_POINT('Ctrl Pts',(14.3560298066371,31.009955402806,0.));
#51065=CARTESIAN_POINT('Ctrl Pts',(14.3560298066371,31.009955402806,31.009955402806));
#51066=CARTESIAN_POINT('Ctrl Pts',(14.3560298066371,0.,31.009955402806));
#51067=CARTESIAN_POINT('Ctrl Pts',(14.3560298066371,-31.009955402806,31.009955402806));
#51068=CARTESIAN_POINT('Ctrl Pts',(14.3560298066371,-31.009955402806,0.));
#51069=CARTESIAN_POINT('Ctrl Pts',(14.3560298066371,-31.009955402806,-31.009955402806));
#51070=CARTESIAN_POINT('Ctrl Pts',(14.3560298066371,0.,-31.009955402806));
#51071=CARTESIAN_POINT('Ctrl Pts',(14.3560298066371,31.009955402806,-31.009955402806));
#51072=CARTESIAN_POINT('Ctrl Pts',(14.3560298066371,31.009955402806,0.));
#51073=CARTESIAN_POINT('Ctrl Pts',(13.722936818686,31.4297496100642,0.));
#51074=CARTESIAN_POINT('Ctrl Pts',(13.722936818686,31.4297496100642,31.4297496100642));
#51075=CARTESIAN_POINT('Ctrl Pts',(13.722936818686,0.,31.4297496100642));
#51076=CARTESIAN_POINT('Ctrl Pts',(13.722936818686,-31.4297496100642,31.4297496100642));
#51077=CARTESIAN_POINT('Ctrl Pts',(13.722936818686,-31.4297496100642,0.));
#51078=CARTESIAN_POINT('Ctrl Pts',(13.722936818686,-31.4297496100642,-31.4297496100642));
#51079=CARTESIAN_POINT('Ctrl Pts',(13.722936818686,0.,-31.4297496100642));
#51080=CARTESIAN_POINT('Ctrl Pts',(13.722936818686,31.4297496100642,-31.4297496100642));
#51081=CARTESIAN_POINT('Ctrl Pts',(13.722936818686,31.4297496100642,0.));
#51082=CARTESIAN_POINT('Ctrl Pts',(12.8977690042853,32.0066217236598,0.));
#51083=CARTESIAN_POINT('Ctrl Pts',(12.8977690042853,32.0066217236598,32.0066217236598));
#51084=CARTESIAN_POINT('Ctrl Pts',(12.8977690042853,0.,32.0066217236598));
#51085=CARTESIAN_POINT('Ctrl Pts',(12.8977690042853,-32.0066217236598,32.0066217236598));
#51086=CARTESIAN_POINT('Ctrl Pts',(12.8977690042853,-32.0066217236598,0.));
#51087=CARTESIAN_POINT('Ctrl Pts',(12.8977690042853,-32.0066217236598,-32.0066217236598));
#51088=CARTESIAN_POINT('Ctrl Pts',(12.8977690042853,0.,-32.0066217236598));
#51089=CARTESIAN_POINT('Ctrl Pts',(12.8977690042853,32.0066217236598,-32.0066217236598));
#51090=CARTESIAN_POINT('Ctrl Pts',(12.8977690042853,32.0066217236598,0.));
#51091=CARTESIAN_POINT('Ctrl Pts',(11.9000549946031,32.7582360586468,0.));
#51092=CARTESIAN_POINT('Ctrl Pts',(11.9000549946031,32.7582360586468,32.7582360586468));
#51093=CARTESIAN_POINT('Ctrl Pts',(11.9000549946031,0.,32.7582360586468));
#51094=CARTESIAN_POINT('Ctrl Pts',(11.9000549946031,-32.7582360586468,32.7582360586468));
#51095=CARTESIAN_POINT('Ctrl Pts',(11.9000549946031,-32.7582360586468,0.));
#51096=CARTESIAN_POINT('Ctrl Pts',(11.9000549946031,-32.7582360586468,-32.7582360586468));
#51097=CARTESIAN_POINT('Ctrl Pts',(11.9000549946031,0.,-32.7582360586468));
#51098=CARTESIAN_POINT('Ctrl Pts',(11.9000549946031,32.7582360586468,-32.7582360586468));
#51099=CARTESIAN_POINT('Ctrl Pts',(11.9000549946031,32.7582360586468,0.));
#51100=CARTESIAN_POINT('Ctrl Pts',(10.9391333834985,33.5431303769822,0.));
#51101=CARTESIAN_POINT('Ctrl Pts',(10.9391333834985,33.5431303769822,33.5431303769822));
#51102=CARTESIAN_POINT('Ctrl Pts',(10.9391333834985,0.,33.5431303769822));
#51103=CARTESIAN_POINT('Ctrl Pts',(10.9391333834985,-33.5431303769822,33.5431303769822));
#51104=CARTESIAN_POINT('Ctrl Pts',(10.9391333834985,-33.5431303769822,0.));
#51105=CARTESIAN_POINT('Ctrl Pts',(10.9391333834985,-33.5431303769822,-33.5431303769822));
#51106=CARTESIAN_POINT('Ctrl Pts',(10.9391333834985,0.,-33.5431303769822));
#51107=CARTESIAN_POINT('Ctrl Pts',(10.9391333834985,33.5431303769822,-33.5431303769822));
#51108=CARTESIAN_POINT('Ctrl Pts',(10.9391333834985,33.5431303769822,0.));
#51109=CARTESIAN_POINT('Ctrl Pts',(10.0180552497783,34.3640644838406,0.));
#51110=CARTESIAN_POINT('Ctrl Pts',(10.0180552497783,34.3640644838406,34.3640644838406));
#51111=CARTESIAN_POINT('Ctrl Pts',(10.0180552497783,0.,34.3640644838406));
#51112=CARTESIAN_POINT('Ctrl Pts',(10.0180552497783,-34.3640644838406,34.3640644838406));
#51113=CARTESIAN_POINT('Ctrl Pts',(10.0180552497783,-34.3640644838406,0.));
#51114=CARTESIAN_POINT('Ctrl Pts',(10.0180552497783,-34.3640644838406,-34.3640644838406));
#51115=CARTESIAN_POINT('Ctrl Pts',(10.0180552497783,0.,-34.3640644838406));
#51116=CARTESIAN_POINT('Ctrl Pts',(10.0180552497783,34.3640644838406,-34.3640644838406));
#51117=CARTESIAN_POINT('Ctrl Pts',(10.0180552497783,34.3640644838406,0.));
#51118=CARTESIAN_POINT('Ctrl Pts',(9.13857394886632,35.2226243491956,0.));
#51119=CARTESIAN_POINT('Ctrl Pts',(9.13857394886632,35.2226243491956,35.2226243491956));
#51120=CARTESIAN_POINT('Ctrl Pts',(9.13857394886632,0.,35.2226243491956));
#51121=CARTESIAN_POINT('Ctrl Pts',(9.13857394886632,-35.2226243491956,35.2226243491956));
#51122=CARTESIAN_POINT('Ctrl Pts',(9.13857394886632,-35.2226243491956,0.));
#51123=CARTESIAN_POINT('Ctrl Pts',(9.13857394886632,-35.2226243491956,-35.2226243491956));
#51124=CARTESIAN_POINT('Ctrl Pts',(9.13857394886632,0.,-35.2226243491956));
#51125=CARTESIAN_POINT('Ctrl Pts',(9.13857394886632,35.2226243491956,-35.2226243491956));
#51126=CARTESIAN_POINT('Ctrl Pts',(9.13857394886632,35.2226243491956,0.));
#51127=CARTESIAN_POINT('Ctrl Pts',(8.29915429043693,36.1174213408745,0.));
#51128=CARTESIAN_POINT('Ctrl Pts',(8.29915429043693,36.1174213408745,36.1174213408745));
#51129=CARTESIAN_POINT('Ctrl Pts',(8.29915429043693,0.,36.1174213408745));
#51130=CARTESIAN_POINT('Ctrl Pts',(8.29915429043693,-36.1174213408745,36.1174213408745));
#51131=CARTESIAN_POINT('Ctrl Pts',(8.29915429043693,-36.1174213408745,0.));
#51132=CARTESIAN_POINT('Ctrl Pts',(8.29915429043693,-36.1174213408745,-36.1174213408745));
#51133=CARTESIAN_POINT('Ctrl Pts',(8.29915429043693,0.,-36.1174213408745));
#51134=CARTESIAN_POINT('Ctrl Pts',(8.29915429043693,36.1174213408745,-36.1174213408745));
#51135=CARTESIAN_POINT('Ctrl Pts',(8.29915429043693,36.1174213408745,0.));
#51136=CARTESIAN_POINT('Ctrl Pts',(7.4968190344241,37.0457624433751,0.));
#51137=CARTESIAN_POINT('Ctrl Pts',(7.4968190344241,37.0457624433751,37.0457624433751));
#51138=CARTESIAN_POINT('Ctrl Pts',(7.4968190344241,0.,37.0457624433751));
#51139=CARTESIAN_POINT('Ctrl Pts',(7.4968190344241,-37.0457624433751,37.0457624433751));
#51140=CARTESIAN_POINT('Ctrl Pts',(7.4968190344241,-37.0457624433751,0.));
#51141=CARTESIAN_POINT('Ctrl Pts',(7.4968190344241,-37.0457624433751,-37.0457624433751));
#51142=CARTESIAN_POINT('Ctrl Pts',(7.4968190344241,0.,-37.0457624433751));
#51143=CARTESIAN_POINT('Ctrl Pts',(7.4968190344241,37.0457624433751,-37.0457624433751));
#51144=CARTESIAN_POINT('Ctrl Pts',(7.4968190344241,37.0457624433751,0.));
#51145=CARTESIAN_POINT('Ctrl Pts',(6.88220761950379,37.8130900244198,0.));
#51146=CARTESIAN_POINT('Ctrl Pts',(6.88220761950379,37.8130900244197,37.8130900244197));
#51147=CARTESIAN_POINT('Ctrl Pts',(6.88220761950379,0.,37.8130900244198));
#51148=CARTESIAN_POINT('Ctrl Pts',(6.88220761950379,-37.8130900244197,37.8130900244197));
#51149=CARTESIAN_POINT('Ctrl Pts',(6.88220761950379,-37.8130900244198,0.));
#51150=CARTESIAN_POINT('Ctrl Pts',(6.88220761950379,-37.8130900244197,-37.8130900244197));
#51151=CARTESIAN_POINT('Ctrl Pts',(6.88220761950379,0.,-37.8130900244198));
#51152=CARTESIAN_POINT('Ctrl Pts',(6.88220761950379,37.8130900244197,-37.8130900244197));
#51153=CARTESIAN_POINT('Ctrl Pts',(6.88220761950379,37.8130900244198,0.));
#51154=CARTESIAN_POINT('Ctrl Pts',(6.43560997955544,38.4015756548256,0.));
#51155=CARTESIAN_POINT('Ctrl Pts',(6.43560997955544,38.4015756548256,38.4015756548256));
#51156=CARTESIAN_POINT('Ctrl Pts',(6.43560997955544,0.,38.4015756548256));
#51157=CARTESIAN_POINT('Ctrl Pts',(6.43560997955544,-38.4015756548256,38.4015756548256));
#51158=CARTESIAN_POINT('Ctrl Pts',(6.43560997955544,-38.4015756548256,0.));
#51159=CARTESIAN_POINT('Ctrl Pts',(6.43560997955544,-38.4015756548256,-38.4015756548256));
#51160=CARTESIAN_POINT('Ctrl Pts',(6.43560997955544,0.,-38.4015756548256));
#51161=CARTESIAN_POINT('Ctrl Pts',(6.43560997955544,38.4015756548256,-38.4015756548256));
#51162=CARTESIAN_POINT('Ctrl Pts',(6.43560997955544,38.4015756548256,0.));
#51163=CARTESIAN_POINT('Ctrl Pts',(6.14415685965718,38.7995786531943,0.));
#51164=CARTESIAN_POINT('Ctrl Pts',(6.14415685965718,38.7995786531942,38.7995786531942));
#51165=CARTESIAN_POINT('Ctrl Pts',(6.14415685965718,0.,38.7995786531943));
#51166=CARTESIAN_POINT('Ctrl Pts',(6.14415685965718,-38.7995786531942,38.7995786531942));
#51167=CARTESIAN_POINT('Ctrl Pts',(6.14415685965718,-38.7995786531943,0.));
#51168=CARTESIAN_POINT('Ctrl Pts',(6.14415685965718,-38.7995786531942,-38.7995786531942));
#51169=CARTESIAN_POINT('Ctrl Pts',(6.14415685965718,0.,-38.7995786531943));
#51170=CARTESIAN_POINT('Ctrl Pts',(6.14415685965718,38.7995786531942,-38.7995786531942));
#51171=CARTESIAN_POINT('Ctrl Pts',(6.14415685965718,38.7995786531943,0.));
#51172=CARTESIAN_POINT('Ctrl Pts',(6.,39.,0.));
#51173=CARTESIAN_POINT('Ctrl Pts',(6.,39.,39.));
#51174=CARTESIAN_POINT('Ctrl Pts',(6.,0.,39.));
#51175=CARTESIAN_POINT('Ctrl Pts',(6.,-39.,39.));
#51176=CARTESIAN_POINT('Ctrl Pts',(6.,-39.,0.));
#51177=CARTESIAN_POINT('Ctrl Pts',(6.,-39.,-39.));
#51178=CARTESIAN_POINT('Ctrl Pts',(6.,0.,-39.));
#51179=CARTESIAN_POINT('Ctrl Pts',(6.,39.,-39.));
#51180=CARTESIAN_POINT('Ctrl Pts',(6.,39.,0.));
#51181=CARTESIAN_POINT('Ctrl Pts',(15.,29.9016733813822,6.49999453793157));
#51182=CARTESIAN_POINT('Ctrl Pts',(14.0108432136945,30.1922309374725,8.0933373864441));
#51183=CARTESIAN_POINT('Ctrl Pts',(13.3692319443824,30.326239798997,9.13849504564574));
#51184=CARTESIAN_POINT('Ctrl Pts',(12.3476991724842,30.7091160415085,10.4190099465543));
#51185=CARTESIAN_POINT('Ctrl Pts',(12.0250187050191,30.8300585000507,10.8234973582048));
#51186=CARTESIAN_POINT('Ctrl Pts',(11.6666317570709,30.9698130949121,11.2708210236445));
#51187=CARTESIAN_POINT('Ctrl Pts',(11.3593868751765,31.1012032550439,11.6408078210926));
#51188=CARTESIAN_POINT('Ctrl Pts',(10.6767716809131,31.3931167252689,12.4628186160575));
#51189=CARTESIAN_POINT('Ctrl Pts',(10.1321636914396,31.6767647812522,13.0594869511698));
#51190=CARTESIAN_POINT('Ctrl Pts',(9.56604173138329,32.0598326220109,13.5737294275949));
#51191=CARTESIAN_POINT('Ctrl Pts',(9.34563078589187,32.2089742397651,13.7739418878736));
#51192=CARTESIAN_POINT('Ctrl Pts',(9.12222951098694,32.3737089207443,13.9612461574834));
#51193=CARTESIAN_POINT('Ctrl Pts',(8.88860711505277,32.5596655696803,14.1470079451216));
#51194=CARTESIAN_POINT('Ctrl Pts',(8.7583060070074,32.6633814711798,14.2506151642196));
#51195=CARTESIAN_POINT('Ctrl Pts',(8.62340343546547,32.7728839871607,14.3558447365466));
#51196=CARTESIAN_POINT('Ctrl Pts',(8.40819516300415,32.9604697380598,14.5166358456818));
#51197=CARTESIAN_POINT('Ctrl Pts',(8.02443006829124,33.2949776202952,14.8033628126358));
#51198=CARTESIAN_POINT('Ctrl Pts',(7.46417034513341,33.8242878903061,15.1962236527291));
#51199=CARTESIAN_POINT('Ctrl Pts',(6.85957019142019,34.4815104721779,15.6187306288434));
#51200=CARTESIAN_POINT('Ctrl Pts',(6.58024553736738,34.7851466343415,15.813928420662));
#51201=CARTESIAN_POINT('Ctrl Pts',(6.28976782192773,35.1265095516122,15.9958523276561));
#51202=CARTESIAN_POINT('Ctrl Pts',(6.,35.4893251315053,16.1712028529206));
#51203=CARTESIAN_POINT('Ctrl Pts',(2.09999999999999,14.6089664780085,6.03638282506164));
#51204=CARTESIAN_POINT('Ctrl Pts',(2.73333333333333,14.6089664780085,6.03638282506164));
#51205=CARTESIAN_POINT('Ctrl Pts',(3.36803666141114,14.6089514020126,6.03642739040373));
#51206=CARTESIAN_POINT('Ctrl Pts',(4.25277476731229,14.6089413613359,6.03645479962891));
#51207=CARTESIAN_POINT('Ctrl Pts',(4.77267392779604,14.60580914364,6.04427548151238));
#51208=CARTESIAN_POINT('Ctrl Pts',(5.76857452348673,14.5967723861308,6.06697519718139));
#51209=CARTESIAN_POINT('Ctrl Pts',(6.48509174407547,14.5970648927013,6.06638586537466));
#51210=CARTESIAN_POINT('Ctrl Pts',(6.99867014586152,14.6094270147457,6.03482055846387));
#51211=CARTESIAN_POINT('Ctrl Pts',(7.1248094424352,14.6126643615689,6.02686070999685));
#51212=CARTESIAN_POINT('Ctrl Pts',(7.37171227452388,14.6196411713314,6.01016358539879));
#51213=CARTESIAN_POINT('Ctrl Pts',(7.68212033066544,14.6296737194089,5.98681197306643));
#51214=CARTESIAN_POINT('Ctrl Pts',(8.05074799119104,14.6437937592098,5.95400947356552));
#51215=CARTESIAN_POINT('Ctrl Pts',(8.41504720380524,14.6600693966795,5.91546519208662));
#51216=CARTESIAN_POINT('Ctrl Pts',(9.01075539007779,14.6909192905048,5.83998490346081));
#51217=CARTESIAN_POINT('Ctrl Pts',(9.46310502651324,14.7214690610296,5.75973149002296));
#51218=CARTESIAN_POINT('Ctrl Pts',(10.2678550742082,14.7879867129576,5.569756534774));
#51219=CARTESIAN_POINT('Ctrl Pts',(10.9804987763497,14.8775467668719,5.33214922536331));
#51220=CARTESIAN_POINT('Ctrl Pts',(11.7910302654894,14.9989457804806,4.98237890778244));
#51221=CARTESIAN_POINT('Ctrl Pts',(12.2471584184909,15.0672903894667,4.76911662962923));
#51222=CARTESIAN_POINT('Ctrl Pts',(12.4732540604029,15.1001958841229,4.65911473846363));
#51223=CARTESIAN_POINT('Ctrl Pts',(12.8351237302837,15.1512383265106,4.48055499444762));
#51224=CARTESIAN_POINT('Ctrl Pts',(13.2802523785554,15.2185532647417,4.23828041374628));
#51225=CARTESIAN_POINT('Ctrl Pts',(14.1612572158898,15.3652875432003,3.68611012476648));
#51226=CARTESIAN_POINT('Ctrl Pts',(14.7820737708942,15.470296535549,3.22798797004085));
#51227=CARTESIAN_POINT('Ctrl Pts',(15.1979896574214,15.5282753821398,2.91077002204977));
#51228=CARTESIAN_POINT('Ctrl Pts',(2.09999999999999,21.5789877761254,9.39296817478263));
#51229=CARTESIAN_POINT('Ctrl Pts',(2.73333333333333,21.5789877761254,9.39296817478263));
#51230=CARTESIAN_POINT('Ctrl Pts',(3.36872402064119,21.5789856176355,9.39296797552278));
#51231=CARTESIAN_POINT('Ctrl Pts',(4.25416148268258,21.5789790511069,9.392979870206));
#51232=CARTESIAN_POINT('Ctrl Pts',(4.78310686396947,21.5740656337635,9.40460628784076));
#51233=CARTESIAN_POINT('Ctrl Pts',(5.7749467285248,21.5599997188704,9.43810307140346));
#51234=CARTESIAN_POINT('Ctrl Pts',(6.47498060646073,21.5606222109823,9.43679310319786));
#51235=CARTESIAN_POINT('Ctrl Pts',(6.96728310384879,21.5793773776101,9.39141943079971));
#51236=CARTESIAN_POINT('Ctrl Pts',(7.09310109124563,21.5844095945329,9.37968238548475));
#51237=CARTESIAN_POINT('Ctrl Pts',(7.33630061315444,21.5951630588673,9.35526265367197));
#51238=CARTESIAN_POINT('Ctrl Pts',(7.64237634935319,21.6106299965699,9.32107331035839));
#51239=CARTESIAN_POINT('Ctrl Pts',(8.00393183687127,21.6323236359645,9.2732461684707));
#51240=CARTESIAN_POINT('Ctrl Pts',(8.36002509556223,21.6573098677089,9.21712208992312));
#51241=CARTESIAN_POINT('Ctrl Pts',(8.93969220933936,21.7045540211068,9.10766060638776));
#51242=CARTESIAN_POINT('Ctrl Pts',(9.37530742884795,21.7512776632157,8.99163168810944));
#51243=CARTESIAN_POINT('Ctrl Pts',(10.1434139136649,21.8525564909802,8.71920853681163));
#51244=CARTESIAN_POINT('Ctrl Pts',(10.8343055464128,21.9900141967434,8.37636376802415));
#51245=CARTESIAN_POINT('Ctrl Pts',(11.6346923207873,22.1797979536336,7.864444884977));
#51246=CARTESIAN_POINT('Ctrl Pts',(12.0872652828465,22.2874582208771,7.55098281250724));
#51247=CARTESIAN_POINT('Ctrl Pts',(12.312256311387,22.339612685259,7.38883923970189));
#51248=CARTESIAN_POINT('Ctrl Pts',(12.6725939224516,22.4207763450689,7.12541325842979));
#51249=CARTESIAN_POINT('Ctrl Pts',(13.1110177472958,22.5275914879739,6.77118204758255));
#51250=CARTESIAN_POINT('Ctrl Pts',(13.9921364194962,22.7634712687919,5.95549963705341));
#51251=CARTESIAN_POINT('Ctrl Pts',(14.6125773377935,22.9346542951002,5.27532892793625));
#51252=CARTESIAN_POINT('Ctrl Pts',(15.0291266285127,23.0308726257289,4.80457770404129));
#51253=CARTESIAN_POINT('Ctrl Pts',(2.09999999999999,28.5490090742423,12.7495535245036));
#51254=CARTESIAN_POINT('Ctrl Pts',(2.73333333333333,28.5490090742423,12.7495535245036));
#51255=CARTESIAN_POINT('Ctrl Pts',(3.36945962045071,28.5489988659933,12.7495858434391));
#51256=CARTESIAN_POINT('Ctrl Pts',(4.25562677475033,28.548983910761,12.7496231050857));
#51257=CARTESIAN_POINT('Ctrl Pts',(4.79359981952435,28.5422019513635,12.7652539921132));
#51258=CARTESIAN_POINT('Ctrl Pts',(5.78147410742106,28.5231249848973,12.8095146599695));
#51259=CARTESIAN_POINT('Ctrl Pts',(6.46488413675066,28.5242644790789,12.807150202051));
#51260=CARTESIAN_POINT('Ctrl Pts',(6.93656514263953,28.5485127737679,12.7498643501742));
#51261=CARTESIAN_POINT('Ctrl Pts',(7.06207703364772,28.5553238593071,12.7343866375677));
#51262=CARTESIAN_POINT('Ctrl Pts',(7.30170817267462,28.5696861826432,12.7025998999942));
#51263=CARTESIAN_POINT('Ctrl Pts',(7.60368716963869,28.5903497015348,12.6580956050301));
#51264=CARTESIAN_POINT('Ctrl Pts',(7.95862452315423,28.6192058724396,12.5961222713689));
#51265=CARTESIAN_POINT('Ctrl Pts',(8.30733312679259,28.6523112124029,12.523726394015));
#51266=CARTESIAN_POINT('Ctrl Pts',(8.8731250253757,28.7147191108611,12.3829612054092));
#51267=CARTESIAN_POINT('Ctrl Pts',(9.29620381707367,28.7758759281063,12.2351772427441));
#51268=CARTESIAN_POINT('Ctrl Pts',(10.0462912732546,28.9085823331564,11.8884246619425));
#51269=CARTESIAN_POINT('Ctrl Pts',(10.740532795554,29.0943838012938,11.4407282263606));
#51270=CARTESIAN_POINT('Ctrl Pts',(11.5482388974608,29.3552929061951,10.7609358700024));
#51271=CARTESIAN_POINT('Ctrl Pts',(12.0041928460984,29.5034651889877,10.3446320328701));
#51272=CARTESIAN_POINT('Ctrl Pts',(12.230425106128,29.5753278301561,10.1293404338719));
#51273=CARTESIAN_POINT('Ctrl Pts',(12.5924623870156,29.6872159910832,9.77975755752727));
#51274=CARTESIAN_POINT('Ctrl Pts',(13.0427831926884,29.8375237688369,9.30259724740986));
#51275=CARTESIAN_POINT('Ctrl Pts',(13.9385931985019,30.1676318405281,8.20544467893018));
#51276=CARTESIAN_POINT('Ctrl Pts',(14.5670688438605,30.4064540621557,7.29435991172798));
#51277=CARTESIAN_POINT('Ctrl Pts',(14.9853697475044,30.5407333311124,6.66741354323698));
#51278=CARTESIAN_POINT('Ctrl Pts',(2.09999999999999,35.5190303723591,16.1061388742246));
#51279=CARTESIAN_POINT('Ctrl Pts',(2.73333333333333,35.5190303723591,16.1061388742246));
#51280=CARTESIAN_POINT('Ctrl Pts',(3.37021074703255,35.5190179918661,16.1061910341859));
#51281=CARTESIAN_POINT('Ctrl Pts',(4.25713143432193,35.5189972061824,16.1062482951899));
#51282=CARTESIAN_POINT('Ctrl Pts',(4.80403829546565,35.510266996621,16.1260480687564));
#51283=CARTESIAN_POINT('Ctrl Pts',(5.78815131161474,35.4862201834073,16.180988197307));
#51284=CARTESIAN_POINT('Ctrl Pts',(6.45447278497571,35.4880475600299,16.1772104845916));
#51285=CARTESIAN_POINT('Ctrl Pts',(6.90692970616558,35.5170694427124,16.1095128073425));
#51286=CARTESIAN_POINT('Ctrl Pts',(7.03216558775775,35.5256482290679,16.0903194135008));
#51287=CARTESIAN_POINT('Ctrl Pts',(7.26851607471023,35.5434898324498,16.0514394705235));
#51288=CARTESIAN_POINT('Ctrl Pts',(7.5668550388522,35.5691915200528,15.9969586081747));
#51289=CARTESIAN_POINT('Ctrl Pts',(7.91607160146964,35.6049494436263,15.9213993037407));
#51290=CARTESIAN_POINT('Ctrl Pts',(8.25886737580142,35.6458980270327,15.8333363661135));
#51291=CARTESIAN_POINT('Ctrl Pts',(8.81429360289333,35.723066410625,15.6621703423368));
#51292=CARTESIAN_POINT('Ctrl Pts',(9.23055663723524,35.7987202743156,15.4825835430176));
#51293=CARTESIAN_POINT('Ctrl Pts',(9.97651644615983,35.9658910107846,15.054823514641));
#51294=CARTESIAN_POINT('Ctrl Pts',(10.6790340006355,36.2049767460737,14.4905374879589));
#51295=CARTESIAN_POINT('Ctrl Pts',(11.4920994849111,36.5390136314546,13.6363007393238));
#51296=CARTESIAN_POINT('Ctrl Pts',(11.9504512738392,36.7283002504095,13.1145784039871));
#51297=CARTESIAN_POINT('Ctrl Pts',(12.1774805106591,36.8199606829071,12.8453218913326));
#51298=CARTESIAN_POINT('Ctrl Pts',(12.5406793815449,36.96265437758,12.4084300684841));
#51299=CARTESIAN_POINT('Ctrl Pts',(12.9976763399582,37.1577232826404,11.8030567245028));
#51300=CARTESIAN_POINT('Ctrl Pts',(13.8994020122616,37.5811368967158,10.4228391106914));
#51301=CARTESIAN_POINT('Ctrl Pts',(14.5324532885843,37.8867466021208,9.28021827726047));
#51302=CARTESIAN_POINT('Ctrl Pts',(14.9514110803021,38.0583529465017,8.49716491833391));
#51303=CARTESIAN_POINT('Ctrl Pts',(2.798152196741,35.1047471537606,15.9066502643122));
#51304=CARTESIAN_POINT('Ctrl Pts',(2.93286303103765,34.8223265530396,15.7706503227344));
#51305=CARTESIAN_POINT('Ctrl Pts',(3.06773152562602,34.5397254804734,15.6345646039347));
#51306=CARTESIAN_POINT('Ctrl Pts',(3.20258456668168,34.2572087160036,15.4985198290696));
#51307=CARTESIAN_POINT('Origin',(2.9,0.,0.));
#51308=CARTESIAN_POINT('Ctrl Pts',(3.19857191619793,37.5892075716104,0.899903760279396));
#51309=CARTESIAN_POINT('Ctrl Pts',(3.06444712372839,37.9029327677378,0.899921831100886));
#51310=CARTESIAN_POINT('Ctrl Pts',(2.93032447855964,38.2166010036509,0.899939693238254));
#51311=CARTESIAN_POINT('Ctrl Pts',(2.79631192480608,38.5299083490545,0.899954961404293));
#51312=CARTESIAN_POINT('Ctrl Pts',(2.09999999999998,6.75299193722314,-7.02449612538514));
#51313=CARTESIAN_POINT('Ctrl Pts',(2.73333333333332,6.75299193722314,-7.02449612538514));
#51314=CARTESIAN_POINT('Ctrl Pts',(3.36629680224277,6.75294648044154,-7.02452016539764));
#51315=CARTESIAN_POINT('Ctrl Pts',(4.12414743392493,6.75293267299237,-7.02452736897372));
#51316=CARTESIAN_POINT('Ctrl Pts',(4.36789509311751,6.75382103504332,-7.02368998068708));
#51317=CARTESIAN_POINT('Ctrl Pts',(4.86512395930617,6.75788793280844,-7.01986881358228));
#51318=CARTESIAN_POINT('Ctrl Pts',(5.74554025010893,6.76750052914464,-7.01085632454488));
#51319=CARTESIAN_POINT('Ctrl Pts',(6.51830366083575,6.76765825457168,-7.01071350589478));
#51320=CARTESIAN_POINT('Ctrl Pts',(7.10303189226247,6.75024197486783,-7.02690235429379));
#51321=CARTESIAN_POINT('Ctrl Pts',(7.23018703713608,6.7463685680123,-7.03058370260869));
#51322=CARTESIAN_POINT('Ctrl Pts',(7.42486685339525,6.74004512713713,-7.03670244791982));
#51323=CARTESIAN_POINT('Ctrl Pts',(7.6194364855123,6.73325250401511,-7.04336236931274));
#51324=CARTESIAN_POINT('Ctrl Pts',(8.01068306999147,6.71849387075291,-7.0579132628484));
#51325=CARTESIAN_POINT('Ctrl Pts',(8.60074918882448,6.69138911852921,-7.08463511606578));
#51326=CARTESIAN_POINT('Ctrl Pts',(9.25145738716207,6.64822816144239,-7.12531658480113));
#51327=CARTESIAN_POINT('Ctrl Pts',(9.76258194382415,6.60305748460113,-7.16601134101606));
#51328=CARTESIAN_POINT('Ctrl Pts',(10.0140805571163,6.57639478329963,-7.18937328759642));
#51329=CARTESIAN_POINT('Ctrl Pts',(10.7176652140345,6.49442351251533,-7.26012459111955));
#51330=CARTESIAN_POINT('Ctrl Pts',(11.8207747103308,6.31202427192381,-7.42265737436954));
#51331=CARTESIAN_POINT('Ctrl Pts',(12.8079604271039,6.07976122230612,-7.61409929856026));
#51332=CARTESIAN_POINT('Ctrl Pts',(13.5603806430126,5.88952590137785,-7.75631007302585));
#51333=CARTESIAN_POINT('Ctrl Pts',(14.1415267869189,5.72554047740206,-7.87660644726836));
#51334=CARTESIAN_POINT('Ctrl Pts',(15.2007169695464,5.37141982919035,-8.12566684501762));
#51335=CARTESIAN_POINT('Ctrl Pts',(15.9285176347281,5.07939082457031,-8.3118546564427));
#51336=CARTESIAN_POINT('Ctrl Pts',(16.6748049519623,4.76690229253182,-8.48846939426682));
#51337=CARTESIAN_POINT('Ctrl Pts',(17.2498356711401,4.50587852518841,-8.62929368175018));
#51338=CARTESIAN_POINT('Ctrl Pts',(18.2985117640075,3.9647261188096,-8.89613004054933));
#51339=CARTESIAN_POINT('Ctrl Pts',(19.0237320074819,3.53448198826109,-9.07450848842596));
#51340=CARTESIAN_POINT('Ctrl Pts',(19.7682744015967,3.07986955814412,-9.23156441073578));
#51341=CARTESIAN_POINT('Ctrl Pts',(20.3332383300351,2.7118628485122,-9.34724050739632));
#51342=CARTESIAN_POINT('Ctrl Pts',(21.372378830394,1.96371839940456,-9.54011298855374));
#51343=CARTESIAN_POINT('Ctrl Pts',(22.0963025405429,1.38682032165031,-9.63797649524687));
#51344=CARTESIAN_POINT('Ctrl Pts',(23.2302948553031,0.477375867824664,-9.72705857836219));
#51345=CARTESIAN_POINT('Ctrl Pts',(23.8854423668127,-0.0855090234660345,
-9.73358440568022));
#51346=CARTESIAN_POINT('Ctrl Pts',(24.5000000001022,-0.653978160206666,
-9.69209888135266));
#51347=CARTESIAN_POINT('Ctrl Pts',(2.09999999999998,9.36161601894518,-10.2956072597364));
#51348=CARTESIAN_POINT('Ctrl Pts',(2.73333333333332,9.36161601894518,-10.2956072597364));
#51349=CARTESIAN_POINT('Ctrl Pts',(3.36609438168516,9.36156585800923,-10.2956375248605));
#51350=CARTESIAN_POINT('Ctrl Pts',(4.12372361563831,9.36155092417073,-10.2956464147504));
#51351=CARTESIAN_POINT('Ctrl Pts',(4.36461784942786,9.36284448355378,-10.2944948929266));
#51352=CARTESIAN_POINT('Ctrl Pts',(4.85995591676349,9.36878888517195,-10.2892169831617));
#51353=CARTESIAN_POINT('Ctrl Pts',(5.74107832803173,9.38288286660015,-10.2767239120257));
#51354=CARTESIAN_POINT('Ctrl Pts',(6.52361564496404,9.38322607140847,-10.2764377689791));
#51355=CARTESIAN_POINT('Ctrl Pts',(7.11998100333695,9.35737516337016,-10.2991928575083));
#51356=CARTESIAN_POINT('Ctrl Pts',(7.24728410350207,9.35169382747716,-10.3042998764577));
#51357=CARTESIAN_POINT('Ctrl Pts',(7.4435678678656,9.34237505256982,-10.3128318292894));
#51358=CARTESIAN_POINT('Ctrl Pts',(7.63948101177056,9.33237103854479,-10.3221128622443));
#51359=CARTESIAN_POINT('Ctrl Pts',(8.0340967935931,9.31060889220749,-10.3424138549802));
#51360=CARTESIAN_POINT('Ctrl Pts',(8.63042364409642,9.27061026833392,-10.3797388678114));
#51361=CARTESIAN_POINT('Ctrl Pts',(9.29098306564,9.20676833650965,-10.4366867439073));
#51362=CARTESIAN_POINT('Ctrl Pts',(9.81197049062606,9.13980195102037,-10.4937819496382));
#51363=CARTESIAN_POINT('Ctrl Pts',(10.069143776842,9.1002104487285,-10.5266151541551));
#51364=CARTESIAN_POINT('Ctrl Pts',(10.7899979265155,8.97839988105312,-10.6261584553481));
#51365=CARTESIAN_POINT('Ctrl Pts',(11.9162899768689,8.70761596878294,-10.8543740998181));
#51366=CARTESIAN_POINT('Ctrl Pts',(12.9132370071959,8.36589560061933,-11.1201717547005));
#51367=CARTESIAN_POINT('Ctrl Pts',(13.6696754081786,8.08747451286091,-11.3161896788352));
#51368=CARTESIAN_POINT('Ctrl Pts',(14.2631204889818,7.84486957224345,-11.4840253590975));
#51369=CARTESIAN_POINT('Ctrl Pts',(15.3328909170884,7.32460265515443,-11.8280126795526));
#51370=CARTESIAN_POINT('Ctrl Pts',(16.0654084078213,6.89829469358604,-12.0827574614016));
#51371=CARTESIAN_POINT('Ctrl Pts',(16.8131418270019,6.44426633978414,-12.3219400191413));
#51372=CARTESIAN_POINT('Ctrl Pts',(17.3939906627799,6.06256663230004,-12.514066674993));
#51373=CARTESIAN_POINT('Ctrl Pts',(18.4452288839039,5.2762145869006,-12.8733663676658));
#51374=CARTESIAN_POINT('Ctrl Pts',(19.1721282346241,4.6539325222597,-13.1101502920758));
#51375=CARTESIAN_POINT('Ctrl Pts',(19.9175012294455,3.99789509083657,-13.3148682619423));
#51376=CARTESIAN_POINT('Ctrl Pts',(20.4827544940035,3.466823258858,-13.4651313654059));
#51377=CARTESIAN_POINT('Ctrl Pts',(21.519538834352,2.39128782352223,-13.7085532256609));
#51378=CARTESIAN_POINT('Ctrl Pts',(22.243410118146,1.5640378022019,-13.8238924709145));
#51379=CARTESIAN_POINT('Ctrl Pts',(23.3781373608504,0.261264463150115,-13.9119182156481));
#51380=CARTESIAN_POINT('Ctrl Pts',(24.0312127056184,-0.541258504051994,
-13.8980156514996));
#51381=CARTESIAN_POINT('Ctrl Pts',(24.6419825553303,-1.34841806297972,-13.8153739167048));
#51382=CARTESIAN_POINT('Ctrl Pts',(2.09999999999998,15.4484055429633,-17.9281999065559));
#51383=CARTESIAN_POINT('Ctrl Pts',(2.73333333333332,15.4484055429633,-17.9281999065559));
#51384=CARTESIAN_POINT('Ctrl Pts',(3.36560383820943,15.4482542660188,-17.9282842178703));
#51385=CARTESIAN_POINT('Ctrl Pts',(4.12271164892521,15.4482089930623,-17.9283090301052));
#51386=CARTESIAN_POINT('Ctrl Pts',(4.35694416238013,15.4504098665771,-17.9264523289363));
#51387=CARTESIAN_POINT('Ctrl Pts',(4.84788036531876,15.4606575463775,-17.9178309694623));
#51388=CARTESIAN_POINT('Ctrl Pts',(5.73060854685652,15.485197672036,-17.8972160956483));
#51389=CARTESIAN_POINT('Ctrl Pts',(6.53602142225768,15.4861289234307,-17.8964252059536));
#51390=CARTESIAN_POINT('Ctrl Pts',(7.15927193639697,15.4394328734173,-17.9354092414246));
#51391=CARTESIAN_POINT('Ctrl Pts',(7.28691515507382,15.4295142084321,-17.9438564347644));
#51392=CARTESIAN_POINT('Ctrl Pts',(7.48689772923258,15.41303282797,-17.9581538640174));
#51393=CARTESIAN_POINT('Ctrl Pts',(7.68589884468759,15.3953696129726,-17.9736779025854));
#51394=CARTESIAN_POINT('Ctrl Pts',(8.08824873453489,15.356840805821,-18.0077261400577));
#51395=CARTESIAN_POINT('Ctrl Pts',(8.69882087827138,15.2857078414599,-18.0705698025253));
#51396=CARTESIAN_POINT('Ctrl Pts',(9.38132108146395,15.1714461091176,-18.1670963317517));
#51397=CARTESIAN_POINT('Ctrl Pts',(9.92332887561784,15.0508171497738,-18.2645410332219));
#51398=CARTESIAN_POINT('Ctrl Pts',(10.1920703899024,14.9791813953041,-18.3208470995776));
#51399=CARTESIAN_POINT('Ctrl Pts',(10.9468728975028,14.7580401386903,-18.4921370629072));
#51400=CARTESIAN_POINT('Ctrl Pts',(12.1070803455683,14.2700737980981,-18.8807886500581));
#51401=CARTESIAN_POINT('Ctrl Pts',(13.1092903106678,13.669858687101,-19.3206148967827));
#51402=CARTESIAN_POINT('Ctrl Pts',(13.8683686220617,13.1837700651208,-19.6422817166552));
#51403=CARTESIAN_POINT('Ctrl Pts',(14.4658593195641,12.7565083867518,-19.9207911761091));
#51404=CARTESIAN_POINT('Ctrl Pts',(15.5292642023136,11.8549986940082,-20.4808296687727));
#51405=CARTESIAN_POINT('Ctrl Pts',(16.2562125089207,11.1195209746368,-20.8922494630454));
#51406=CARTESIAN_POINT('Ctrl Pts',(17.0019278536568,10.3355434884947,-21.2762452283177));
#51407=CARTESIAN_POINT('Ctrl Pts',(17.571102235943,9.68442584412187,-21.5819298232724));
#51408=CARTESIAN_POINT('Ctrl Pts',(18.6069001071236,8.34497393440998,-22.1498934640546));
#51409=CARTESIAN_POINT('Ctrl Pts',(19.324410136667,7.28445042254237,-22.5206154711307));
#51410=CARTESIAN_POINT('Ctrl Pts',(20.0667019463849,6.16093662590418,-22.8369405220828));
#51411=CARTESIAN_POINT('Ctrl Pts',(20.6168083009691,5.26926327642183,-23.0642318020815));
#51412=CARTESIAN_POINT('Ctrl Pts',(21.6393821249845,3.45112699200824,-23.4269677091127));
#51413=CARTESIAN_POINT('Ctrl Pts',(22.355423454672,2.04984247969421,-23.5861493055354));
#51414=CARTESIAN_POINT('Ctrl Pts',(23.4866230007993,-0.166763625493847,
-23.6784015849194));
#51415=CARTESIAN_POINT('Ctrl Pts',(24.1251264448473,-1.50769880146339,-23.6212865253562));
#51416=CARTESIAN_POINT('Ctrl Pts',(24.7275462447973,-2.86016104503983,-23.4511481200426));
#51417=CARTESIAN_POINT('Ctrl Pts',(2.09999999999998,21.5351950669813,-25.5607925533754));
#51418=CARTESIAN_POINT('Ctrl Pts',(2.73333333333332,21.5351950669813,-25.5607925533754));
#51419=CARTESIAN_POINT('Ctrl Pts',(3.36505757484791,21.5350703650623,-25.5608567667729));
#51420=CARTESIAN_POINT('Ctrl Pts',(4.12163108581741,21.5350353954978,-25.560873804661));
#51421=CARTESIAN_POINT('Ctrl Pts',(4.34918564951889,21.5380828728627,-25.5583623704001));
#51422=CARTESIAN_POINT('Ctrl Pts',(4.83578055685505,21.5525165407171,-25.5464973559168));
#51423=CARTESIAN_POINT('Ctrl Pts',(5.71990630918781,21.5875843019598,-25.5177015341715));
#51424=CARTESIAN_POINT('Ctrl Pts',(6.54861467977253,21.5899024265319,-25.5158130206185));
#51425=CARTESIAN_POINT('Ctrl Pts',(7.19737718820032,21.5199952205941,-25.572922103257));
#51426=CARTESIAN_POINT('Ctrl Pts',(7.32533517773902,21.5058054333461,-25.5847352647941));
#51427=CARTESIAN_POINT('Ctrl Pts',(7.5287921094654,21.4818075562725,-25.6050786014901));
#51428=CARTESIAN_POINT('Ctrl Pts',(7.73064555922848,21.4561637232329,-25.6270995800213));
#51429=CARTESIAN_POINT('Ctrl Pts',(8.14007691415316,21.4000011169923,-25.6755745536324));
#51430=CARTESIAN_POINT('Ctrl Pts',(8.76314309124191,21.2960181027815,-25.7653002467248));
#51431=CARTESIAN_POINT('Ctrl Pts',(9.4626157237208,21.1278957466071,-25.9040486107134));
#51432=CARTESIAN_POINT('Ctrl Pts',(10.0174850844879,20.9503131071729,-26.0442833898104));
#51433=CARTESIAN_POINT('Ctrl Pts',(10.2917439720134,20.8451238836403,-26.1251447081148));
#51434=CARTESIAN_POINT('Ctrl Pts',(11.0595344553679,20.5214871941961,-26.3704086438438));
#51435=CARTESIAN_POINT('Ctrl Pts',(12.2112380684354,19.8253512247695,-26.9121436740289));
#51436=CARTESIAN_POINT('Ctrl Pts',(13.2033849117556,18.9800507080956,-27.5171566231235));
#51437=CARTESIAN_POINT('Ctrl Pts',(13.9587773933514,18.2915509251392,-27.961398750055));
#51438=CARTESIAN_POINT('Ctrl Pts',(14.5428578718472,17.6981445922241,-28.3395188819555));
#51439=CARTESIAN_POINT('Ctrl Pts',(15.5916238649149,16.4391156082604,-29.1041678052385));
#51440=CARTESIAN_POINT('Ctrl Pts',(16.312400049336,15.4069402374363,-29.668803308567));
#51441=CARTESIAN_POINT('Ctrl Pts',(17.056455937744,14.2976159276549,-30.1984376782621));
#51442=CARTESIAN_POINT('Ctrl Pts',(17.6163953201452,13.3949790764644,-30.6123038825733));
#51443=CARTESIAN_POINT('Ctrl Pts',(18.6452863355316,11.5178862779835,-31.3895589768448));
#51444=CARTESIAN_POINT('Ctrl Pts',(19.3595097225576,10.0270239113276,-31.8973975158089));
#51445=CARTESIAN_POINT('Ctrl Pts',(20.1009956523856,8.43910743895403,-32.3304198138232));
#51446=CARTESIAN_POINT('Ctrl Pts',(20.6467087769493,7.19557321337572,-32.6373262144115));
#51447=CARTESIAN_POINT('Ctrl Pts',(21.6664645546449,4.63991827379282,-33.1285294116352));
#51448=CARTESIAN_POINT('Ctrl Pts',(22.3810936914814,2.66633276714268,-33.3391354765121));
#51449=CARTESIAN_POINT('Ctrl Pts',(23.5117886219139,-0.463686149823179,
-33.4478182016441));
#51450=CARTESIAN_POINT('Ctrl Pts',(24.1480627906507,-2.34324698531702,-33.355023097548));
#51451=CARTESIAN_POINT('Ctrl Pts',(24.7493903499091,-4.24322991552065,-33.1044542694871));
#51452=CARTESIAN_POINT('Ctrl Pts',(2.09999999999998,25.0133605092774,-29.9222740658437));
#51453=CARTESIAN_POINT('Ctrl Pts',(2.73333333333332,25.0133605092774,-29.9222740658437));
#51454=CARTESIAN_POINT('Ctrl Pts',(3.36472971107534,25.013251165713,-29.9223277377518));
#51455=CARTESIAN_POINT('Ctrl Pts',(4.12099543456558,25.0132219827751,-29.9223407668436));
#51456=CARTESIAN_POINT('Ctrl Pts',(4.34472654423455,25.0167312931454,-29.9194727333837));
#51457=CARTESIAN_POINT('Ctrl Pts',(4.82887687085582,25.0335070742804,-29.9057944106773));
#51458=CARTESIAN_POINT('Ctrl Pts',(5.71369265357388,25.0746209309229,-29.8722994997285));
#51459=CARTESIAN_POINT('Ctrl Pts',(6.55595753081649,25.0778849396657,-29.8696640285394));
#51460=CARTESIAN_POINT('Ctrl Pts',(7.21857014796824,24.9940353943491,-29.9376703562618));
#51461=CARTESIAN_POINT('Ctrl Pts',(7.34669496716987,24.9773954267909,-29.9514140474994));
#51462=CARTESIAN_POINT('Ctrl Pts',(7.55201908987345,24.9490050308752,-29.9752888612808));
#51463=CARTESIAN_POINT('Ctrl Pts',(7.75538136776272,24.9187155839832,-30.0010890760549));
#51464=CARTESIAN_POINT('Ctrl Pts',(8.16852342416032,24.852261565673,-30.0579755062707));
#51465=CARTESIAN_POINT('Ctrl Pts',(8.79787876017354,24.7290969956901,-30.1633810071747));
#51466=CARTESIAN_POINT('Ctrl Pts',(9.50485227440166,24.5297789011458,-30.3265656499729));
#51467=CARTESIAN_POINT('Ctrl Pts',(10.0642596293231,24.3199216659945,-30.4910276389621));
#51468=CARTESIAN_POINT('Ctrl Pts',(10.3399826652695,24.1960548694606,-30.5855364272996));
#51469=CARTESIAN_POINT('Ctrl Pts',(11.1101489081078,23.8160012772372,-30.871434727323));
#51470=CARTESIAN_POINT('Ctrl Pts',(12.2544520762226,23.0072865685853,-31.4960965077243));
#51471=CARTESIAN_POINT('Ctrl Pts',(13.2427910811612,22.0238011148559,-32.1947581271007));
#51472=CARTESIAN_POINT('Ctrl Pts',(13.9963706129132,21.2205661293469,-32.7087935562777));
#51473=CARTESIAN_POINT('Ctrl Pts',(14.5753869953058,20.5339755367801,-33.1430744875865));
#51474=CARTESIAN_POINT('Ctrl Pts',(15.6192748726438,19.0705105601026,-34.025466524286));
#51475=CARTESIAN_POINT('Ctrl Pts',(16.3374370627988,17.8688444541749,-34.678170573092));
#51476=CARTESIAN_POINT('Ctrl Pts',(17.0806842060506,16.573933856076,-35.2914329668221));
#51477=CARTESIAN_POINT('Ctrl Pts',(17.6370784162494,15.52656213101,-35.7679955458421));
#51478=CARTESIAN_POINT('Ctrl Pts',(18.6628686849426,13.3407406140021,-36.6661078330889));
#51479=CARTESIAN_POINT('Ctrl Pts',(19.3755242818045,11.6037884542861,-37.2528622744394));
#51480=CARTESIAN_POINT('Ctrl Pts',(20.1166807260025,9.75072239293528,-37.7530069912839));
#51481=CARTESIAN_POINT('Ctrl Pts',(20.6600607371703,8.30504525023832,-38.1060328053929));
#51482=CARTESIAN_POINT('Ctrl Pts',(21.6778468485764,5.32712143347218,-38.6712798616524));
#51483=CARTESIAN_POINT('Ctrl Pts',(22.3918418174935,3.02641427127417,-38.9118000510999));
#51484=CARTESIAN_POINT('Ctrl Pts',(23.5225304573588,-0.625454001463374,
-39.0305666347567));
#51485=CARTESIAN_POINT('Ctrl Pts',(24.157514841919,-2.81332401857134,-38.9179235041683));
#51486=CARTESIAN_POINT('Ctrl Pts',(24.7577717974218,-5.02641089220852,-38.6216026000469));
#51487=CARTESIAN_POINT('',(24.5,-0.653978160124863,-9.69209888145294));
#51488=CARTESIAN_POINT('Ctrl Pts',(24.5,-0.653978160124861,-9.69209888145294));
#51489=CARTESIAN_POINT('Ctrl Pts',(23.8274939346292,-0.0568713776825579,
-9.92072428837519));
#51490=CARTESIAN_POINT('Ctrl Pts',(23.3366347313518,0.36306026833911,-10.07387674794));
#51491=CARTESIAN_POINT('Ctrl Pts',(22.5855494187791,1.01440792710674,-10.3088927153609));
#51492=CARTESIAN_POINT('Ctrl Pts',(22.2454144272946,1.30937592429666,-10.4153215760233));
#51493=CARTESIAN_POINT('Ctrl Pts',(21.8382660744817,1.67447889633593,-10.5406724665088));
#51494=CARTESIAN_POINT('Ctrl Pts',(21.3802156950691,2.09338387047635,-10.6833058014315));
#51495=CARTESIAN_POINT('Ctrl Pts',(20.7694693293112,2.65193529200826,-10.8734874819961));
#51496=CARTESIAN_POINT('Ctrl Pts',(20.1629003033437,3.21491192658957,-11.0664040289027));
#51497=CARTESIAN_POINT('Ctrl Pts',(19.5574857571565,3.76869085487531,-11.2860183244349));
#51498=CARTESIAN_POINT('Ctrl Pts',(18.6418529411432,4.60622963346666,-11.6181643838934));
#51499=CARTESIAN_POINT('Ctrl Pts',(17.7734813312658,5.48886970291495,-11.9591596836358));
#51500=CARTESIAN_POINT('Ctrl Pts',(16.962125309523,6.31350499047669,-12.3453577907039));
#51501=CARTESIAN_POINT('Ctrl Pts',(16.8133360659434,6.46472943126141,-12.4161801210775));
#51502=CARTESIAN_POINT('Ctrl Pts',(16.665620536455,6.61523128891394,-12.4887778929881));
#51503=CARTESIAN_POINT('Ctrl Pts',(16.5183901926363,6.7654651816002,-12.5635998093483));
#51504=CARTESIAN_POINT('Ctrl Pts',(15.7264522886975,7.57355888693799,-12.9660597240242));
#51505=CARTESIAN_POINT('Ctrl Pts',(14.9462259719268,8.45630023657397,-13.3952652048773));
#51506=CARTESIAN_POINT('Ctrl Pts',(14.2963150414942,9.19178199464821,-13.806242544063));
#51507=CARTESIAN_POINT('Ctrl Pts',(13.990835093413,9.53748310344734,-13.9994156857325));
#51508=CARTESIAN_POINT('Ctrl Pts',(13.7077063566926,9.85948540296888,-14.1905588167449));
#51509=CARTESIAN_POINT('Ctrl Pts',(13.4460198946299,10.1567774063765,-14.377323000521));
#51510=CARTESIAN_POINT('Ctrl Pts',(12.8373295404644,10.8482872896864,-14.811741947042));
#51511=CARTESIAN_POINT('Ctrl Pts',(12.3530827408093,11.4368508716292,-15.185241342805));
#51512=CARTESIAN_POINT('Ctrl Pts',(11.9770275686809,11.8938113412781,-15.4929541616242));
#51513=CARTESIAN_POINT('Ctrl Pts',(11.6553972428173,12.2846378892233,-15.756133028781));
#51514=CARTESIAN_POINT('Ctrl Pts',(11.368420561492,12.6371055267151,-16.0048905246756));
#51515=CARTESIAN_POINT('Ctrl Pts',(11.0710856781083,13.0022863177644,-16.2795265088952));
#51516=CARTESIAN_POINT('Ctrl Pts',(10.8141787015496,13.31781435759,-16.5168209008521));
#51517=CARTESIAN_POINT('Ctrl Pts',(10.557680266175,13.633060973974,-16.766807974016));
#51518=CARTESIAN_POINT('Ctrl Pts',(10.2957959918397,13.9533753754527,-17.0392327535223));
#51519=CARTESIAN_POINT('Ctrl Pts',(9.71459276345166,14.6642533566189,-17.643828664231));
#51520=CARTESIAN_POINT('Ctrl Pts',(9.09527967376015,15.4163405024385,-18.3675428588812));
#51521=CARTESIAN_POINT('Ctrl Pts',(8.43168033652333,16.2610296723031,-19.2501379487015));
#51522=CARTESIAN_POINT('Ctrl Pts',(7.97964340480089,16.836423105025,-19.8513524978554));
#51523=CARTESIAN_POINT('Ctrl Pts',(7.52291961074422,17.4368467103674,-20.5091832448366));
#51524=CARTESIAN_POINT('Ctrl Pts',(7.10363554125516,18.0137184170276,-21.1546025206863));
#51525=CARTESIAN_POINT('Ctrl Pts',(6.56327799554033,18.7571689849997,-21.9863946187741));
#51526=CARTESIAN_POINT('Ctrl Pts',(6.08559840020807,19.4238605072403,-22.8142482171243));
#51527=CARTESIAN_POINT('Ctrl Pts',(5.61708670825923,20.1096693259461,-23.6903418871945));
#51528=CARTESIAN_POINT('Ctrl Pts',(5.04102956502001,20.9529034985418,-24.7675402270935));
#51529=CARTESIAN_POINT('Ctrl Pts',(4.50102820502495,21.7942496273475,-25.8856366973652));
#51530=CARTESIAN_POINT('Ctrl Pts',(4.00000000000001,22.6717457083367,-26.9859819793801));
#51531=CARTESIAN_POINT('Ctrl Pts',(3.72183418897161,23.1589226907791,-27.5968825927851));
#51532=CARTESIAN_POINT('Ctrl Pts',(3.45538353518261,23.6483861031357,-28.2106502986174));
#51533=CARTESIAN_POINT('Ctrl Pts',(3.2,24.1401481407882,-28.8273003894017));
#51534=CARTESIAN_POINT('',(24.5,-2.74456356862312,-26.8601446537018));
#51535=CARTESIAN_POINT('Ctrl Pts',(24.5,-2.74456356862309,-26.8601446537018));
#51536=CARTESIAN_POINT('Ctrl Pts',(24.5,-2.60355257661784,-25.6295076340102));
#51537=CARTESIAN_POINT('Ctrl Pts',(24.5,-2.46403488201538,-24.4198369473708));
#51538=CARTESIAN_POINT('Ctrl Pts',(24.5,-1.8827407509511,-19.4217612240443));
#51539=CARTESIAN_POINT('Ctrl Pts',(24.5,-1.25682129644897,-14.1166108279068));
#51540=CARTESIAN_POINT('Ctrl Pts',(24.5,-0.653978160124862,-9.69209888145293));
#51541=CARTESIAN_POINT('',(10.2670750393577,21.2938329649397,-26.7016219748491));
#51542=CARTESIAN_POINT('Ctrl Pts',(10.2670750393577,21.2938329649397,-26.7016219748491));
#51543=CARTESIAN_POINT('Ctrl Pts',(11.2293198185888,20.3809543843202,-26.3034024647587));
#51544=CARTESIAN_POINT('Ctrl Pts',(12.092802582344,19.4083234525969,-26.1769225550568));
#51545=CARTESIAN_POINT('Ctrl Pts',(14.3080979519049,16.7229516930375,-26.1226250533543));
#51546=CARTESIAN_POINT('Ctrl Pts',(14.8952017874601,15.9502790457014,-26.200370237811));
#51547=CARTESIAN_POINT('Ctrl Pts',(17.0803363586062,12.6346433376763,-26.6151103878942));
#51548=CARTESIAN_POINT('Ctrl Pts',(17.6922811489506,11.6274647466155,-26.7485362699767));
#51549=CARTESIAN_POINT('Ctrl Pts',(19.0755427322033,9.15735669344811,-27.067694655141));
#51550=CARTESIAN_POINT('Ctrl Pts',(20.2687424742408,6.9356814778935,-27.3229116595642));
#51551=CARTESIAN_POINT('Ctrl Pts',(22.3267279388309,2.40858489185046,-27.4185519724605));
#51552=CARTESIAN_POINT('Ctrl Pts',(23.4192562717209,-0.0469403629655241,
-27.32111731319));
#51553=CARTESIAN_POINT('Ctrl Pts',(24.5,-2.74456356862309,-26.8601446537018));
#51554=CARTESIAN_POINT('Ctrl Pts',(6.,25.0681110272506,-29.8762415562171));
#51555=CARTESIAN_POINT('Ctrl Pts',(7.51604047332548,23.7203706882541,-28.1913747515183));
#51556=CARTESIAN_POINT('Ctrl Pts',(9.08449301626627,22.3720336796495,-27.2810033999414));
#51557=CARTESIAN_POINT('Ctrl Pts',(9.8624969752411,21.6716883636697,-26.8795174907072));
#51558=CARTESIAN_POINT('Ctrl Pts',(10.0667253012217,21.4839041282495,-26.7845355705259));
#51559=CARTESIAN_POINT('Ctrl Pts',(10.2670750393577,21.2938329649397,-26.7016219748491));
#51560=CARTESIAN_POINT('Origin',(24.5,5.29966331579923,-6.64556760097826));
#51561=CARTESIAN_POINT('',(24.5,-3.12544889498789,-9.19761041611355));
#51562=CARTESIAN_POINT('Ctrl Pts',(24.5,-3.12544889498789,-9.19761041611355));
#51563=CARTESIAN_POINT('Ctrl Pts',(24.5,-2.86474614381472,-9.2862000702423));
#51564=CARTESIAN_POINT('Ctrl Pts',(24.5,-2.60012121793576,-9.36375841858885));
#51565=CARTESIAN_POINT('Ctrl Pts',(24.5,-1.78027869528961,-9.56652528394258));
#51566=CARTESIAN_POINT('Ctrl Pts',(24.5,-1.21867492867614,-9.65399574628659));
#51567=CARTESIAN_POINT('Ctrl Pts',(24.5,-0.653978160124863,-9.69209888145294));
#51568=CARTESIAN_POINT('',(24.5,-7.88307893260268,-25.8235757892348));
#51569=CARTESIAN_POINT('Ctrl Pts',(24.5,-3.12544889498789,-9.19761041611355));
#51570=CARTESIAN_POINT('Ctrl Pts',(24.5,-4.24788855647684,-13.3567531368014));
#51571=CARTESIAN_POINT('Ctrl Pts',(24.5,-5.84332298292785,-18.8793734697304));
#51572=CARTESIAN_POINT('Ctrl Pts',(24.5,-7.88307893260268,-25.8235757892348));
#51573=CARTESIAN_POINT('Origin',(24.5,0.,0.));
#51574=CARTESIAN_POINT('Ctrl Pts',(24.5,-7.88307920268519,-25.8235757067876));
#51575=CARTESIAN_POINT('Ctrl Pts',(24.5,5.71692116672878,-29.9752037108234));
#51576=CARTESIAN_POINT('Ctrl Pts',(24.5,16.8342246501858,-21.1094500266368));
#51577=CARTESIAN_POINT('Ctrl Pts',(24.5,37.9436746768226,-4.27522537645101));
#51578=CARTESIAN_POINT('Ctrl Pts',(24.5,21.1094500266368,16.8342246501858));
#51579=CARTESIAN_POINT('Ctrl Pts',(24.5,4.27522537645101,37.9436746768226));
#51580=CARTESIAN_POINT('Ctrl Pts',(24.5,-16.8342246501858,21.1094500266368));
#51581=CARTESIAN_POINT('Ctrl Pts',(24.5,-37.9436746768226,4.27522537645101));
#51582=CARTESIAN_POINT('Ctrl Pts',(24.5,-21.1094500266368,-16.8342246501858));
#51583=CARTESIAN_POINT('Ctrl Pts',(24.5,-15.8898724606626,-23.3793678972715));
#51584=CARTESIAN_POINT('Ctrl Pts',(24.5,-7.88307920268519,-25.8235757067876));
#51585=CARTESIAN_POINT('Ctrl Pts',(24.3078118955742,-7.89265172758991,-25.8549336083419));
#51586=CARTESIAN_POINT('Ctrl Pts',(24.3078118955742,5.72386329794929,-30.0116029878912));
#51587=CARTESIAN_POINT('Ctrl Pts',(24.3078118955742,16.8546666666329,-21.1350835044834));
#51588=CARTESIAN_POINT('Ctrl Pts',(24.3078118955742,37.9897501711163,-4.28041683785043));
#51589=CARTESIAN_POINT('Ctrl Pts',(24.3078118955742,21.1350835044834,16.8546666666329));
#51590=CARTESIAN_POINT('Ctrl Pts',(24.3078118955742,4.28041683785043,37.9897501711163));
#51591=CARTESIAN_POINT('Ctrl Pts',(24.3078118955742,-16.8546666666329,21.1350835044834));
#51592=CARTESIAN_POINT('Ctrl Pts',(24.3078118955742,-37.9897501711163,4.28041683785043));
#51593=CARTESIAN_POINT('Ctrl Pts',(24.3078118955742,-21.1350835044834,-16.8546666666329));
#51594=CARTESIAN_POINT('Ctrl Pts',(24.3078118955742,-15.9091677380474,-23.4077577657098));
#51595=CARTESIAN_POINT('Ctrl Pts',(24.3078118955742,-7.89265172758991,-25.8549336083419));
#51596=CARTESIAN_POINT('Ctrl Pts',(23.9225830034177,-7.91301273816933,-25.9216326842544));
#51597=CARTESIAN_POINT('Ctrl Pts',(23.9225830034177,5.73862939243657,-30.0890252012401));
#51598=CARTESIAN_POINT('Ctrl Pts',(23.9225830034177,16.8981473697169,-21.1896065816043));
#51599=CARTESIAN_POINT('Ctrl Pts',(23.9225830034177,38.0877539513211,-4.29145921188743));
#51600=CARTESIAN_POINT('Ctrl Pts',(23.9225830034177,21.1896065816043,16.8981473697169));
#51601=CARTESIAN_POINT('Ctrl Pts',(23.9225830034177,4.29145921188743,38.0877539513211));
#51602=CARTESIAN_POINT('Ctrl Pts',(23.9225830034177,-16.8981473697169,21.1896065816043));
#51603=CARTESIAN_POINT('Ctrl Pts',(23.9225830034177,-38.0877539513211,4.29145921188743));
#51604=CARTESIAN_POINT('Ctrl Pts',(23.9225830034177,-21.1896065816043,-16.8981473697169));
#51605=CARTESIAN_POINT('Ctrl Pts',(23.9225830034177,-15.9502092971843,-23.4681437576372));
#51606=CARTESIAN_POINT('Ctrl Pts',(23.9225830034177,-7.91301273816933,-25.9216326842544));
#51607=CARTESIAN_POINT('Ctrl Pts',(23.3421815947946,-7.9472021240383,-26.0336310762095));
#51608=CARTESIAN_POINT('Ctrl Pts',(23.3421815947946,5.76342402137866,-30.2190294520944));
#51609=CARTESIAN_POINT('Ctrl Pts',(23.3421815947946,16.9711584086233,-21.2811595286045));
#51610=CARTESIAN_POINT('Ctrl Pts',(23.3421815947946,38.2523179372279,-4.31000111998122));
#51611=CARTESIAN_POINT('Ctrl Pts',(23.3421815947946,21.2811595286045,16.9711584086233));
#51612=CARTESIAN_POINT('Ctrl Pts',(23.3421815947946,4.31000111998122,38.2523179372279));
#51613=CARTESIAN_POINT('Ctrl Pts',(23.3421815947946,-16.9711584086233,21.2811595286045));
#51614=CARTESIAN_POINT('Ctrl Pts',(23.3421815947946,-38.2523179372279,4.31000111998122));
#51615=CARTESIAN_POINT('Ctrl Pts',(23.3421815947946,-21.2811595286045,-16.9711584086233));
#51616=CARTESIAN_POINT('Ctrl Pts',(23.3421815947946,-16.0191246241775,-23.5695414741716));
#51617=CARTESIAN_POINT('Ctrl Pts',(23.3421815947946,-7.9472021240383,-26.0336310762095));
#51618=CARTESIAN_POINT('Ctrl Pts',(22.5631762070947,-8.00011358475547,-26.2069596799766));
#51619=CARTESIAN_POINT('Ctrl Pts',(22.5631762070947,5.80179616530353,-30.4202239057914));
#51620=CARTESIAN_POINT('Ctrl Pts',(22.5631762070947,17.0841502222764,-21.4228467814061));
#51621=CARTESIAN_POINT('Ctrl Pts',(22.5631762070947,38.5069970036825,-4.33869655912968));
#51622=CARTESIAN_POINT('Ctrl Pts',(22.5631762070947,21.4228467814061,17.0841502222764));
#51623=CARTESIAN_POINT('Ctrl Pts',(22.5631762070947,4.33869655912968,38.5069970036825));
#51624=CARTESIAN_POINT('Ctrl Pts',(22.5631762070947,-17.0841502222764,21.4228467814061));
#51625=CARTESIAN_POINT('Ctrl Pts',(22.5631762070947,-38.5069970036825,4.33869655912968));
#51626=CARTESIAN_POINT('Ctrl Pts',(22.5631762070947,-21.4228467814061,-17.0841502222764));
#51627=CARTESIAN_POINT('Ctrl Pts',(22.5631762070947,-16.1257779180092,-23.7264644828441));
#51628=CARTESIAN_POINT('Ctrl Pts',(22.5631762070947,-8.00011358475547,-26.2069596799766));
#51629=CARTESIAN_POINT('Ctrl Pts',(21.5808622776984,-8.07867607201863,-26.4643165180079));
#51630=CARTESIAN_POINT('Ctrl Pts',(21.5808622776984,5.85877079853982,-30.7189557210115));
#51631=CARTESIAN_POINT('Ctrl Pts',(21.5808622776984,17.2519195070522,-21.633222810393));
#51632=CARTESIAN_POINT('Ctrl Pts',(21.5808622776984,38.8851423174451,-4.38130330334077));
#51633=CARTESIAN_POINT('Ctrl Pts',(21.5808622776984,21.633222810393,17.2519195070522));
#51634=CARTESIAN_POINT('Ctrl Pts',(21.5808622776984,4.38130330334077,38.8851423174451));
#51635=CARTESIAN_POINT('Ctrl Pts',(21.5808622776984,-17.2519195070522,21.633222810393));
#51636=CARTESIAN_POINT('Ctrl Pts',(21.5808622776984,-38.8851423174451,4.38130330334077));
#51637=CARTESIAN_POINT('Ctrl Pts',(21.5808622776984,-21.633222810393,-17.2519195070522));
#51638=CARTESIAN_POINT('Ctrl Pts',(21.5808622776984,-16.2841358224153,-23.9594624326839));
#51639=CARTESIAN_POINT('Ctrl Pts',(21.5808622776984,-8.07867607201863,-26.4643165180079));
#51640=CARTESIAN_POINT('Ctrl Pts',(20.5902243197586,-8.16999801768733,-26.7634710890877));
#51641=CARTESIAN_POINT('Ctrl Pts',(20.5902243197586,5.92499877250238,-31.0662050450771));
#51642=CARTESIAN_POINT('Ctrl Pts',(20.5902243197586,17.4469364679823,-21.8777663445708));
#51643=CARTESIAN_POINT('Ctrl Pts',(20.5902243197586,39.3247028125531,-4.43082987658853));
#51644=CARTESIAN_POINT('Ctrl Pts',(20.5902243197586,21.8777663445708,17.4469364679823));
#51645=CARTESIAN_POINT('Ctrl Pts',(20.5902243197586,4.43082987658853,39.3247028125531));
#51646=CARTESIAN_POINT('Ctrl Pts',(20.5902243197586,-17.4469364679823,21.8777663445708));
#51647=CARTESIAN_POINT('Ctrl Pts',(20.5902243197586,-39.3247028125531,4.43082987658853));
#51648=CARTESIAN_POINT('Ctrl Pts',(20.5902243197586,-21.8777663445708,-17.4469364679823));
#51649=CARTESIAN_POINT('Ctrl Pts',(20.5902243197586,-16.4682128857335,-24.2303019498304));
#51650=CARTESIAN_POINT('Ctrl Pts',(20.5902243197586,-8.16999801768733,-26.7634710890877));
#51651=CARTESIAN_POINT('Ctrl Pts',(19.591895069338,-8.27451080226189,-27.1058365195744));
#51652=CARTESIAN_POINT('Ctrl Pts',(19.591895069338,6.000792930466,-31.4636121911249));
#51653=CARTESIAN_POINT('Ctrl Pts',(19.591895069338,17.6701223131461,-22.157632542334));
#51654=CARTESIAN_POINT('Ctrl Pts',(19.591895069338,39.8277548554801,-4.48751022918787));
#51655=CARTESIAN_POINT('Ctrl Pts',(19.591895069338,22.157632542334,17.6701223131461));
#51656=CARTESIAN_POINT('Ctrl Pts',(19.591895069338,4.48751022918787,39.8277548554801));
#51657=CARTESIAN_POINT('Ctrl Pts',(19.591895069338,-17.6701223131461,22.157632542334));
#51658=CARTESIAN_POINT('Ctrl Pts',(19.591895069338,-39.8277548554801,4.48751022918787));
#51659=CARTESIAN_POINT('Ctrl Pts',(19.591895069338,-22.157632542334,-17.6701223131461));
#51660=CARTESIAN_POINT('Ctrl Pts',(19.591895069338,-16.6788786388865,-24.540262407884));
#51661=CARTESIAN_POINT('Ctrl Pts',(19.591895069338,-8.27451080226189,-27.1058365195744));
#51662=CARTESIAN_POINT('Ctrl Pts',(18.5871162949016,-8.39271031247285,-27.4930372468484));
#51663=CARTESIAN_POINT('Ctrl Pts',(18.5871162949016,6.08651289654117,-31.9130627555549));
#51664=CARTESIAN_POINT('Ctrl Pts',(18.5871162949016,17.9225360029332,-22.47414929801));
#51665=CARTESIAN_POINT('Ctrl Pts',(18.5871162949016,40.3966853009432,-4.55161329507688));
#51666=CARTESIAN_POINT('Ctrl Pts',(18.5871162949016,22.47414929801,17.9225360029332));
#51667=CARTESIAN_POINT('Ctrl Pts',(18.5871162949016,4.55161329507688,40.3966853009432));
#51668=CARTESIAN_POINT('Ctrl Pts',(18.5871162949016,-17.9225360029332,22.47414929801));
#51669=CARTESIAN_POINT('Ctrl Pts',(18.5871162949016,-40.3966853009432,4.55161329507688));
#51670=CARTESIAN_POINT('Ctrl Pts',(18.5871162949016,-22.47414929801,-17.9225360029332));
#51671=CARTESIAN_POINT('Ctrl Pts',(18.5871162949016,-16.9171326375936,-24.8908144908262));
#51672=CARTESIAN_POINT('Ctrl Pts',(18.5871162949016,-8.39271031247285,-27.4930372468484));
#51673=CARTESIAN_POINT('Ctrl Pts',(17.577868433379,-8.52509880948018,-27.9267185897952));
#51674=CARTESIAN_POINT('Ctrl Pts',(17.577868433379,6.18252291766525,-32.4164665733692));
#51675=CARTESIAN_POINT('Ctrl Pts',(17.577868433379,18.2052501102534,-22.8286615754873));
#51676=CARTESIAN_POINT('Ctrl Pts',(17.577868433379,41.0339116857407,-4.62341146523394));
#51677=CARTESIAN_POINT('Ctrl Pts',(17.577868433379,22.8286615754873,18.2052501102534));
#51678=CARTESIAN_POINT('Ctrl Pts',(17.577868433379,4.62341146523394,41.0339116857407));
#51679=CARTESIAN_POINT('Ctrl Pts',(17.577868433379,-18.2052501102534,22.8286615754873));
#51680=CARTESIAN_POINT('Ctrl Pts',(17.577868433379,-41.0339116857407,4.62341146523394));
#51681=CARTESIAN_POINT('Ctrl Pts',(17.577868433379,-22.8286615754873,-18.2052501102534));
#51682=CARTESIAN_POINT('Ctrl Pts',(17.577868433379,-17.1839872864711,-25.2834477877042));
#51683=CARTESIAN_POINT('Ctrl Pts',(17.577868433379,-8.52509880948018,-27.9267185897952));
#51684=CARTESIAN_POINT('Ctrl Pts',(16.5668667015923,-8.67209622266927,-28.4082561629427));
#51685=CARTESIAN_POINT('Ctrl Pts',(16.5668667015923,6.28912753260161,-32.9754204151378));
#51686=CARTESIAN_POINT('Ctrl Pts',(16.5668667015923,18.5191613894625,-23.2222938691605));
#51687=CARTESIAN_POINT('Ctrl Pts',(16.5668667015923,41.7414552586229,-4.703132479698));
#51688=CARTESIAN_POINT('Ctrl Pts',(16.5668667015923,23.2222938691605,18.5191613894625));
#51689=CARTESIAN_POINT('Ctrl Pts',(16.5668667015923,4.703132479698,41.7414552586229));
#51690=CARTESIAN_POINT('Ctrl Pts',(16.5668667015923,-18.5191613894625,23.2222938691605));
#51691=CARTESIAN_POINT('Ctrl Pts',(16.5668667015923,-41.7414552586229,4.703132479698));
#51692=CARTESIAN_POINT('Ctrl Pts',(16.5668667015923,-23.2222938691605,-18.5191613894625));
#51693=CARTESIAN_POINT('Ctrl Pts',(16.5668667015923,-17.480289034502,-25.7194077107917));
#51694=CARTESIAN_POINT('Ctrl Pts',(16.5668667015923,-8.67209622266927,-28.4082561629427));
#51695=CARTESIAN_POINT('Ctrl Pts',(15.5576189940876,-8.83393595783092,-28.9384145624536));
#51696=CARTESIAN_POINT('Ctrl Pts',(15.5576189940876,6.40649601054971,-33.5908118003118));
#51697=CARTESIAN_POINT('Ctrl Pts',(15.5576189940876,18.8647682759327,-23.6556711972172));
#51698=CARTESIAN_POINT('Ctrl Pts',(15.5576189940876,42.5204394731498,-4.79090292128453));
#51699=CARTESIAN_POINT('Ctrl Pts',(15.5576189940876,23.6556711972172,18.8647682759327));
#51700=CARTESIAN_POINT('Ctrl Pts',(15.5576189940876,4.79090292128453,42.5204394731498));
#51701=CARTESIAN_POINT('Ctrl Pts',(15.5576189940876,-18.8647682759327,23.6556711972172));
#51702=CARTESIAN_POINT('Ctrl Pts',(15.5576189940876,-42.5204394731498,4.79090292128453));
#51703=CARTESIAN_POINT('Ctrl Pts',(15.5576189940876,-23.6556711972172,-18.8647682759327));
#51704=CARTESIAN_POINT('Ctrl Pts',(15.5576189940876,-17.80650835625,-26.1993864870359));
#51705=CARTESIAN_POINT('Ctrl Pts',(15.5576189940876,-8.83393595783092,-28.9384145624536));
#51706=CARTESIAN_POINT('Ctrl Pts',(14.5544447688713,-9.01056601144323,-29.5170234339714));
#51707=CARTESIAN_POINT('Ctrl Pts',(14.5544447688713,6.53459063781575,-34.262442986851));
#51708=CARTESIAN_POINT('Ctrl Pts',(14.5544447688713,19.2419597167431,-24.1286543036994));
#51709=CARTESIAN_POINT('Ctrl Pts',(14.5544447688713,43.3706140204425,-4.88669458695624));
#51710=CARTESIAN_POINT('Ctrl Pts',(14.5544447688713,24.1286543036994,19.2419597167431));
#51711=CARTESIAN_POINT('Ctrl Pts',(14.5544447688713,4.88669458695624,43.3706140204425));
#51712=CARTESIAN_POINT('Ctrl Pts',(14.5544447688713,-19.2419597167431,24.1286543036994));
#51713=CARTESIAN_POINT('Ctrl Pts',(14.5544447688713,-43.3706140204425,4.88669458695624));
#51714=CARTESIAN_POINT('Ctrl Pts',(14.5544447688713,-24.1286543036994,-19.2419597167431));
#51715=CARTESIAN_POINT('Ctrl Pts',(14.5544447688713,-18.1625404285478,-26.7232298861623));
#51716=CARTESIAN_POINT('Ctrl Pts',(14.5544447688713,-9.01056601144323,-29.5170234339714));
#51717=CARTESIAN_POINT('Ctrl Pts',(13.5625963827217,-9.20148423244017,-30.1424378192589));
#51718=CARTESIAN_POINT('Ctrl Pts',(13.5625963827217,6.67304724730406,-34.9884045583829));
#51719=CARTESIAN_POINT('Ctrl Pts',(13.5625963827217,19.6496633740883,-24.6398985195302));
#51720=CARTESIAN_POINT('Ctrl Pts',(13.5625963827217,44.2895618936185,-4.99023514544194));
#51721=CARTESIAN_POINT('Ctrl Pts',(13.5625963827217,24.6398985195302,19.6496633740883));
#51722=CARTESIAN_POINT('Ctrl Pts',(13.5625963827217,4.99023514544194,44.2895618936185));
#51723=CARTESIAN_POINT('Ctrl Pts',(13.5625963827217,-19.6496633740883,24.6398985195302));
#51724=CARTESIAN_POINT('Ctrl Pts',(13.5625963827217,-44.2895618936185,4.99023514544194));
#51725=CARTESIAN_POINT('Ctrl Pts',(13.5625963827217,-24.6398985195302,-19.6496633740883));
#51726=CARTESIAN_POINT('Ctrl Pts',(13.5625963827217,-18.5473730686949,-27.2894486456364));
#51727=CARTESIAN_POINT('Ctrl Pts',(13.5625963827217,-9.20148423244017,-30.1424378192589));
#51728=CARTESIAN_POINT('Ctrl Pts',(12.5880795783847,-9.40573585110567,-30.8115300612911));
#51729=CARTESIAN_POINT('Ctrl Pts',(12.5880795783847,6.82117342643589,-35.7650660278856));
#51730=CARTESIAN_POINT('Ctrl Pts',(12.5880795783847,20.0858403482595,-25.1868471453426));
#51731=CARTESIAN_POINT('Ctrl Pts',(12.5880795783847,45.2726874936021,-5.10100679708315));
#51732=CARTESIAN_POINT('Ctrl Pts',(12.5880795783847,25.1868471453426,20.0858403482595));
#51733=CARTESIAN_POINT('Ctrl Pts',(12.5880795783847,5.10100679708315,45.2726874936021));
#51734=CARTESIAN_POINT('Ctrl Pts',(12.5880795783847,-20.0858403482595,25.1868471453426));
#51735=CARTESIAN_POINT('Ctrl Pts',(12.5880795783847,-45.2726874936021,5.10100679708315));
#51736=CARTESIAN_POINT('Ctrl Pts',(12.5880795783847,-25.1868471453426,-20.0858403482595));
#51737=CARTESIAN_POINT('Ctrl Pts',(12.5880795783847,-18.9590817534653,-27.895211141942));
#51738=CARTESIAN_POINT('Ctrl Pts',(12.5880795783847,-9.40573585110567,-30.8115300612911));
#51739=CARTESIAN_POINT('Ctrl Pts',(11.6370973936883,-9.62212179125491,-31.5203721981841));
#51740=CARTESIAN_POINT('Ctrl Pts',(11.6370973936883,6.97809958810636,-36.587867939342));
#51741=CARTESIAN_POINT('Ctrl Pts',(11.6370973936883,20.5479300259039,-25.766289273552));
#51742=CARTESIAN_POINT('Ctrl Pts',(11.6370973936883,46.3142192994558,-5.21835924764817));
#51743=CARTESIAN_POINT('Ctrl Pts',(11.6370973936883,25.766289273552,20.5479300259039));
#51744=CARTESIAN_POINT('Ctrl Pts',(11.6370973936883,5.21835924764817,46.3142192994558));
#51745=CARTESIAN_POINT('Ctrl Pts',(11.6370973936883,-20.5479300259039,25.766289273552));
#51746=CARTESIAN_POINT('Ctrl Pts',(11.6370973936883,-46.3142192994558,5.21835924764817));
#51747=CARTESIAN_POINT('Ctrl Pts',(11.6370973936883,-25.766289273552,-20.5479300259039));
#51748=CARTESIAN_POINT('Ctrl Pts',(11.6370973936883,-19.3952495126426,-28.5369611957563));
#51749=CARTESIAN_POINT('Ctrl Pts',(11.6370973936883,-9.62212179125491,-31.5203721981841));
#51750=CARTESIAN_POINT('Ctrl Pts',(10.7155646400367,-9.84933794718583,-32.2646922098985));
#51751=CARTESIAN_POINT('Ctrl Pts',(10.7155646400367,7.14287997631073,-37.4518514647263));
#51752=CARTESIAN_POINT('Ctrl Pts',(10.7155646400367,21.0331475043468,-26.3747327466602));
#51753=CARTESIAN_POINT('Ctrl Pts',(10.7155646400367,47.4078802510069,-5.34158524231338));
#51754=CARTESIAN_POINT('Ctrl Pts',(10.7155646400367,26.3747327466602,21.0331475043468));
#51755=CARTESIAN_POINT('Ctrl Pts',(10.7155646400367,5.34158524231338,47.4078802510069));
#51756=CARTESIAN_POINT('Ctrl Pts',(10.7155646400367,-21.0331475043468,26.3747327466602));
#51757=CARTESIAN_POINT('Ctrl Pts',(10.7155646400367,-47.4078802510069,5.34158524231338));
#51758=CARTESIAN_POINT('Ctrl Pts',(10.7155646400367,-26.3747327466602,-21.0331475043468));
#51759=CARTESIAN_POINT('Ctrl Pts',(10.7155646400367,-19.8532476686822,-29.2108311347902));
#51760=CARTESIAN_POINT('Ctrl Pts',(10.7155646400367,-9.84933794718583,-32.2646922098985));
#51761=CARTESIAN_POINT('Ctrl Pts',(9.82859575068344,-10.0861224473418,-33.0403564279984));
#51762=CARTESIAN_POINT('Ctrl Pts',(9.82859575068344,7.31459946384724,-38.3522183702525));
#51763=CARTESIAN_POINT('Ctrl Pts',(9.82859575068344,21.5387980714436,-27.0087985025163));
#51764=CARTESIAN_POINT('Ctrl Pts',(9.82859575068344,48.5475965739599,-5.47000043107263));
#51765=CARTESIAN_POINT('Ctrl Pts',(9.82859575068344,27.0087985025163,21.5387980714436));
#51766=CARTESIAN_POINT('Ctrl Pts',(9.82859575068344,5.47000043107263,48.5475965739599));
#51767=CARTESIAN_POINT('Ctrl Pts',(9.82859575068344,-21.5387980714436,27.0087985025163));
#51768=CARTESIAN_POINT('Ctrl Pts',(9.82859575068344,-48.5475965739599,5.47000043107263));
#51769=CARTESIAN_POINT('Ctrl Pts',(9.82859575068344,-27.0087985025163,-21.5387980714436));
#51770=CARTESIAN_POINT('Ctrl Pts',(9.82859575068344,-20.3305326751374,-29.913078543345));
#51771=CARTESIAN_POINT('Ctrl Pts',(9.82859575068344,-10.0861224473418,-33.0403564279984));
#51772=CARTESIAN_POINT('Ctrl Pts',(8.97989469943246,-10.3313960385027,-33.8438294094779));
#51773=CARTESIAN_POINT('Ctrl Pts',(8.97989469943246,7.49247536092943,-39.2848648236118));
#51774=CARTESIAN_POINT('Ctrl Pts',(8.97989469943246,22.0625769943999,-27.6655964976071));
#51775=CARTESIAN_POINT('Ctrl Pts',(8.97989469943246,49.7281734920069,-5.6030195032072));
#51776=CARTESIAN_POINT('Ctrl Pts',(8.97989469943246,27.6655964976071,22.0625769943999));
#51777=CARTESIAN_POINT('Ctrl Pts',(8.97989469943246,5.6030195032072,49.7281734920069));
#51778=CARTESIAN_POINT('Ctrl Pts',(8.97989469943246,-22.0625769943999,27.6655964976071));
#51779=CARTESIAN_POINT('Ctrl Pts',(8.97989469943246,-49.7281734920069,5.6030195032072));
#51780=CARTESIAN_POINT('Ctrl Pts',(8.97989469943246,-27.6655964976071,-22.0625769943999));
#51781=CARTESIAN_POINT('Ctrl Pts',(8.97989469943246,-20.8249290881771,-30.6405026089669));
#51782=CARTESIAN_POINT('Ctrl Pts',(8.97989469943246,-10.3313960385027,-33.8438294094779));
#51783=CARTESIAN_POINT('Ctrl Pts',(8.1713316609345,-10.5843692822308,-34.6725250933902));
#51784=CARTESIAN_POINT('Ctrl Pts',(8.1713316609345,7.6759351555732,-40.2467890056693));
#51785=CARTESIAN_POINT('Ctrl Pts',(8.1713316609345,22.6027984365432,-28.3430127596098));
#51786=CARTESIAN_POINT('Ctrl Pts',(8.1713316609345,50.945811196153,-5.74021432306657));
#51787=CARTESIAN_POINT('Ctrl Pts',(8.1713316609345,28.3430127596098,22.6027984365432));
#51788=CARTESIAN_POINT('Ctrl Pts',(8.1713316609345,5.74021432306657,50.945811196153));
#51789=CARTESIAN_POINT('Ctrl Pts',(8.1713316609345,-22.6027984365432,28.3430127596098));
#51790=CARTESIAN_POINT('Ctrl Pts',(8.1713316609345,-50.945811196153,5.74021432306657));
#51791=CARTESIAN_POINT('Ctrl Pts',(8.1713316609345,-28.3430127596098,-22.6027984365432));
#51792=CARTESIAN_POINT('Ctrl Pts',(8.1713316609345,-21.3348456417785,-31.3907620420157));
#51793=CARTESIAN_POINT('Ctrl Pts',(8.1713316609345,-10.5843692822308,-34.6725250933902));
#51794=CARTESIAN_POINT('Ctrl Pts',(7.40358438374929,-10.8444940039127,-35.5246477564824));
#51795=CARTESIAN_POINT('Ctrl Pts',(7.40358438374929,7.86458130375168,-41.23590649671));
#51796=CARTESIAN_POINT('Ctrl Pts',(7.40358438374929,23.1582917773139,-29.039579376772));
#51797=CARTESIAN_POINT('Ctrl Pts',(7.40358438374929,52.1978711540859,-5.88128759945807));
#51798=CARTESIAN_POINT('Ctrl Pts',(7.40358438374929,29.039579376772,23.1582917773139));
#51799=CARTESIAN_POINT('Ctrl Pts',(7.40358438374929,5.88128759945807,52.1978711540859));
#51800=CARTESIAN_POINT('Ctrl Pts',(7.40358438374929,-23.1582917773139,29.039579376772));
#51801=CARTESIAN_POINT('Ctrl Pts',(7.40358438374929,-52.1978711540859,5.88128759945807));
#51802=CARTESIAN_POINT('Ctrl Pts',(7.40358438374929,-29.039579376772,-23.1582917773139));
#51803=CARTESIAN_POINT('Ctrl Pts',(7.40358438374929,-21.8591773838701,-32.1622310848871));
#51804=CARTESIAN_POINT('Ctrl Pts',(7.40358438374929,-10.8444940039127,-35.5246477564824));
#51805=CARTESIAN_POINT('Ctrl Pts',(6.82198164612729,-11.058045141737,-36.2242035814446));
#51806=CARTESIAN_POINT('Ctrl Pts',(6.82198164612729,8.01945162645387,-42.0479291460297));
#51807=CARTESIAN_POINT('Ctrl Pts',(6.82198164612729,23.6143277673129,-29.6114304207775));
#51808=CARTESIAN_POINT('Ctrl Pts',(6.82198164612729,53.2257581880904,-5.99710265346456));
#51809=CARTESIAN_POINT('Ctrl Pts',(6.82198164612729,29.6114304207775,23.6143277673129));
#51810=CARTESIAN_POINT('Ctrl Pts',(6.82198164612729,5.99710265346456,53.2257581880904));
#51811=CARTESIAN_POINT('Ctrl Pts',(6.82198164612729,-23.6143277673129,29.6114304207775));
#51812=CARTESIAN_POINT('Ctrl Pts',(6.82198164612729,-53.2257581880904,5.99710265346456));
#51813=CARTESIAN_POINT('Ctrl Pts',(6.82198164612729,-29.6114304207775,-23.6143277673129));
#51814=CARTESIAN_POINT('Ctrl Pts',(6.82198164612729,-22.2896310500849,-32.7955737784852));
#51815=CARTESIAN_POINT('Ctrl Pts',(6.82198164612729,-11.058045141737,-36.2242035814446));
#51816=CARTESIAN_POINT('Ctrl Pts',(6.40395249919757,-11.2211992099643,-36.7586675040324));
#51817=CARTESIAN_POINT('Ctrl Pts',(6.40395249919757,8.13777327743625,-42.6683182485135));
#51818=CARTESIAN_POINT('Ctrl Pts',(6.40395249919757,23.9627413968746,-30.048327293349));
#51819=CARTESIAN_POINT('Ctrl Pts',(6.40395249919757,54.0110686902236,-6.08558589647434));
#51820=CARTESIAN_POINT('Ctrl Pts',(6.40395249919757,30.048327293349,23.9627413968746));
#51821=CARTESIAN_POINT('Ctrl Pts',(6.40395249919757,6.08558589647434,54.0110686902236));
#51822=CARTESIAN_POINT('Ctrl Pts',(6.40395249919757,-23.9627413968746,30.048327293349));
#51823=CARTESIAN_POINT('Ctrl Pts',(6.40395249919757,-54.0110686902236,6.08558589647434));
#51824=CARTESIAN_POINT('Ctrl Pts',(6.40395249919757,-30.048327293349,-23.9627413968746));
#51825=CARTESIAN_POINT('Ctrl Pts',(6.40395249919757,-22.6184996646089,-33.2794505589853));
#51826=CARTESIAN_POINT('Ctrl Pts',(6.40395249919757,-11.2211992099643,-36.7586675040324));
#51827=CARTESIAN_POINT('Ctrl Pts',(6.13331019225912,-11.3312924070318,-37.1193133806217));
#51828=CARTESIAN_POINT('Ctrl Pts',(6.13331019225912,8.21761442991556,-43.086944767977));
#51829=CARTESIAN_POINT('Ctrl Pts',(6.13331019225912,24.1978441485076,-30.3431368191721));
#51830=CARTESIAN_POINT('Ctrl Pts',(6.13331019225912,54.5409809676797,-6.14529267066448));
#51831=CARTESIAN_POINT('Ctrl Pts',(6.13331019225912,30.3431368191721,24.1978441485076));
#51832=CARTESIAN_POINT('Ctrl Pts',(6.13331019225912,6.14529267066448,54.5409809676797));
#51833=CARTESIAN_POINT('Ctrl Pts',(6.13331019225912,-24.1978441485076,30.3431368191721));
#51834=CARTESIAN_POINT('Ctrl Pts',(6.13331019225912,-54.5409809676797,6.14529267066448));
#51835=CARTESIAN_POINT('Ctrl Pts',(6.13331019225912,-30.3431368191721,-24.1978441485076));
#51836=CARTESIAN_POINT('Ctrl Pts',(6.13331019225912,-22.8404138196251,-33.6059612144093));
#51837=CARTESIAN_POINT('Ctrl Pts',(6.13331019225912,-11.3312924070318,-37.1193133806217));
#51838=CARTESIAN_POINT('Ctrl Pts',(6.,-11.3866699594342,-37.3007204653599));
#51839=CARTESIAN_POINT('Ctrl Pts',(6.,8.25777501860823,-43.2975164711894));
#51840=CARTESIAN_POINT('Ctrl Pts',(6.,24.3161022724906,-30.4914278162532));
#51841=CARTESIAN_POINT('Ctrl Pts',(6.,54.8075300887437,-6.17532554376256));
#51842=CARTESIAN_POINT('Ctrl Pts',(6.,30.4914278162532,24.3161022724906));
#51843=CARTESIAN_POINT('Ctrl Pts',(6.,6.17532554376256,54.8075300887437));
#51844=CARTESIAN_POINT('Ctrl Pts',(6.,-24.3161022724906,30.4914278162532));
#51845=CARTESIAN_POINT('Ctrl Pts',(6.,-54.8075300887437,6.17532554376256));
#51846=CARTESIAN_POINT('Ctrl Pts',(6.,-30.4914278162532,-24.3161022724906));
#51847=CARTESIAN_POINT('Ctrl Pts',(6.,-22.9520379987349,-33.7701980738366));
#51848=CARTESIAN_POINT('Ctrl Pts',(6.,-11.3866699594342,-37.3007204653599));
#51849=CARTESIAN_POINT('Ctrl Pts',(24.5,-7.88307893260267,-25.8235757892348));
#51850=CARTESIAN_POINT('Ctrl Pts',(23.5178991898112,-5.12440787864319,-26.8408810021941));
#51851=CARTESIAN_POINT('Ctrl Pts',(22.3947886245986,-2.29122169990625,-27.4715439015176));
#51852=CARTESIAN_POINT('Ctrl Pts',(21.1743874927566,0.532981741024215,-27.7985414433729));
#51853=CARTESIAN_POINT('Ctrl Pts',(20.5031871793438,2.08624663502909,-27.9783846497186));
#51854=CARTESIAN_POINT('Ctrl Pts',(19.8411792966416,3.6507154806329,-28.0507750408847));
#51855=CARTESIAN_POINT('Ctrl Pts',(19.1295827650275,5.18988031863482,-28.0566862810056));
#51856=CARTESIAN_POINT('Ctrl Pts',(18.8261415870923,5.84621571479024,-28.0592069701682));
#51857=CARTESIAN_POINT('Ctrl Pts',(18.5104994276276,6.50331037286216,-28.0498981370496));
#51858=CARTESIAN_POINT('Ctrl Pts',(18.2016639423759,7.11415464453783,-28.0364358938641));
#51859=CARTESIAN_POINT('Ctrl Pts',(17.6747132403632,8.15640799025529,-28.013465934659));
#51860=CARTESIAN_POINT('Ctrl Pts',(17.2016343370993,9.08626906934427,-27.9569617268139));
#51861=CARTESIAN_POINT('Ctrl Pts',(16.872935292646,9.71033923360541,-27.916829044088));
#51862=CARTESIAN_POINT('Ctrl Pts',(16.6342454025477,10.1635174263466,-27.8876860764072));
#51863=CARTESIAN_POINT('Ctrl Pts',(16.5014949770664,10.4082918220469,-27.8702638626044));
#51864=CARTESIAN_POINT('Ctrl Pts',(16.3424569562979,10.698116742743,-27.8501213404638));
#51865=CARTESIAN_POINT('Ctrl Pts',(15.993118510103,11.334738017173,-27.8058768424938));
#51866=CARTESIAN_POINT('Ctrl Pts',(15.6312480487537,11.9648274577435,-27.7609569624451));
#51867=CARTESIAN_POINT('Ctrl Pts',(15.2503296894305,12.58375600882,-27.7280544894048));
#51868=CARTESIAN_POINT('Ctrl Pts',(14.7484414179076,13.3992404114303,-27.684703033853));
#51869=CARTESIAN_POINT('Ctrl Pts',(14.2669345517206,14.1852815321393,-27.6314704530746));
#51870=CARTESIAN_POINT('Ctrl Pts',(13.7912435751455,14.9172443259166,-27.6009121644364));
#51871=CARTESIAN_POINT('Ctrl Pts',(13.5533980868579,15.2832257228053,-27.5856330201174));
#51872=CARTESIAN_POINT('Ctrl Pts',(13.3161115657262,15.6377572992835,-27.5758360909478));
#51873=CARTESIAN_POINT('Ctrl Pts',(13.0766514227367,15.9813914150943,-27.5754070621212));
#51874=CARTESIAN_POINT('Ctrl Pts',(12.9188702359555,16.2078132234764,-27.5751243734174));
#51875=CARTESIAN_POINT('Ctrl Pts',(12.7601526360409,16.4295109353367,-27.5789102998031));
#51876=CARTESIAN_POINT('Ctrl Pts',(12.5997389313808,16.6466716884716,-27.5879931844747));
#51877=CARTESIAN_POINT('Ctrl Pts',(12.5166971934814,16.7590898037572,-27.5926951426389));
#51878=CARTESIAN_POINT('Ctrl Pts',(12.4397215765388,16.861779476413,-27.59820158806));
#51879=CARTESIAN_POINT('Ctrl Pts',(12.3478597934844,16.9819818549666,-27.606669709847));
#51880=CARTESIAN_POINT('Ctrl Pts',(11.9116121727781,17.5528177336491,-27.6468844526771));
#51881=CARTESIAN_POINT('Ctrl Pts',(10.7144663992386,19.17879676418,-27.7119011061896));
#51882=CARTESIAN_POINT('Ctrl Pts',(9.56604185022482,20.3673840450418,-28.2355768679772));
#51883=CARTESIAN_POINT('Ctrl Pts',(9.07284645450855,20.8778274823851,-28.4604714636071));
#51884=CARTESIAN_POINT('Ctrl Pts',(8.57333454992941,21.3352833188185,-28.7628944317207));
#51885=CARTESIAN_POINT('Ctrl Pts',(8.00348148263335,21.8507631464374,-29.1850206512921));
#51886=CARTESIAN_POINT('Ctrl Pts',(7.63919428966136,22.1802914234861,-29.4548712223124));
#51887=CARTESIAN_POINT('Ctrl Pts',(7.24388644384718,22.5359692004009,-29.7845767075602));
#51888=CARTESIAN_POINT('Ctrl Pts',(6.94254646282516,22.8138796544531,-30.0547884375835));
#51889=CARTESIAN_POINT('Ctrl Pts',(6.91433564865254,22.8398970456712,-30.0800850904774));
#51890=CARTESIAN_POINT('Ctrl Pts',(6.88669635040547,22.8654448722984,-30.1050387574276));
#51891=CARTESIAN_POINT('Ctrl Pts',(6.85962514029878,22.8905248103199,-30.129631969423));
#51892=CARTESIAN_POINT('Ctrl Pts',(6.4400006207374,23.279283085308,-30.5108456177005));
#51893=CARTESIAN_POINT('Ctrl Pts',(6.15412442492902,23.5258752447222,-30.8298076941652));
#51894=CARTESIAN_POINT('Ctrl Pts',(6.,23.6628748086085,-31.0011024931715));
#51895=CARTESIAN_POINT('Ctrl Pts',(2.09999999999998,5.34456416452658,-8.14535940885845));
#51896=CARTESIAN_POINT('Ctrl Pts',(2.73333333333332,5.34456416452658,-8.14535940885845));
#51897=CARTESIAN_POINT('Ctrl Pts',(3.36703045510619,5.34460712586018,-8.14533631625124));
#51898=CARTESIAN_POINT('Ctrl Pts',(4.1258438026898,5.34462008683109,-8.14532944421707));
#51899=CARTESIAN_POINT('Ctrl Pts',(4.38280550094044,5.34570783050074,-8.14463189797639));
#51900=CARTESIAN_POINT('Ctrl Pts',(4.88877630191765,5.35053371396832,-8.14154574907976));
#51901=CARTESIAN_POINT('Ctrl Pts',(5.76582860138385,5.36167176813889,-8.13444079857371));
#51902=CARTESIAN_POINT('Ctrl Pts',(6.49307225725675,5.36150896502748,-8.13458573839888));
#51903=CARTESIAN_POINT('Ctrl Pts',(7.02345937097035,5.34325603592381,-8.14610072176819));
#51904=CARTESIAN_POINT('Ctrl Pts',(7.14991970135013,5.33879812318534,-8.14899078713681));
#51905=CARTESIAN_POINT('Ctrl Pts',(7.33710498699582,5.33174922546116,-8.15365385893716));
#51906=CARTESIAN_POINT('Ctrl Pts',(7.52538047832545,5.32413774318376,-8.15876542857883));
#51907=CARTESIAN_POINT('Ctrl Pts',(7.90085937976029,5.30771267984777,-8.16986641378499));
#51908=CARTESIAN_POINT('Ctrl Pts',(8.46131778044036,5.27795323293097,-8.19002168993195));
#51909=CARTESIAN_POINT('Ctrl Pts',(9.06510517903235,5.23166569178312,-8.21981836831304));
#51910=CARTESIAN_POINT('Ctrl Pts',(9.52848763525404,5.18451311071437,-8.24862090594879));
#51911=CARTESIAN_POINT('Ctrl Pts',(9.75208483560215,5.15725817655892,-8.26472591834395));
#51912=CARTESIAN_POINT('Ctrl Pts',(10.3694305746462,5.07483970414387,-8.31257577375928));
#51913=CARTESIAN_POINT('Ctrl Pts',(11.3479755118771,4.89091383636494,-8.42464079424009));
#51914=CARTESIAN_POINT('Ctrl Pts',(12.2739432230502,4.64635231866122,-8.56256142325114));
#51915=CARTESIAN_POINT('Ctrl Pts',(13.0009186596788,4.44074096877511,-8.66574892117875));
#51916=CARTESIAN_POINT('Ctrl Pts',(13.5007657464189,4.28304830756585,-8.74312201390955));
#51917=CARTESIAN_POINT('Ctrl Pts',(14.4712209115036,3.92573756082701,-8.91215537488908));
#51918=CARTESIAN_POINT('Ctrl Pts',(15.1525957863043,3.62734188705641,-9.03883135866711));
#51919=CARTESIAN_POINT('Ctrl Pts',(15.7474668256706,3.35786214483351,-9.13646540471693));
#51920=CARTESIAN_POINT('Ctrl Pts',(16.0037627434752,3.23694584628154,-9.17854126131123));
#51921=CARTESIAN_POINT('Ctrl Pts',(16.5107347057776,2.98182782255615,-9.26366275020945));
#51922=CARTESIAN_POINT('Ctrl Pts',(17.3591246875254,2.51561318345669,-9.40643332398099));
#51923=CARTESIAN_POINT('Ctrl Pts',(18.0498326782835,2.08512110773588,-9.51119006271148));
#51924=CARTESIAN_POINT('Ctrl Pts',(18.7837576316761,1.61772190021554,-9.59472621339316));
#51925=CARTESIAN_POINT('Ctrl Pts',(19.2874983687974,1.27668484968537,-9.6462243441966));
#51926=CARTESIAN_POINT('Ctrl Pts',(20.2705670405104,0.551057000957825,-9.72220562049248));
#51927=CARTESIAN_POINT('Ctrl Pts',(20.968423963075,-0.0130109990231726,
-9.73577142111487));
#51928=CARTESIAN_POINT('Ctrl Pts',(22.6569785206169,-1.37366893882804,-9.67192624996041));
#51929=CARTESIAN_POINT('Ctrl Pts',(23.7241254823866,-2.3362350951335,-9.47253804281166));
#51930=CARTESIAN_POINT('Ctrl Pts',(24.6950729185821,-3.32180370011223,-9.13150534684048));
#51931=CARTESIAN_POINT('Ctrl Pts',(2.09999999999998,7.95334816354381,-11.4166710731552));
#51932=CARTESIAN_POINT('Ctrl Pts',(2.73333333333332,7.95334816354381,-11.4166710731552));
#51933=CARTESIAN_POINT('Ctrl Pts',(3.36722921888214,7.95339083450222,-11.4166436748178));
#51934=CARTESIAN_POINT('Ctrl Pts',(4.12626245611356,7.95340335909069,-11.4166357236622));
#51935=CARTESIAN_POINT('Ctrl Pts',(4.38607734488415,7.95493785056024,-11.4155904452611));
#51936=CARTESIAN_POINT('Ctrl Pts',(4.89393849803322,7.96172076053339,-11.4109823514058));
#51937=CARTESIAN_POINT('Ctrl Pts',(5.77028399864619,7.97732575169866,-11.4004072666733));
#51938=CARTESIAN_POINT('Ctrl Pts',(6.48775133512661,7.97697012330154,-11.4006984916951));
#51939=CARTESIAN_POINT('Ctrl Pts',(7.00649985389096,7.95176660573384,-11.4175960094363));
#51940=CARTESIAN_POINT('Ctrl Pts',(7.1328122089054,7.94552344412315,-11.4218945357638));
#51941=CARTESIAN_POINT('Ctrl Pts',(7.31839339846734,7.93570247397948,-11.4287944424324));
#51942=CARTESIAN_POINT('Ctrl Pts',(7.50532535803233,7.92508991461552,-11.4363618062793));
#51943=CARTESIAN_POINT('Ctrl Pts',(7.87743482519494,7.90221930046077,-11.4527758654708));
#51944=CARTESIAN_POINT('Ctrl Pts',(8.43163383044899,7.86082555090579,-11.4825467102839));
#51945=CARTESIAN_POINT('Ctrl Pts',(9.02557103671809,7.79663844533022,-11.5264740745866));
#51946=CARTESIAN_POINT('Ctrl Pts',(9.47909108553348,7.73146286135872,-11.5688495286329));
#51947=CARTESIAN_POINT('Ctrl Pts',(9.69701368850754,7.69388237767458,-11.5925048579334));
#51948=CARTESIAN_POINT('Ctrl Pts',(10.2970955435366,7.58039638756159,-11.662716724276));
#51949=CARTESIAN_POINT('Ctrl Pts',(11.2524630852568,7.32685330737253,-11.8275326519127));
#51950=CARTESIAN_POINT('Ctrl Pts',(12.1686924220656,6.98608110701113,-12.0331549997054));
#51951=CARTESIAN_POINT('Ctrl Pts',(12.8916733902102,6.69791329894401,-12.1883803970336));
#51952=CARTESIAN_POINT('Ctrl Pts',(13.3792423851727,6.48008047549737,-12.3034763709601));
#51953=CARTESIAN_POINT('Ctrl Pts',(14.3391274674842,5.98209567733816,-12.5578967665008));
#51954=CARTESIAN_POINT('Ctrl Pts',(15.0158575632568,5.56322362445193,-12.7509990333251));
#51955=CARTESIAN_POINT('Ctrl Pts',(15.6096998984311,5.18299682455851,-12.9017952037445));
#51956=CARTESIAN_POINT('Ctrl Pts',(15.8629234378176,5.01414769058628,-12.9665415390874));
#51957=CARTESIAN_POINT('Ctrl Pts',(16.366769191659,4.65589390592607,-13.0986310142571));
#51958=CARTESIAN_POINT('Ctrl Pts',(17.2116336585144,3.99947370123076,-13.3224762399715));
#51959=CARTESIAN_POINT('Ctrl Pts',(17.9015681458004,3.38939186549384,-13.491162196428));
#51960=CARTESIAN_POINT('Ctrl Pts',(18.6346321455063,2.72577662783367,-13.630803315184));
#51961=CARTESIAN_POINT('Ctrl Pts',(19.1381734987811,2.24198588579176,-13.7198489991737));
#51962=CARTESIAN_POINT('Ctrl Pts',(20.1235843849346,1.20814441723857,-13.8612245457287));
#51963=CARTESIAN_POINT('Ctrl Pts',(20.8218560196981,0.402341697820859,-13.9055220555452));
#51964=CARTESIAN_POINT('Ctrl Pts',(22.509656326961,-1.54359381676115,-13.873432467644));
#51965=CARTESIAN_POINT('Ctrl Pts',(23.5814142719248,-2.93009156681438,-13.6326211887675));
#51966=CARTESIAN_POINT('Ctrl Pts',(24.5630597774301,-4.36475478204552,-13.1847221831164));
#51967=CARTESIAN_POINT('Ctrl Pts',(2.09999999999999,14.0405108279174,-19.0497316231808));
#51968=CARTESIAN_POINT('Ctrl Pts',(2.73333333333332,14.0405108279174,-19.0497316231808));
#51969=CARTESIAN_POINT('Ctrl Pts',(3.36770544049384,14.0406593647044,-19.0496470247757));
#51970=CARTESIAN_POINT('Ctrl Pts',(4.12725475148089,14.0407035545206,-19.0496222505543));
#51971=CARTESIAN_POINT('Ctrl Pts',(4.39373035273626,14.0433198866416,-19.0477371998816));
#51972=CARTESIAN_POINT('Ctrl Pts',(4.90599112616755,14.0547497465385,-19.0395208824725));
#51973=CARTESIAN_POINT('Ctrl Pts',(5.78072777450692,14.0807920378816,-19.0208473878005));
#51974=CARTESIAN_POINT('Ctrl Pts',(6.47530496203834,14.0798518061703,-19.0216406137609));
#51975=CARTESIAN_POINT('Ctrl Pts',(6.96716149433085,14.0396024305645,-19.0501859265548));
#51976=CARTESIAN_POINT('Ctrl Pts',(7.09313355494184,14.029212756938,-19.0577571393445));
#51977=CARTESIAN_POINT('Ctrl Pts',(7.27501518208594,14.0130979804571,-19.0697412543813));
#51978=CARTESIAN_POINT('Ctrl Pts',(7.4588585143809,13.9956499602412,-19.0829112118382));
#51979=CARTESIAN_POINT('Ctrl Pts',(7.8232328589516,13.9581658333788,-19.111391624162));
#51980=CARTESIAN_POINT('Ctrl Pts',(8.36318149154488,13.8906875946527,-19.1628145686548));
#51981=CARTESIAN_POINT('Ctrl Pts',(8.93517301674487,13.7869110179481,-19.2380842355627));
#51982=CARTESIAN_POINT('Ctrl Pts',(9.36766944102217,13.6824940828447,-19.3100449969906));
#51983=CARTESIAN_POINT('Ctrl Pts',(9.57402188182549,13.6227011914904,-19.3499427790005));
#51984=CARTESIAN_POINT('Ctrl Pts',(10.1401453128135,13.4431272840522,-19.4677531472923));
#51985=CARTESIAN_POINT('Ctrl Pts',(11.0615860966997,13.0381462718132,-19.7484552766342));
#51986=CARTESIAN_POINT('Ctrl Pts',(11.9725168252953,12.4760551457986,-20.1114798309039));
#51987=CARTESIAN_POINT('Ctrl Pts',(12.6928298617397,11.9972242157899,-20.3879965049244));
#51988=CARTESIAN_POINT('Ctrl Pts',(13.1763132367642,11.6403697206645,-20.591319917764));
#51989=CARTESIAN_POINT('Ctrl Pts',(14.1425443268685,10.807707670116,-21.0504208046439));
#51990=CARTESIAN_POINT('Ctrl Pts',(14.8246630432476,10.1039973091049,-21.4016095272698));
#51991=CARTESIAN_POINT('Ctrl Pts',(15.4199295464537,9.46515875405639,-21.6773329562573));
#51992=CARTESIAN_POINT('Ctrl Pts',(15.6784405514184,9.17859896251508,-21.7979768782073));
#51993=CARTESIAN_POINT('Ctrl Pts',(16.1907883125052,8.57011255948466,-22.0441196100552));
#51994=CARTESIAN_POINT('Ctrl Pts',(17.0509810894248,7.45168253371926,-22.4641884940993));
#51995=CARTESIAN_POINT('Ctrl Pts',(17.7490528301793,6.41387004578994,-22.7837202098578));
#51996=CARTESIAN_POINT('Ctrl Pts',(18.4852578323668,5.28986633116544,-23.053856315933));
#51997=CARTESIAN_POINT('Ctrl Pts',(19.0038260606132,4.45316762536295,-23.2340669203721));
#51998=CARTESIAN_POINT('Ctrl Pts',(20.0035139458143,2.67878447452734,-23.52668999913));
#51999=CARTESIAN_POINT('Ctrl Pts',(20.7091427978092,1.29885794752446,-23.6391186363694));
#52000=CARTESIAN_POINT('Ctrl Pts',(22.403146683307,-2.02022054163564,-23.6710719995345));
#52001=CARTESIAN_POINT('Ctrl Pts',(23.5046677369882,-4.44224583503547,-23.3201179538783));
#52002=CARTESIAN_POINT('Ctrl Pts',(24.5020292171972,-6.94171785952187,-22.6001034215803));
#52003=CARTESIAN_POINT('Ctrl Pts',(2.09999999999998,20.1276734922909,-26.6827921732065));
#52004=CARTESIAN_POINT('Ctrl Pts',(2.73333333333332,20.1276734922909,-26.6827921732065));
#52005=CARTESIAN_POINT('Ctrl Pts',(3.36824035468517,20.1277999966281,-26.6827248844676));
#52006=CARTESIAN_POINT('Ctrl Pts',(4.12831946050022,20.1278353407483,-26.682706983803));
#52007=CARTESIAN_POINT('Ctrl Pts',(4.40147222634207,20.1315942338715,-26.6799317263204));
#52008=CARTESIAN_POINT('Ctrl Pts',(4.9180724847728,20.1477887080798,-26.6680072176987));
#52009=CARTESIAN_POINT('Ctrl Pts',(5.79140913132176,20.1841869107284,-26.6412944630435));
#52010=CARTESIAN_POINT('Ctrl Pts',(6.46267874194441,20.1818673038256,-26.6431805808982));
#52011=CARTESIAN_POINT('Ctrl Pts',(6.92901748474213,20.1289400767798,-26.6814764936299));
#52012=CARTESIAN_POINT('Ctrl Pts',(7.05467459429316,20.1144377758426,-26.692294551178));
#52013=CARTESIAN_POINT('Ctrl Pts',(7.23308118280245,20.0923833573486,-26.7090822928829));
#52014=CARTESIAN_POINT('Ctrl Pts',(7.41407148153067,20.0684217407377,-26.7276006746662));
#52015=CARTESIAN_POINT('Ctrl Pts',(7.77136342402986,20.0171916206279,-26.767467725355));
#52016=CARTESIAN_POINT('Ctrl Pts',(8.29881147671608,19.9253506286527,-26.8391763377014));
#52017=CARTESIAN_POINT('Ctrl Pts',(8.85382441430446,19.7854312459419,-26.9431420824863));
#52018=CARTESIAN_POINT('Ctrl Pts',(9.27345552895879,19.6450682120238,-27.0422453297518));
#52019=CARTESIAN_POINT('Ctrl Pts',(9.47428870911876,19.5645742402598,-27.0973020227195));
#52020=CARTESIAN_POINT('Ctrl Pts',(10.0274094887188,19.3220973290901,-27.2604732414786));
#52021=CARTESIAN_POINT('Ctrl Pts',(10.957336519856,18.7566911999351,-27.6644010649527));
#52022=CARTESIAN_POINT('Ctrl Pts',(11.8782898182081,17.9599375300719,-28.1936376395817));
#52023=CARTESIAN_POINT('Ctrl Pts',(12.6022503935223,17.2852478950138,-28.5944892337399));
#52024=CARTESIAN_POINT('Ctrl Pts',(13.0991012510153,16.7709190727932,-28.8970744032444));
#52025=CARTESIAN_POINT('Ctrl Pts',(14.0799616178224,15.5798854129963,-29.5722844768448));
#52026=CARTESIAN_POINT('Ctrl Pts',(14.7680852092718,14.579052621997,-30.0849315139416));
#52027=CARTESIAN_POINT('Ctrl Pts',(15.3645561107598,13.6781623100496,-30.4847911076143));
#52028=CARTESIAN_POINT('Ctrl Pts',(15.6279528535259,13.2647887968605,-30.6643324056741));
#52029=CARTESIAN_POINT('Ctrl Pts',(16.1459139527021,12.3946624979674,-31.0266453695517));
#52030=CARTESIAN_POINT('Ctrl Pts',(17.013910567048,10.7975178255105,-31.6438588656908));
#52031=CARTESIAN_POINT('Ctrl Pts',(17.7140149010249,9.32634196499537,-32.1100100091169));
#52032=CARTESIAN_POINT('Ctrl Pts',(18.4510929547942,7.73876056396156,-32.505613445104));
#52033=CARTESIAN_POINT('Ctrl Pts',(18.9739954119137,6.5405150412443,-32.774374473624));
#52034=CARTESIAN_POINT('Ctrl Pts',(19.9765231119574,4.02047707679407,-33.2090980004561));
#52035=CARTESIAN_POINT('Ctrl Pts',(20.6834924480325,2.06477337861421,-33.3821520755448));
#52036=CARTESIAN_POINT('Ctrl Pts',(22.3784539898323,-2.62828368271897,-33.4598843240797));
#52037=CARTESIAN_POINT('Ctrl Pts',(23.4839952293235,-6.08084055797285,-32.9845938002433));
#52038=CARTESIAN_POINT('Ctrl Pts',(24.4831092917558,-9.6347294289213,-31.9813971448826));
#52039=CARTESIAN_POINT('Ctrl Pts',(2.09999999999998,23.6060521576472,-31.0445410589354));
#52040=CARTESIAN_POINT('Ctrl Pts',(2.73333333333332,23.6060521576472,-31.0445410589354));
#52041=CARTESIAN_POINT('Ctrl Pts',(3.36856654542017,23.6061635860875,-31.0444839306223));
#52042=CARTESIAN_POINT('Ctrl Pts',(4.12895234149475,23.606193256038,-31.0444699032081));
#52043=CARTESIAN_POINT('Ctrl Pts',(4.40592848799383,23.6106268023555,-31.041168515519));
#52044=CARTESIAN_POINT('Ctrl Pts',(4.92497320633879,23.6295933396541,-31.0270850709477));
#52045=CARTESIAN_POINT('Ctrl Pts',(5.79761961985324,23.6718783150368,-30.9958030248401));
#52046=CARTESIAN_POINT('Ctrl Pts',(6.45533229527709,23.6686137447905,-30.998435202078));
#52047=CARTESIAN_POINT('Ctrl Pts',(6.90782015375558,23.6091196795821,-31.0417634176017));
#52048=CARTESIAN_POINT('Ctrl Pts',(7.03331040148622,23.5922768022307,-31.0544297184954));
#52049=CARTESIAN_POINT('Ctrl Pts',(7.20984968522255,23.5669255464429,-31.0738857861351));
#52050=CARTESIAN_POINT('Ctrl Pts',(7.3893310776903,23.5393269357799,-31.095393818285));
#52051=CARTESIAN_POINT('Ctrl Pts',(7.74291210335288,23.4804567813196,-31.1415999795215));
#52052=CARTESIAN_POINT('Ctrl Pts',(8.26407103775564,23.375101565528,-31.2245832648744));
#52053=CARTESIAN_POINT('Ctrl Pts',(8.8115830223524,23.2149449411146,-31.3446386044841));
#52054=CARTESIAN_POINT('Ctrl Pts',(9.22667581471618,23.0537694784089,-31.4594769231126));
#52055=CARTESIAN_POINT('Ctrl Pts',(9.42604477578941,22.9609496680068,-31.5235804262132));
#52056=CARTESIAN_POINT('Ctrl Pts',(9.97678856421979,22.6803689675826,-31.7143127377213));
#52057=CARTESIAN_POINT('Ctrl Pts',(10.9141162969295,22.0169016367236,-32.1932131535475));
#52058=CARTESIAN_POINT('Ctrl Pts',(11.8388701416734,21.084176748631,-32.8181792996892));
#52059=CARTESIAN_POINT('Ctrl Pts',(12.5646367114059,20.2966269440717,-33.2903357867815));
#52060=CARTESIAN_POINT('Ctrl Pts',(13.0665475226764,19.6905411085284,-33.6504100246034));
#52061=CARTESIAN_POINT('Ctrl Pts',(14.0522782066389,18.294866663048,-34.4482865325554));
#52062=CARTESIAN_POINT('Ctrl Pts',(14.7430221797613,17.1241308380047,-35.0527157552754));
#52063=CARTESIAN_POINT('Ctrl Pts',(15.3400953918683,16.0732499778056,-35.5231797794399));
#52064=CARTESIAN_POINT('Ctrl Pts',(15.6052823188849,15.5879425580852,-35.7359287758697));
#52065=CARTESIAN_POINT('Ctrl Pts',(16.1254560189452,14.569125220435,-36.1638827804151));
#52066=CARTESIAN_POINT('Ctrl Pts',(16.996829231524,12.699834206496,-36.8925871221106));
#52067=CARTESIAN_POINT('Ctrl Pts',(17.6980324177114,10.9811103327506,-37.4420145883602));
#52068=CARTESIAN_POINT('Ctrl Pts',(18.4354718827656,9.1283982665082,-37.9088830089142));
#52069=CARTESIAN_POINT('Ctrl Pts',(18.9606999869237,7.72463416692537,-38.2276352431276));
#52070=CARTESIAN_POINT('Ctrl Pts',(19.9652054243195,4.77933627887349,-38.7429228174106));
#52071=CARTESIAN_POINT('Ctrl Pts',(20.6728661623116,2.49477830019891,-38.9501574688157));
#52072=CARTESIAN_POINT('Ctrl Pts',(22.3680046594236,-2.98344825060076,-39.0530209806881));
#52073=CARTESIAN_POINT('Ctrl Pts',(23.4757593035169,-7.02359945440365,-38.5057313141264));
#52074=CARTESIAN_POINT('Ctrl Pts',(24.4767076204831,-11.1800381806575,-37.3402432932818));
#52075=CARTESIAN_POINT('',(3.2,22.7328514723457,-29.9495820327474));
#52076=CARTESIAN_POINT('Ctrl Pts',(3.2,22.7328514723457,-29.9495820327475));
#52077=CARTESIAN_POINT('Ctrl Pts',(3.45174020120132,22.248104974443,-29.3417291505565));
#52078=CARTESIAN_POINT('Ctrl Pts',(3.71840125348693,21.7576384332226,-28.7267035609156));
#52079=CARTESIAN_POINT('Ctrl Pts',(4.,21.2644490398942,-28.1082636227258));
#52080=CARTESIAN_POINT('Ctrl Pts',(4.62816482155513,20.1642870857335,-26.7287041672028));
#52081=CARTESIAN_POINT('Ctrl Pts',(5.32582969298372,19.112709122184,-25.3133815304913));
#52082=CARTESIAN_POINT('Ctrl Pts',(6.03866111506183,18.0956114522777,-24.0462604082467));
#52083=CARTESIAN_POINT('Ctrl Pts',(6.32798220275237,17.6827960305236,-23.5319664953119));
#52084=CARTESIAN_POINT('Ctrl Pts',(6.61604117795301,17.2794652714956,-23.0487162961897));
#52085=CARTESIAN_POINT('Ctrl Pts',(6.89476148100327,16.8874284567183,-22.6097510295672));
#52086=CARTESIAN_POINT('Ctrl Pts',(7.65522892342214,15.817785410966,-21.4120672226614));
#52087=CARTESIAN_POINT('Ctrl Pts',(8.35226708635794,14.9194503847516,-20.4715588563443));
#52088=CARTESIAN_POINT('Ctrl Pts',(8.78926323490749,14.355233051296,-19.9177206283292));
#52089=CARTESIAN_POINT('Ctrl Pts',(8.99031958628575,14.0956438562298,-19.662906727227));
#52090=CARTESIAN_POINT('Ctrl Pts',(9.18275523109629,13.8483915014505,-19.4286423508446));
#52091=CARTESIAN_POINT('Ctrl Pts',(9.37496047537633,13.6006174248028,-19.2038629336386));
#52092=CARTESIAN_POINT('Ctrl Pts',(9.48075234282032,13.4642398646018,-19.0801418853484));
#52093=CARTESIAN_POINT('Ctrl Pts',(9.58626091404298,13.327984642801,-18.9596114725911));
#52094=CARTESIAN_POINT('Ctrl Pts',(9.69257910363365,13.1899893895466,-18.8412172354227));
#52095=CARTESIAN_POINT('Ctrl Pts',(10.0319880484304,12.7494549572509,-18.4632568575979));
#52096=CARTESIAN_POINT('Ctrl Pts',(10.3788056761856,12.2902497006998,-18.1076143195385));
#52097=CARTESIAN_POINT('Ctrl Pts',(10.7756849101744,11.7648559982034,-17.731189557802));
#52098=CARTESIAN_POINT('Ctrl Pts',(10.8890930420524,11.6147248923208,-17.6236262857404));
#52099=CARTESIAN_POINT('Ctrl Pts',(11.0576203537643,11.3913842275629,-17.466093373954));
#52100=CARTESIAN_POINT('Ctrl Pts',(11.2725125506914,11.1084603654433,-17.2736114037459));
#52101=CARTESIAN_POINT('Ctrl Pts',(11.5968279603642,10.6814715330817,-16.9831175192989));
#52102=CARTESIAN_POINT('Ctrl Pts',(12.025567884929,10.1177168965354,-16.6161644397795));
#52103=CARTESIAN_POINT('Ctrl Pts',(12.532035905153,9.4869884079099,-16.2042316548138));
#52104=CARTESIAN_POINT('Ctrl Pts',(13.0988763173527,8.7810753350164,-15.7431953399735));
#52105=CARTESIAN_POINT('Ctrl Pts',(13.7495416906409,7.95432619929805,-15.2695479464202));
#52106=CARTESIAN_POINT('Ctrl Pts',(14.4398764931151,7.10916666494483,-14.8029953911254));
#52107=CARTESIAN_POINT('Ctrl Pts',(14.7901814026826,6.68029717554548,-14.5662470045378));
#52108=CARTESIAN_POINT('Ctrl Pts',(15.1459546144383,6.25591299863767,-14.3334813778935));
#52109=CARTESIAN_POINT('Ctrl Pts',(15.4570717747561,5.9001432106612,-14.1321338018072));
#52110=CARTESIAN_POINT('Ctrl Pts',(15.7998231427917,5.50819896235894,-13.9103133240047));
#52111=CARTESIAN_POINT('Ctrl Pts',(16.0676294537022,5.20198370959687,-13.7458456728629));
#52112=CARTESIAN_POINT('Ctrl Pts',(16.3615308038184,4.86844862366034,-13.5698041325856));
#52113=CARTESIAN_POINT('Ctrl Pts',(17.0296616067428,4.110217793206,-13.1696059858025));
#52114=CARTESIAN_POINT('Ctrl Pts',(17.7084691897444,3.34909561452446,-12.7911871969579));
#52115=CARTESIAN_POINT('Ctrl Pts',(18.4207032016838,2.62478996807377,-12.4048105193286));
#52116=CARTESIAN_POINT('Ctrl Pts',(18.8298642044523,2.20869410681929,-12.1828465774007));
#52117=CARTESIAN_POINT('Ctrl Pts',(19.2113759275114,1.81977531174774,-11.9848915561808));
#52118=CARTESIAN_POINT('Ctrl Pts',(19.5701113610614,1.45769348413641,-11.8009398056712));
#52119=CARTESIAN_POINT('Ctrl Pts',(20.1215476022647,0.901113276683472,-11.5181752600562));
#52120=CARTESIAN_POINT('Ctrl Pts',(20.6514912601111,0.363614694912416,-11.2519266478905));
#52121=CARTESIAN_POINT('Ctrl Pts',(21.3979544325339,-0.320646129817996,
-10.8732172390043));
#52122=CARTESIAN_POINT('Ctrl Pts',(21.8107631281271,-0.699055713757323,
-10.6637835484127));
#52123=CARTESIAN_POINT('Ctrl Pts',(22.3076315954084,-1.14579605062356,-10.4120946972692));
#52124=CARTESIAN_POINT('Ctrl Pts',(22.8472772293558,-1.62955662628835,-10.1269169192224));
#52125=CARTESIAN_POINT('Ctrl Pts',(23.3953136567549,-2.12083905484158,-9.83730499461342));
#52126=CARTESIAN_POINT('Ctrl Pts',(23.9608264582608,-2.62824069788209,-9.52568075404202));
#52127=CARTESIAN_POINT('Ctrl Pts',(24.5,-3.12544889498789,-9.19761041611355));
#52128=CARTESIAN_POINT('Ctrl Pts',(2.79761440945937,23.3193979595446,-30.6850251548975));
#52129=CARTESIAN_POINT('Ctrl Pts',(2.93206893024197,23.1240804350591,-30.4400833497039));
#52130=CARTESIAN_POINT('Ctrl Pts',(3.06672946893634,22.928527622209,-30.1948428266097));
#52131=CARTESIAN_POINT('Ctrl Pts',(3.20144293004172,22.7329275986254,-29.9495427664931));
#52132=CARTESIAN_POINT('Origin',(2.9,0.,0.));
#52133=CARTESIAN_POINT('Origin',(3.2,0.,0.));
#52134=CARTESIAN_POINT('Ctrl Pts',(2.1,-1.28155061440791,-9.65940339474764));
#52135=CARTESIAN_POINT('Ctrl Pts',(2.73333333333333,-1.28155061440791,-9.65940339474764));
#52136=CARTESIAN_POINT('Ctrl Pts',(3.36631731606888,-1.28160190790707,-9.65938099478861));
#52137=CARTESIAN_POINT('Ctrl Pts',(4.12417509565397,-1.28161736833688,-9.65937414787961));
#52138=CARTESIAN_POINT('Ctrl Pts',(4.36792464736457,-1.2804091068822,-9.6595464518039));
#52139=CARTESIAN_POINT('Ctrl Pts',(4.86515686825693,-1.27488660478215,-9.66034332028297));
#52140=CARTESIAN_POINT('Ctrl Pts',(5.74557748576906,-1.26184798249892,-9.66223911748733));
#52141=CARTESIAN_POINT('Ctrl Pts',(6.51835851955694,-1.26164230505555,-9.66227145200332));
#52142=CARTESIAN_POINT('Ctrl Pts',(7.10309338724208,-1.28515972010509,-9.658747726709));
#52143=CARTESIAN_POINT('Ctrl Pts',(7.23024869643521,-1.29045297976683,-9.65801464099689));
#52144=CARTESIAN_POINT('Ctrl Pts',(7.42492914335972,-1.29917956503778,-9.6568856789673));
#52145=CARTESIAN_POINT('Ctrl Pts',(7.61949923308775,-1.30862177632596,-9.65572731198123));
#52146=CARTESIAN_POINT('Ctrl Pts',(8.01074641232386,-1.32920013902525,-9.65326080679973));
#52147=CARTESIAN_POINT('Ctrl Pts',(8.60081577956197,-1.36699309999216,-9.64872946052249));
#52148=CARTESIAN_POINT('Ctrl Pts',(9.25152613287282,-1.42571070422604,-9.64034868889098));
#52149=CARTESIAN_POINT('Ctrl Pts',(9.76265059143103,-1.48569089122728,-9.63040536367191));
#52150=CARTESIAN_POINT('Ctrl Pts',(10.0141493386521,-1.52058012336349,-9.62412541731759));
#52151=CARTESIAN_POINT('Ctrl Pts',(10.7177310059152,-1.62700473913724,-9.60414949273162));
#52152=CARTESIAN_POINT('Ctrl Pts',(11.8208420069978,-1.8678059348864,-9.56287894547604));
#52153=CARTESIAN_POINT('Ctrl Pts',(12.8080068087818,-2.16229044149045,-9.50065093843371));
#52154=CARTESIAN_POINT('Ctrl Pts',(13.560404949554,-2.3920805659028,-9.44058642082993));
#52155=CARTESIAN_POINT('Ctrl Pts',(14.1415309352711,-2.58837046806001,-9.38738192823919));
#52156=CARTESIAN_POINT('Ctrl Pts',(15.2007195797304,-3.00388456952685,-9.26580533995201));
#52157=CARTESIAN_POINT('Ctrl Pts',(15.9284992208669,-3.33152214815673,-9.15357602363817));
#52158=CARTESIAN_POINT('Ctrl Pts',(16.6747671783401,-3.66443059394905,-9.01938328351392));
#52159=CARTESIAN_POINT('Ctrl Pts',(17.2497798582943,-3.93726930925875,-8.90311266260874));
#52160=CARTESIAN_POINT('Ctrl Pts',(18.2984578568314,-4.48329425942222,-8.64639146157842));
#52161=CARTESIAN_POINT('Ctrl Pts',(19.0236730578911,-4.89100422008468,-8.42123413259578));
#52162=CARTESIAN_POINT('Ctrl Pts',(19.7682055319328,-5.29723443513983,-8.16373299921013));
#52163=CARTESIAN_POINT('Ctrl Pts',(20.3331603255054,-5.61711561770474,-7.94814232298995));
#52164=CARTESIAN_POINT('Ctrl Pts',(21.3723035139214,-6.23437055880962,-7.48347305814291));
#52165=CARTESIAN_POINT('Ctrl Pts',(22.0962492277569,-6.67058221462383,-7.09344903901532));
#52166=CARTESIAN_POINT('Ctrl Pts',(23.230243247065,-7.3072573440811,-6.43796882578206));
#52167=CARTESIAN_POINT('Ctrl Pts',(23.8854423668127,-7.66333672971863,-6.00193696589197));
#52168=CARTESIAN_POINT('Ctrl Pts',(24.5000000001022,-7.98533675016187,-5.53162409663373));
#52169=CARTESIAN_POINT('Ctrl Pts',(2.1,-2.21255777005862,-13.7384122607767));
#52170=CARTESIAN_POINT('Ctrl Pts',(2.73333333333334,-2.21255777005862,-13.7384122607767));
#52171=CARTESIAN_POINT('Ctrl Pts',(3.36612146729749,-2.21261791852302,-13.7383900087247));
#52172=CARTESIAN_POINT('Ctrl Pts',(4.12376029167732,-2.21263571619322,-13.738383314838));
#52173=CARTESIAN_POINT('Ctrl Pts',(4.36465706155994,-2.21092930027329,-13.7386765514597));
#52174=CARTESIAN_POINT('Ctrl Pts',(4.85999961632898,-2.20309745300305,-13.740033035105));
#52175=CARTESIAN_POINT('Ctrl Pts',(5.74112770525578,-2.18454375550621,-13.7432623997142));
#52176=CARTESIAN_POINT('Ctrl Pts',(6.52368850139862,-2.18411163742531,-13.7433502946453));
#52177=CARTESIAN_POINT('Ctrl Pts',(7.12006273833317,-2.21802212159882,-13.7373260594817));
#52178=CARTESIAN_POINT('Ctrl Pts',(7.24736606576941,-2.22555725019054,-13.7360683688785));
#52179=CARTESIAN_POINT('Ctrl Pts',(7.44365067907975,-2.23803816094386,-13.7341021683655));
#52180=CARTESIAN_POINT('Ctrl Pts',(7.63956445145365,-2.25153194017601,-13.7320672730228));
#52181=CARTESIAN_POINT('Ctrl Pts',(8.03418103434733,-2.28097257160256,-13.7277103278323));
#52182=CARTESIAN_POINT('Ctrl Pts',(8.63051246970729,-2.33509483691623,-13.7197091635916));
#52183=CARTESIAN_POINT('Ctrl Pts',(9.29107501673555,-2.41942454694128,-13.7053013523184));
#52184=CARTESIAN_POINT('Ctrl Pts',(9.81206255454758,-2.50581650276758,-13.6885430133877));
#52185=CARTESIAN_POINT('Ctrl Pts',(10.0692361367767,-2.55617164041776,-13.6780601778355));
#52186=CARTESIAN_POINT('Ctrl Pts',(10.7900877092649,-2.7099459022409,-13.6448883888619));
#52187=CARTESIAN_POINT('Ctrl Pts',(11.9163843329042,-3.05720701099178,-13.5754688821817));
#52188=CARTESIAN_POINT('Ctrl Pts',(12.9133076943621,-3.47807008854133,-13.4740241097693));
#52189=CARTESIAN_POINT('Ctrl Pts',(13.6697202365407,-3.80490979930021,-13.378562011322));
#52190=CARTESIAN_POINT('Ctrl Pts',(14.2631414165878,-4.08738507427771,-13.2935308185664));
#52191=CARTESIAN_POINT('Ctrl Pts',(15.3329106576864,-4.68070912639053,-13.101240706448));
#52192=CARTESIAN_POINT('Ctrl Pts',(16.0654025907068,-5.14567124856755,-12.9267704504935));
#52193=CARTESIAN_POINT('Ctrl Pts',(16.8131118314614,-5.61574596327599,-12.7209271490644));
#52194=CARTESIAN_POINT('Ctrl Pts',(17.3939372393177,-6.00393438452058,-12.5422941481349));
#52195=CARTESIAN_POINT('Ctrl Pts',(18.4451742590423,-6.77513244775298,-12.1515155544068));
#52196=CARTESIAN_POINT('Ctrl Pts',(19.1720636185852,-7.34823939444788,-11.812629885177));
#52197=CARTESIAN_POINT('Ctrl Pts',(19.9174234244712,-7.91731656489557,-11.4273658819217));
#52198=CARTESIAN_POINT('Ctrl Pts',(20.4826637954952,-8.36590489807333,-11.1058515767196));
#52199=CARTESIAN_POINT('Ctrl Pts',(21.5194458983524,-9.22680492945096,-10.4167337199079));
#52200=CARTESIAN_POINT('Ctrl Pts',(22.243344548252,-9.83277155091188,-9.84187194559463));
#52201=CARTESIAN_POINT('Ctrl Pts',(23.3780871572094,-10.71385497485,-8.87822042993801));
#52202=CARTESIAN_POINT('Ctrl Pts',(24.0312127056184,-11.2033753376215,-8.24209808616164));
#52203=CARTESIAN_POINT('Ctrl Pts',(24.6419825553303,-11.6420191810575,-7.55950905276451));
#52204=CARTESIAN_POINT('Ctrl Pts',(2.1,-4.38490779991026,-23.2560996148446));
#52205=CARTESIAN_POINT('Ctrl Pts',(2.73333333333333,-4.38490779991026,-23.2560996148446));
#52206=CARTESIAN_POINT('Ctrl Pts',(3.36564008017942,-4.38508116042703,-23.2560287329169));
#52207=CARTESIAN_POINT('Ctrl Pts',(4.12276128472868,-4.38513262027402,-23.2560072996302));
#52208=CARTESIAN_POINT('Ctrl Pts',(4.35699735286594,-4.38230977740128,-23.2565699804445));
#52209=CARTESIAN_POINT('Ctrl Pts',(4.84793951429674,-4.36918210570372,-23.2592057903194));
#52210=CARTESIAN_POINT('Ctrl Pts',(5.73067499683022,-4.33776730212203,-23.2655376571851));
#52211=CARTESIAN_POINT('Ctrl Pts',(6.53611671636356,-4.33658160877012,-23.265767496589));
#52212=CARTESIAN_POINT('Ctrl Pts',(7.15937822818369,-4.39617994653139,-23.2535633235265));
#52213=CARTESIAN_POINT('Ctrl Pts',(7.28702172240692,-4.40896850912345,-23.2510752985911));
#52214=CARTESIAN_POINT('Ctrl Pts',(7.48700530829323,-4.43042311822182,-23.2471037568475));
#52215=CARTESIAN_POINT('Ctrl Pts',(7.68600700139787,-4.45357347133899,-23.2429730262749));
#52216=CARTESIAN_POINT('Ctrl Pts',(8.08835779392234,-4.50421621750767,-23.2340785398084));
#52217=CARTESIAN_POINT('Ctrl Pts',(8.69893195391736,-4.59770266101496,-23.2176455238328));
#52218=CARTESIAN_POINT('Ctrl Pts',(9.38143254163704,-4.74441292400085,-23.1884943501166));
#52219=CARTESIAN_POINT('Ctrl Pts',(9.92343839876597,-4.89580885444304,-23.1549384812191));
#52220=CARTESIAN_POINT('Ctrl Pts',(10.1921791819974,-4.98449489776192,-23.134037511346));
#52221=CARTESIAN_POINT('Ctrl Pts',(10.9469680088848,-5.25628971829095,-23.0679401690825));
#52222=CARTESIAN_POINT('Ctrl Pts',(12.107158260859,-5.8643925878101,-22.9287500587564));
#52223=CARTESIAN_POINT('Ctrl Pts',(13.1093288009718,-6.58246121751017,-22.7337196703867));
#52224=CARTESIAN_POINT('Ctrl Pts',(13.868363784104,-7.13699217373245,-22.5542454574039));
#52225=CARTESIAN_POINT('Ctrl Pts',(14.4658194679741,-7.62110550283362,-22.3938560929523));
#52226=CARTESIAN_POINT('Ctrl Pts',(15.5292195040136,-8.62103895016778,-22.038206914543));
#52227=CARTESIAN_POINT('Ctrl Pts',(16.2561491669276,-9.40122850868889,-21.7197205453348));
#52228=CARTESIAN_POINT('Ctrl Pts',(17.0018532435041,-10.1902220748077,-21.3462154347651));
#52229=CARTESIAN_POINT('Ctrl Pts',(17.5710203116058,-10.8351560227674,-21.0277573312478));
#52230=CARTESIAN_POINT('Ctrl Pts',(18.6068243381709,-12.1143416642866,-20.3346523661785));
#52231=CARTESIAN_POINT('Ctrl Pts',(19.3243654506886,-13.065403566866,-19.7366577355752));
#52232=CARTESIAN_POINT('Ctrl Pts',(20.066678302647,-14.0132094185406,-19.0554988265218));
#52233=CARTESIAN_POINT('Ctrl Pts',(20.6168033619827,-14.7468573051219,-18.5000859105222));
#52234=CARTESIAN_POINT('Ctrl Pts',(21.6393889693043,-16.1640493530773,-17.3047719379402));
#52235=CARTESIAN_POINT('Ctrl Pts',(22.355483248933,-17.162221968649,-16.3084425572014));
#52236=CARTESIAN_POINT('Ctrl Pts',(23.4867251715054,-18.6164016930582,-14.6329535278187));
#52237=CARTESIAN_POINT('Ctrl Pts',(24.1253025812515,-19.4078682665568,-13.5489185574));
#52238=CARTESIAN_POINT('Ctrl Pts',(24.7277223812015,-20.1180951211746,-12.3854414359051));
#52239=CARTESIAN_POINT('Ctrl Pts',(2.1,-6.55725782976191,-32.7737869689125));
#52240=CARTESIAN_POINT('Ctrl Pts',(2.73333333333334,-6.55725782976191,-32.7737869689125));
#52241=CARTESIAN_POINT('Ctrl Pts',(3.36510076549686,-6.55740130038319,-32.7737235429482));
#52242=CARTESIAN_POINT('Ctrl Pts',(4.12169087089434,-6.55744105729207,-32.7737050579337));
#52243=CARTESIAN_POINT('Ctrl Pts',(4.34924984699947,-6.55357866493385,-32.774521358146));
#52244=CARTESIAN_POINT('Ctrl Pts',(4.83585190383048,-6.53530567363434,-32.7784073324155));
#52245=CARTESIAN_POINT('Ctrl Pts',(5.71998614385741,-6.49093149495111,-32.7878690946995));
#52246=CARTESIAN_POINT('Ctrl Pts',(6.54872736208918,-6.48802766186921,-32.7884974133419));
#52247=CARTESIAN_POINT('Ctrl Pts',(7.19750250780191,-6.57627048209899,-32.7694462450512));
#52248=CARTESIAN_POINT('Ctrl Pts',(7.32546084490579,-6.59435371051836,-32.765717554002));
#52249=CARTESIAN_POINT('Ctrl Pts',(7.52891895171438,-6.62522183456192,-32.7596388835674));
#52250=CARTESIAN_POINT('Ctrl Pts',(7.73077307336616,-6.65842767110204,-32.7533193763253));
#52251=CARTESIAN_POINT('Ctrl Pts',(8.14020547050341,-6.73134435356068,-32.7396330973257));
#52252=CARTESIAN_POINT('Ctrl Pts',(8.76327382634538,-6.86633080121424,-32.714277000723));
#52253=CARTESIAN_POINT('Ctrl Pts',(9.46274681600517,-7.07963379346393,-32.6693403316508));
#52254=CARTESIAN_POINT('Ctrl Pts',(10.017614109892,-7.29999454273279,-32.617935281249));
#52255=CARTESIAN_POINT('Ctrl Pts',(10.2918722028545,-7.42879902723335,-32.586110997956));
#52256=CARTESIAN_POINT('Ctrl Pts',(11.0596479948439,-7.8223339461195,-32.4860007673529));
#52257=CARTESIAN_POINT('Ctrl Pts',(12.211331411252,-8.67991526033185,-32.2795014435999));
#52258=CARTESIAN_POINT('Ctrl Pts',(13.2034376761732,-9.67994219031867,-31.9958455494954));
#52259=CARTESIAN_POINT('Ctrl Pts',(13.9587869858217,-10.4565075782823,-31.7345428390373));
#52260=CARTESIAN_POINT('Ctrl Pts',(14.5428320694722,-11.1220898054817,-31.5063608409992));
#52261=CARTESIAN_POINT('Ctrl Pts',(15.5915904941101,-12.5049041760033,-30.9987636124804));
#52262=CARTESIAN_POINT('Ctrl Pts',(16.3123392972128,-13.5898788951704,-30.5438307640613));
#52263=CARTESIAN_POINT('Ctrl Pts',(17.0563791111118,-14.6955951922712,-30.0067575635175));
#52264=CARTESIAN_POINT('Ctrl Pts',(17.6163059289884,-15.5819349355565,-29.5590986201794));
#52265=CARTESIAN_POINT('Ctrl Pts',(18.6451985583325,-17.3599656796549,-28.5761389977681));
#52266=CARTESIAN_POINT('Ctrl Pts',(19.3594303438975,-18.6865488395582,-27.7271731514842));
#52267=CARTESIAN_POINT('Ctrl Pts',(20.1009222175396,-20.0151479025086,-26.7556821733498));
#52268=CARTESIAN_POINT('Ctrl Pts',(20.6466402308937,-21.030426465412,-25.9748073051926));
#52269=CARTESIAN_POINT('Ctrl Pts',(21.6664010977576,-23.0078930048959,-24.2829755073075));
#52270=CARTESIAN_POINT('Ctrl Pts',(22.3810504024336,-24.4030893583186,-22.8712638027695));
#52271=CARTESIAN_POINT('Ctrl Pts',(23.5117580694457,-26.4396142021185,-20.4918798317284));
#52272=CARTESIAN_POINT('Ctrl Pts',(24.1480627906507,-27.5389977546928,-18.9644924777646));
#52273=CARTESIAN_POINT('Ctrl Pts',(24.7493903499091,-28.5277151370773,-17.3227988978198));
#52274=CARTESIAN_POINT('Ctrl Pts',(2.1,-7.79860070396284,-38.2124654569512));
#52275=CARTESIAN_POINT('Ctrl Pts',(2.73333333333333,-7.79860070396284,-38.2124654569512));
#52276=CARTESIAN_POINT('Ctrl Pts',(3.36477451767734,-7.79872668178171,-38.2124076368945));
#52277=CARTESIAN_POINT('Ctrl Pts',(4.12105795390395,-7.79875982746218,-38.2123912207539));
#52278=CARTESIAN_POINT('Ctrl Pts',(4.34479378544621,-7.79433071314039,-38.2133462736395));
#52279=CARTESIAN_POINT('Ctrl Pts',(4.82895151376368,-7.77317986564745,-38.2179328211141));
#52280=CARTESIAN_POINT('Ctrl Pts',(5.71377591256104,-7.72136220442836,-38.2291918165454));
#52281=CARTESIAN_POINT('Ctrl Pts',(6.55607299317545,-7.71728578679096,-38.2300939740762));
#52282=CARTESIAN_POINT('Ctrl Pts',(7.21869808515308,-7.82274179205237,-38.2069365723915));
#52283=CARTESIAN_POINT('Ctrl Pts',(7.34682327184808,-7.84386203725498,-38.2024959214673));
#52284=CARTESIAN_POINT('Ctrl Pts',(7.55214855896988,-7.8802299041422,-38.1951848870786));
#52285=CARTESIAN_POINT('Ctrl Pts',(7.75551147978984,-7.91928693575672,-38.1875896312606));
#52286=CARTESIAN_POINT('Ctrl Pts',(8.16865455442754,-8.00519656802901,-38.1711016701523));
#52287=CARTESIAN_POINT('Ctrl Pts',(8.79801144190279,-8.16440073086343,-38.1405254358603));
#52288=CARTESIAN_POINT('Ctrl Pts',(9.50498474714468,-8.41625819933518,-38.0864351163565));
#52289=CARTESIAN_POINT('Ctrl Pts',(10.0643900034903,-8.67568279563254,-38.024902443149));
#52290=CARTESIAN_POINT('Ctrl Pts',(10.3401121837103,-8.82680225521101,-37.9869846363453));
#52291=CARTESIAN_POINT('Ctrl Pts',(11.1102644279334,-9.28727841432574,-37.868102320491));
#52292=CARTESIAN_POINT('Ctrl Pts',(12.2545468430399,-10.2798783318648,-37.6252922831318));
#52293=CARTESIAN_POINT('Ctrl Pts',(13.2428517544314,-11.4392785377615,-37.2919891637173));
#52294=CARTESIAN_POINT('Ctrl Pts',(13.9963939127891,-12.3419444861523,-36.9844996268006));
#52295=CARTESIAN_POINT('Ctrl Pts',(14.5753802005105,-13.1095340012662,-36.7184795152973));
#52296=CARTESIAN_POINT('Ctrl Pts',(15.6192625879179,-14.7118683070092,-36.1244593262902));
#52297=CARTESIAN_POINT('Ctrl Pts',(16.3374020123066,-15.9713792188489,-35.5919214093329));
#52298=CARTESIAN_POINT('Ctrl Pts',(17.0806356432168,-17.2581947700535,-34.9618903427716));
#52299=CARTESIAN_POINT('Ctrl Pts',(17.6370189134984,-18.2837979918633,-34.4401616107928));
#52300=CARTESIAN_POINT('Ctrl Pts',(18.6628099255013,-20.3488100760065,-33.291180187705));
#52301=CARTESIAN_POINT('Ctrl Pts',(19.3754696037404,-21.8905313156091,-32.2990136429051));
#52302=CARTESIAN_POINT('Ctrl Pts',(20.1166288096483,-23.4369295004069,-31.1620681816041));
#52303=CARTESIAN_POINT('Ctrl Pts',(20.6600107888588,-24.6143015822174,-30.2519047078682));
#52304=CARTESIAN_POINT('Ctrl Pts',(21.677799407356,-26.9129383770149,-28.276094543497));
#52305=CARTESIAN_POINT('Ctrl Pts',(22.3918093779893,-28.5354767163545,-26.6272808649087));
#52306=CARTESIAN_POINT('Ctrl Pts',(23.5225085832192,-30.905250682406,-23.8461862521349));
#52307=CARTESIAN_POINT('Ctrl Pts',(24.157514841919,-32.1813366627448,-22.0653831262647));
#52308=CARTESIAN_POINT('Ctrl Pts',(24.7577717974218,-33.3295007473295,-20.1503690732212));
#52309=CARTESIAN_POINT('',(24.5,-7.98533675018927,-5.53162409676021));
#52310=CARTESIAN_POINT('Ctrl Pts',(24.5,-7.98533675018927,-5.53162409676021));
#52311=CARTESIAN_POINT('Ctrl Pts',(23.8274939346105,-7.79179330153433,-6.14100658734753));
#52312=CARTESIAN_POINT('Ctrl Pts',(23.3366347313968,-7.64970961728591,-6.56481136530389));
#52313=CARTESIAN_POINT('Ctrl Pts',(22.5855494187791,-7.42734387677876,-7.22058552996049));
#52314=CARTESIAN_POINT('Ctrl Pts',(22.2454144274572,-7.32664377261339,-7.51755810558866));
#52315=CARTESIAN_POINT('Ctrl Pts',(21.8382660749244,-7.19700906555054,-7.88116210508794));
#52316=CARTESIAN_POINT('Ctrl Pts',(21.3802156956577,-7.04734131796725,-8.29760563162483));
#52317=CARTESIAN_POINT('Ctrl Pts',(20.7694693297003,-6.84778022801936,-8.85287505606244));
#52318=CARTESIAN_POINT('Ctrl Pts',(20.1629003035383,-6.64759826746033,-9.41330941265572));
#52319=CARTESIAN_POINT('Ctrl Pts',(19.5574857571565,-6.47402412338126,-9.98319848690682));
#52320=CARTESIAN_POINT('Ctrl Pts',(18.641852941883,-6.2115094825428,-10.8451023519009));
#52321=CARTESIAN_POINT('Ctrl Pts',(17.7734813325897,-5.92779326145821,-11.7477852370966));
#52322=CARTESIAN_POINT('Ctrl Pts',(16.9621253116777,-5.71558340812137,-12.6333016467232));
#52323=CARTESIAN_POINT('Ctrl Pts',(16.8133360673648,-5.67666763884139,-12.7956906769628));
#52324=CARTESIAN_POINT('Ctrl Pts',(16.6656205371618,-5.63959048888305,-12.9586217386495));
#52325=CARTESIAN_POINT('Ctrl Pts',(16.5183901926363,-5.60441931851976,-13.1227300282793));
#52326=CARTESIAN_POINT('Ctrl Pts',(15.726452288601,-5.41523696599741,-14.0054527804615));
#52327=CARTESIAN_POINT('Ctrl Pts',(14.9462259717426,-5.20042309417513,-14.9632129988162));
#52328=CARTESIAN_POINT('Ctrl Pts',(14.2963150412798,-5.06317274092078,-15.7944759718845));
#52329=CARTESIAN_POINT('Ctrl Pts',(13.9908350932728,-4.99866046883726,-16.1851974660009));
#52330=CARTESIAN_POINT('Ctrl Pts',(13.7077063566251,-4.94733703640913,-16.556124793982));
#52331=CARTESIAN_POINT('Ctrl Pts',(13.4460198946299,-4.90799662279406,-16.905002605579));
#52332=CARTESIAN_POINT('Ctrl Pts',(12.8373295399395,-4.81648967155765,-17.7165025863783));
#52333=CARTESIAN_POINT('Ctrl Pts',(12.3530827400008,-4.74153986672384,-18.4095331888858));
#52334=CARTESIAN_POINT('Ctrl Pts',(11.977027567753,-4.69720924336388,-18.958655074939));
#52335=CARTESIAN_POINT('Ctrl Pts',(11.655397242359,-4.65929440036105,-19.4283049133829));
#52336=CARTESIAN_POINT('Ctrl Pts',(11.368420561205,-4.63402086471352,-19.8589729704981));
#52337=CARTESIAN_POINT('Ctrl Pts',(11.0710856781053,-4.62105342435355,-20.3157155446813));
#52338=CARTESIAN_POINT('Ctrl Pts',(10.8141787015478,-4.60984913556699,-20.7103559332398));
#52339=CARTESIAN_POINT('Ctrl Pts',(10.5576802661741,-4.60874384919066,-21.1126900533831));
#52340=CARTESIAN_POINT('Ctrl Pts',(10.2957959918397,-4.62202135570263,-21.5329760085416));
#52341=CARTESIAN_POINT('Ctrl Pts',(9.71459276345479,-4.65148830124287,-22.4657221789779));
#52342=CARTESIAN_POINT('Ctrl Pts',(9.09527967376712,-4.74839217740081,-23.5049560069573));
#52343=CARTESIAN_POINT('Ctrl Pts',(8.43168033653304,-4.91177772174176,-24.7156496305248));
#52344=CARTESIAN_POINT('Ctrl Pts',(7.97964340480655,-5.02307424663008,-25.5403614711655));
#52345=CARTESIAN_POINT('Ctrl Pts',(7.52291961074554,-5.16302904003053,-26.4199423107392));
#52346=CARTESIAN_POINT('Ctrl Pts',(7.10363554125515,-5.30796452319851,-27.2733711087693));
#52347=CARTESIAN_POINT('Ctrl Pts',(6.56327799556932,-5.49475192502499,-28.3732380588341));
#52348=CARTESIAN_POINT('Ctrl Pts',(6.08559840026265,-5.72631856597084,-29.4106367559605));
#52349=CARTESIAN_POINT('Ctrl Pts',(5.61708670833696,-5.98368137431826,-30.4930591500792));
#52350=CARTESIAN_POINT('Ctrl Pts',(5.04102956506852,-6.30012104213272,-31.8239483528715));
#52351=CARTESIAN_POINT('Ctrl Pts',(4.50102820504748,-6.64971333190113,-33.1788609907931));
#52352=CARTESIAN_POINT('Ctrl Pts',(4.,-6.96288805731186,-34.5509691145741));
#52353=CARTESIAN_POINT('Ctrl Pts',(3.72183418896936,-7.13675950927916,-35.3127497193948));
#52354=CARTESIAN_POINT('Ctrl Pts',(3.45538353518157,-7.31144697863298,-36.0781055299851));
#52355=CARTESIAN_POINT('Ctrl Pts',(3.2,-7.48695481785668,-36.8470556158206));
#52356=CARTESIAN_POINT('',(24.5,-22.711314109499,-14.6012400644491));
#52357=CARTESIAN_POINT('Ctrl Pts',(24.5,-22.7113141094989,-14.6012400644491));
#52358=CARTESIAN_POINT('Ctrl Pts',(24.5,-21.6612444285481,-13.9441972658053));
#52359=CARTESIAN_POINT('Ctrl Pts',(24.5,-20.6284979425513,-13.2990592550798));
#52360=CARTESIAN_POINT('Ctrl Pts',(24.5,-16.3584140276965,-10.6372840649079));
#52361=CARTESIAN_POINT('Ctrl Pts',(24.5,-11.8204260321014,-7.81894043060838));
#52362=CARTESIAN_POINT('Ctrl Pts',(24.5,-7.98533675018928,-5.53162409676021));
#52363=CARTESIAN_POINT('',(10.2670750393577,-7.59968099677392,-33.2963779888109));
#52364=CARTESIAN_POINT('Ctrl Pts',(10.2670750393577,-7.59968099677392,-33.2963779888109));
#52365=CARTESIAN_POINT('Ctrl Pts',(11.2293198185888,-7.85751093220376,-32.3343749713692));
#52366=CARTESIAN_POINT('Ctrl Pts',(12.092802582344,-8.36505042380101,-31.4950825542866));
#52367=CARTESIAN_POINT('Ctrl Pts',(14.3080979519049,-9.99690083383536,-29.3617204319546));
#52368=CARTESIAN_POINT('Ctrl Pts',(14.8952017874601,-10.5394379824431,-28.8060939602778));
#52369=CARTESIAN_POINT('Ctrl Pts',(17.0803363586062,-12.930959939454,-26.4724118333468));
#52370=CARTESIAN_POINT('Ctrl Pts',(17.6922811489506,-13.6632420748191,-25.7681575791701));
#52371=CARTESIAN_POINT('Ctrl Pts',(19.0755427322033,-15.4528573288732,-24.0359413364337));
#52372=CARTESIAN_POINT('Ctrl Pts',(20.2687424742408,-17.037585857733,-22.4580909086129));
#52373=CARTESIAN_POINT('Ctrl Pts',(22.3267279388309,-19.9349590187757,-18.9782950332083));
#52374=CARTESIAN_POINT('Ctrl Pts',(23.4192562717209,-21.3897764892588,-16.9977385665951));
#52375=CARTESIAN_POINT('Ctrl Pts',(24.5,-22.7113141094989,-14.6012400644491));
#52376=CARTESIAN_POINT('Ctrl Pts',(6.,-7.72847464911698,-38.226570335278));
#52377=CARTESIAN_POINT('Ctrl Pts',(7.51604047332548,-7.25149509435605,-36.1223672378383));
#52378=CARTESIAN_POINT('Ctrl Pts',(9.08449301626627,-7.38041248529,-34.500587661922));
#52379=CARTESIAN_POINT('Ctrl Pts',(9.8624969752411,-7.50317632397629,-33.7027132752924));
#52380=CARTESIAN_POINT('Ctrl Pts',(10.0667253012217,-7.54599802424764,-33.4966773895357));
#52381=CARTESIAN_POINT('Ctrl Pts',(10.2670750393577,-7.59968099677392,-33.2963779888109));
#52382=CARTESIAN_POINT('Origin',(24.5,-1.89142793862867,-8.2868872535455));
#52383=CARTESIAN_POINT('',(24.5,-9.13966689904905,-3.29104195297002));
#52384=CARTESIAN_POINT('Ctrl Pts',(24.5,-9.13966689904905,-3.29104195297002));
#52385=CARTESIAN_POINT('Ctrl Pts',(24.5,-9.07110398184028,-3.48145041140664));
#52386=CARTESIAN_POINT('Ctrl Pts',(24.5,-8.99656198952293,-3.66979647783168));
#52387=CARTESIAN_POINT('Ctrl Pts',(24.5,-8.66176238807634,-4.44398568939236));
#52388=CARTESIAN_POINT('Ctrl Pts',(24.5,-8.34993106747065,-5.00530337254428));
#52389=CARTESIAN_POINT('Ctrl Pts',(24.5,-7.98533675018927,-5.53162409676021));
#52390=CARTESIAN_POINT('',(24.5,-25.1047038636482,-9.93749686382478));
#52391=CARTESIAN_POINT('Ctrl Pts',(24.5,-9.13966689904905,-3.29104195297002));
#52392=CARTESIAN_POINT('Ctrl Pts',(24.5,-13.0912453003007,-5.00666635927105));
#52393=CARTESIAN_POINT('Ctrl Pts',(24.5,-18.4037408367292,-7.20260295357725));
#52394=CARTESIAN_POINT('Ctrl Pts',(24.5,-25.1047038636482,-9.93749686382477));
#52395=CARTESIAN_POINT('Origin',(24.5,0.,0.));
#52396=CARTESIAN_POINT('Ctrl Pts',(24.5,-25.1047039675821,-9.93749660126077));
#52397=CARTESIAN_POINT('Ctrl Pts',(24.5,-19.8711159090285,-23.1589027732729));
#52398=CARTESIAN_POINT('Ctrl Pts',(24.5,-6.00806521682049,-26.3230536289092));
#52399=CARTESIAN_POINT('Ctrl Pts',(24.5,20.3149884120887,-32.3311188457297));
#52400=CARTESIAN_POINT('Ctrl Pts',(24.5,26.3230536289092,-6.00806521682049));
#52401=CARTESIAN_POINT('Ctrl Pts',(24.5,32.3311188457297,20.3149884120887));
#52402=CARTESIAN_POINT('Ctrl Pts',(24.5,6.00806521682049,26.3230536289092));
#52403=CARTESIAN_POINT('Ctrl Pts',(24.5,-20.3149884120887,32.3311188457297));
#52404=CARTESIAN_POINT('Ctrl Pts',(24.5,-26.3230536289092,6.00806521682049));
#52405=CARTESIAN_POINT('Ctrl Pts',(24.5,-28.1858992943483,-2.15359491570446));
#52406=CARTESIAN_POINT('Ctrl Pts',(24.5,-25.1047039675821,-9.93749660126077));
#52407=CARTESIAN_POINT('Ctrl Pts',(24.3078118955742,-25.1351889338974,-9.9495638317503));
#52408=CARTESIAN_POINT('Ctrl Pts',(24.3078118955742,-19.89524566176,-23.1870249280633));
#52409=CARTESIAN_POINT('Ctrl Pts',(24.3078118955742,-6.01536088802186,-26.3550180529563));
#52410=CARTESIAN_POINT('Ctrl Pts',(24.3078118955742,20.3396571649344,-32.3703789409781));
#52411=CARTESIAN_POINT('Ctrl Pts',(24.3078118955742,26.3550180529563,-6.01536088802186));
#52412=CARTESIAN_POINT('Ctrl Pts',(24.3078118955742,32.3703789409781,20.3396571649344));
#52413=CARTESIAN_POINT('Ctrl Pts',(24.3078118955742,6.01536088802186,26.3550180529563));
#52414=CARTESIAN_POINT('Ctrl Pts',(24.3078118955742,-20.3396571649344,32.3703789409781));
#52415=CARTESIAN_POINT('Ctrl Pts',(24.3078118955742,-26.3550180529563,6.01536088802186));
#52416=CARTESIAN_POINT('Ctrl Pts',(24.3078118955742,-28.22012579595,-2.15621005382945));
#52417=CARTESIAN_POINT('Ctrl Pts',(24.3078118955742,-25.1351889338974,-9.9495638317503));
#52418=CARTESIAN_POINT('Ctrl Pts',(23.9225830034177,-25.2000312537492,-9.97523114628931));
#52419=CARTESIAN_POINT('Ctrl Pts',(23.9225830034177,-19.9465702762725,-23.2468414860669));
#52420=CARTESIAN_POINT('Ctrl Pts',(23.9225830034177,-6.03087897128556,-26.4230072180579));
#52421=CARTESIAN_POINT('Ctrl Pts',(23.9225830034177,20.3921282467724,-32.4538861893435));
#52422=CARTESIAN_POINT('Ctrl Pts',(23.9225830034177,26.4230072180579,-6.03087897128556));
#52423=CARTESIAN_POINT('Ctrl Pts',(23.9225830034177,32.4538861893435,20.3921282467724));
#52424=CARTESIAN_POINT('Ctrl Pts',(23.9225830034177,6.03087897128556,26.4230072180579));
#52425=CARTESIAN_POINT('Ctrl Pts',(23.9225830034177,-20.3921282467724,32.4538861893435));
#52426=CARTESIAN_POINT('Ctrl Pts',(23.9225830034177,-26.4230072180579,6.03087897128556));
#52427=CARTESIAN_POINT('Ctrl Pts',(23.9225830034177,-28.2929264591131,-2.16177252094858));
#52428=CARTESIAN_POINT('Ctrl Pts',(23.9225830034177,-25.2000312537492,-9.97523114628931));
#52429=CARTESIAN_POINT('Ctrl Pts',(23.3421815947946,-25.3089118559866,-10.0183306632593));
#52430=CARTESIAN_POINT('Ctrl Pts',(23.3421815947946,-20.0327524941588,-23.3472830321759));
#52431=CARTESIAN_POINT('Ctrl Pts',(23.3421815947946,-6.05693630938179,-26.5371718756275));
#52432=CARTESIAN_POINT('Ctrl Pts',(23.3421815947946,20.4802355662457,-32.5941081850093));
#52433=CARTESIAN_POINT('Ctrl Pts',(23.3421815947946,26.5371718756275,-6.05693630938179));
#52434=CARTESIAN_POINT('Ctrl Pts',(23.3421815947946,32.5941081850093,20.4802355662457));
#52435=CARTESIAN_POINT('Ctrl Pts',(23.3421815947946,6.05693630938179,26.5371718756275));
#52436=CARTESIAN_POINT('Ctrl Pts',(23.3421815947946,-20.4802355662457,32.5941081850093));
#52437=CARTESIAN_POINT('Ctrl Pts',(23.3421815947946,-26.5371718756275,6.05693630938179));
#52438=CARTESIAN_POINT('Ctrl Pts',(23.3421815947946,-28.4151703897221,-2.17111279087171));
#52439=CARTESIAN_POINT('Ctrl Pts',(23.3421815947946,-25.3089118559866,-10.0183306632593));
#52440=CARTESIAN_POINT('Ctrl Pts',(22.5631762070947,-25.4774153713825,-10.0850314343064));
#52441=CARTESIAN_POINT('Ctrl Pts',(22.5631762070947,-20.1661280117444,-23.5027262724168));
#52442=CARTESIAN_POINT('Ctrl Pts',(22.5631762070947,-6.09726262078023,-26.7138529899778));
#52443=CARTESIAN_POINT('Ctrl Pts',(22.5631762070947,20.6165903691975,-32.811115610758));
#52444=CARTESIAN_POINT('Ctrl Pts',(22.5631762070947,26.7138529899778,-6.09726262078023));
#52445=CARTESIAN_POINT('Ctrl Pts',(22.5631762070947,32.811115610758,20.6165903691975));
#52446=CARTESIAN_POINT('Ctrl Pts',(22.5631762070947,6.09726262078023,26.7138529899778));
#52447=CARTESIAN_POINT('Ctrl Pts',(22.5631762070947,-20.6165903691975,32.811115610758));
#52448=CARTESIAN_POINT('Ctrl Pts',(22.5631762070947,-26.7138529899778,6.09726262078023));
#52449=CARTESIAN_POINT('Ctrl Pts',(22.5631762070947,-28.6043549792646,-2.18556778362938));
#52450=CARTESIAN_POINT('Ctrl Pts',(22.5631762070947,-25.4774153713825,-10.0850314343064));
#52451=CARTESIAN_POINT('Ctrl Pts',(21.5808622776984,-25.7276079592011,-10.1840681723743));
#52452=CARTESIAN_POINT('Ctrl Pts',(21.5808622776984,-20.3641628469109,-23.7335270746635));
#52453=CARTESIAN_POINT('Ctrl Pts',(21.5808622776984,-6.15713878527594,-26.9761876072355));
#52454=CARTESIAN_POINT('Ctrl Pts',(21.5808622776984,20.8190488219595,-33.1333263925114));
#52455=CARTESIAN_POINT('Ctrl Pts',(21.5808622776984,26.9761876072355,-6.15713878527594));
#52456=CARTESIAN_POINT('Ctrl Pts',(21.5808622776984,33.1333263925114,20.8190488219595));
#52457=CARTESIAN_POINT('Ctrl Pts',(21.5808622776984,6.15713878527594,26.9761876072355));
#52458=CARTESIAN_POINT('Ctrl Pts',(21.5808622776984,-20.8190488219595,33.1333263925114));
#52459=CARTESIAN_POINT('Ctrl Pts',(21.5808622776984,-26.9761876072355,6.15713878527594));
#52460=CARTESIAN_POINT('Ctrl Pts',(21.5808622776984,-28.8852546502407,-2.20703043404616));
#52461=CARTESIAN_POINT('Ctrl Pts',(21.5808622776984,-25.7276079592011,-10.1840681723743));
#52462=CARTESIAN_POINT('Ctrl Pts',(20.5902243197586,-26.0184347228058,-10.2991896244579));
#52463=CARTESIAN_POINT('Ctrl Pts',(20.5902243197586,-20.5943608343677,-24.0018126019847));
#52464=CARTESIAN_POINT('Ctrl Pts',(20.5902243197586,-6.22673953280079,-27.2811284065763));
#52465=CARTESIAN_POINT('Ctrl Pts',(20.5902243197586,21.0543888737755,-33.5078679393771));
#52466=CARTESIAN_POINT('Ctrl Pts',(20.5902243197586,27.2811284065763,-6.22673953280079));
#52467=CARTESIAN_POINT('Ctrl Pts',(20.5902243197586,33.5078679393771,21.0543888737755));
#52468=CARTESIAN_POINT('Ctrl Pts',(20.5902243197586,6.22673953280079,27.2811284065763));
#52469=CARTESIAN_POINT('Ctrl Pts',(20.5902243197586,-21.0543888737755,33.5078679393771));
#52470=CARTESIAN_POINT('Ctrl Pts',(20.5902243197586,-27.2811284065763,6.22673953280079));
#52471=CARTESIAN_POINT('Ctrl Pts',(20.5902243197586,-29.2117756831773,-2.23197886762493));
#52472=CARTESIAN_POINT('Ctrl Pts',(20.5902243197586,-26.0184347228058,-10.2991896244579));
#52473=CARTESIAN_POINT('Ctrl Pts',(19.591895069338,-26.3512694502151,-10.4309395935745));
#52474=CARTESIAN_POINT('Ctrl Pts',(19.591895069338,-20.8578093679748,-24.3088501636144));
#52475=CARTESIAN_POINT('Ctrl Pts',(19.591895069338,-6.30639363871179,-27.6301158469569));
#52476=CARTESIAN_POINT('Ctrl Pts',(19.591895069338,21.3237222082451,-33.9365094856687));
#52477=CARTESIAN_POINT('Ctrl Pts',(19.591895069338,27.6301158469569,-6.30639363871179));
#52478=CARTESIAN_POINT('Ctrl Pts',(19.591895069338,33.9365094856687,21.3237222082451));
#52479=CARTESIAN_POINT('Ctrl Pts',(19.591895069338,6.30639363871179,27.6301158469569));
#52480=CARTESIAN_POINT('Ctrl Pts',(19.591895069338,-21.3237222082451,33.9365094856687));
#52481=CARTESIAN_POINT('Ctrl Pts',(19.591895069338,-27.6301158469569,6.30639363871179));
#52482=CARTESIAN_POINT('Ctrl Pts',(19.591895069338,-29.5854604762956,-2.26053093410794));
#52483=CARTESIAN_POINT('Ctrl Pts',(19.591895069338,-26.3512694502151,-10.4309395935745));
#52484=CARTESIAN_POINT('Ctrl Pts',(18.5871162949016,-26.7276913580337,-10.5799432000069));
#52485=CARTESIAN_POINT('Ctrl Pts',(18.5871162949016,-21.1557584443957,-24.6560965751298));
#52486=CARTESIAN_POINT('Ctrl Pts',(18.5871162949016,-6.39647904159621,-28.0248057855197));
#52487=CARTESIAN_POINT('Ctrl Pts',(18.5871162949016,21.6283267439235,-34.4212848271159));
#52488=CARTESIAN_POINT('Ctrl Pts',(18.5871162949016,28.0248057855197,-6.39647904159621));
#52489=CARTESIAN_POINT('Ctrl Pts',(18.5871162949016,34.4212848271159,21.6283267439235));
#52490=CARTESIAN_POINT('Ctrl Pts',(18.5871162949016,6.39647904159621,28.0248057855197));
#52491=CARTESIAN_POINT('Ctrl Pts',(18.5871162949016,-21.6283267439235,34.4212848271159));
#52492=CARTESIAN_POINT('Ctrl Pts',(18.5871162949016,-28.0248057855197,6.39647904159621));
#52493=CARTESIAN_POINT('Ctrl Pts',(18.5871162949016,-30.0080820694305,-2.29282210582957));
#52494=CARTESIAN_POINT('Ctrl Pts',(18.5871162949016,-26.7276913580337,-10.5799432000069));
#52495=CARTESIAN_POINT('Ctrl Pts',(17.577868433379,-27.149299963076,-10.7468335997137));
#52496=CARTESIAN_POINT('Ctrl Pts',(17.577868433379,-21.4894741285104,-25.045027378901));
#52497=CARTESIAN_POINT('Ctrl Pts',(17.577868433379,-6.49737853829363,-28.4668753648014));
#52498=CARTESIAN_POINT('Ctrl Pts',(17.577868433379,21.9694968265077,-34.964253903095));
#52499=CARTESIAN_POINT('Ctrl Pts',(17.577868433379,28.4668753648014,-6.49737853829363));
#52500=CARTESIAN_POINT('Ctrl Pts',(17.577868433379,34.964253903095,21.9694968265077));
#52501=CARTESIAN_POINT('Ctrl Pts',(17.577868433379,6.49737853829363,28.4668753648014));
#52502=CARTESIAN_POINT('Ctrl Pts',(17.577868433379,-21.9694968265077,34.964253903095));
#52503=CARTESIAN_POINT('Ctrl Pts',(17.577868433379,-28.4668753648014,6.49737853829363));
#52504=CARTESIAN_POINT('Ctrl Pts',(17.577868433379,-30.4814362941487,-2.32898959656791));
#52505=CARTESIAN_POINT('Ctrl Pts',(17.577868433379,-27.149299963076,-10.7468335997137));
#52506=CARTESIAN_POINT('Ctrl Pts',(16.5668667015923,-27.617432585777,-10.9321401603104));
#52507=CARTESIAN_POINT('Ctrl Pts',(16.5668667015923,-21.8600149490077,-25.4768762430872));
#52508=CARTESIAN_POINT('Ctrl Pts',(16.5668667015923,-6.60941217672811,-28.9577268063763));
#52509=CARTESIAN_POINT('Ctrl Pts',(16.5668667015923,22.3483146296482,-35.5671389831044));
#52510=CARTESIAN_POINT('Ctrl Pts',(16.5668667015923,28.9577268063763,-6.60941217672811));
#52511=CARTESIAN_POINT('Ctrl Pts',(16.5668667015923,35.5671389831044,22.3483146296482));
#52512=CARTESIAN_POINT('Ctrl Pts',(16.5668667015923,6.60941217672811,28.9577268063763));
#52513=CARTESIAN_POINT('Ctrl Pts',(16.5668667015923,-22.3483146296482,35.5671389831044));
#52514=CARTESIAN_POINT('Ctrl Pts',(16.5668667015923,-28.9577268063763,6.60941217672811));
#52515=CARTESIAN_POINT('Ctrl Pts',(16.5668667015923,-31.007024605283,-2.36914812771116));
#52516=CARTESIAN_POINT('Ctrl Pts',(16.5668667015923,-27.617432585777,-10.9321401603104));
#52517=CARTESIAN_POINT('Ctrl Pts',(15.5576189940876,-28.1328325376183,-11.1361571157115));
#52518=CARTESIAN_POINT('Ctrl Pts',(15.5576189940876,-22.2679692589159,-25.952328867004));
#52519=CARTESIAN_POINT('Ctrl Pts',(15.5576189940876,-6.73275784642441,-29.4981394951766));
#52520=CARTESIAN_POINT('Ctrl Pts',(15.5576189940876,22.7653816487522,-36.230897341601));
#52521=CARTESIAN_POINT('Ctrl Pts',(15.5576189940876,29.4981394951766,-6.73275784642441));
#52522=CARTESIAN_POINT('Ctrl Pts',(15.5576189940876,36.230897341601,22.7653816487522));
#52523=CARTESIAN_POINT('Ctrl Pts',(15.5576189940876,6.73275784642441,29.4981394951766));
#52524=CARTESIAN_POINT('Ctrl Pts',(15.5576189940876,-22.7653816487522,36.230897341601));
#52525=CARTESIAN_POINT('Ctrl Pts',(15.5576189940876,-29.4981394951766,6.73275784642441));
#52526=CARTESIAN_POINT('Ctrl Pts',(15.5576189940876,-31.5856815437464,-2.41336146387609));
#52527=CARTESIAN_POINT('Ctrl Pts',(15.5576189940876,-28.1328325376183,-11.1361571157115));
#52528=CARTESIAN_POINT('Ctrl Pts',(14.5544447688713,-28.6953342065352,-11.3588189097037));
#52529=CARTESIAN_POINT('Ctrl Pts',(14.5544447688713,-22.7132059713864,-26.4712324747531));
#52530=CARTESIAN_POINT('Ctrl Pts',(14.5544447688713,-6.86737591305398,-30.0879397818628));
#52531=CARTESIAN_POINT('Ctrl Pts',(14.5544447688713,23.2205638688088,-36.9553156949167));
#52532=CARTESIAN_POINT('Ctrl Pts',(14.5544447688713,30.0879397818628,-6.86737591305398));
#52533=CARTESIAN_POINT('Ctrl Pts',(14.5544447688713,36.9553156949167,23.2205638688088));
#52534=CARTESIAN_POINT('Ctrl Pts',(14.5544447688713,6.86737591305398,30.0879397818628));
#52535=CARTESIAN_POINT('Ctrl Pts',(14.5544447688713,-23.2205638688088,36.9553156949167));
#52536=CARTESIAN_POINT('Ctrl Pts',(14.5544447688713,-30.0879397818628,6.86737591305398));
#52537=CARTESIAN_POINT('Ctrl Pts',(14.5544447688713,-32.2172211712787,-2.46161539811165));
#52538=CARTESIAN_POINT('Ctrl Pts',(14.5544447688713,-28.6953342065352,-11.3588189097037));
#52539=CARTESIAN_POINT('Ctrl Pts',(13.5625963827217,-29.303338426322,-11.599492525114));
#52540=CARTESIAN_POINT('Ctrl Pts',(13.5625963827217,-23.1944592990561,-27.0321118473983));
#52541=CARTESIAN_POINT('Ctrl Pts',(13.5625963827217,-7.01288366368501,-30.7254508915224));
#52542=CARTESIAN_POINT('Ctrl Pts',(13.5625963827217,23.7125672278374,-37.7383345552074));
#52543=CARTESIAN_POINT('Ctrl Pts',(13.5625963827217,30.7254508915224,-7.01288366368501));
#52544=CARTESIAN_POINT('Ctrl Pts',(13.5625963827217,37.7383345552074,23.7125672278374));
#52545=CARTESIAN_POINT('Ctrl Pts',(13.5625963827217,7.01288366368501,30.7254508915224));
#52546=CARTESIAN_POINT('Ctrl Pts',(13.5625963827217,-23.7125672278374,37.7383345552074));
#52547=CARTESIAN_POINT('Ctrl Pts',(13.5625963827217,-30.7254508915224,7.01288366368501));
#52548=CARTESIAN_POINT('Ctrl Pts',(13.5625963827217,-32.8998480499537,-2.51377274671653));
#52549=CARTESIAN_POINT('Ctrl Pts',(13.5625963827217,-29.303338426322,-11.599492525114));
#52550=CARTESIAN_POINT('Ctrl Pts',(12.5880795783847,-29.953804607069,-11.8569743687062));
#52551=CARTESIAN_POINT('Ctrl Pts',(12.5880795783847,-23.7093225250562,-27.6321620633528));
#52552=CARTESIAN_POINT('Ctrl Pts',(12.5880795783847,-7.16855342343643,-31.4074846721918));
#52553=CARTESIAN_POINT('Ctrl Pts',(12.5880795783847,24.2389312487553,-38.5760380956282));
#52554=CARTESIAN_POINT('Ctrl Pts',(12.5880795783847,31.4074846721918,-7.16855342343643));
#52555=CARTESIAN_POINT('Ctrl Pts',(12.5880795783847,38.5760380956282,24.2389312487553));
#52556=CARTESIAN_POINT('Ctrl Pts',(12.5880795783847,7.16855342343643,31.4074846721918));
#52557=CARTESIAN_POINT('Ctrl Pts',(12.5880795783847,-24.2389312487553,38.5760380956282));
#52558=CARTESIAN_POINT('Ctrl Pts',(12.5880795783847,-31.4074846721918,7.16855342343643));
#52559=CARTESIAN_POINT('Ctrl Pts',(12.5880795783847,-33.6301484067549,-2.56957267415257));
#52560=CARTESIAN_POINT('Ctrl Pts',(12.5880795783847,-29.953804607069,-11.8569743687062));
#52561=CARTESIAN_POINT('Ctrl Pts',(11.6370973936883,-30.6429141327405,-12.1297528718146));
#52562=CARTESIAN_POINT('Ctrl Pts',(11.6370973936883,-24.2547731018213,-28.2678604777126));
#52563=CARTESIAN_POINT('Ctrl Pts',(11.6370973936883,-7.33347131998335,-32.1300371876035));
#52564=CARTESIAN_POINT('Ctrl Pts',(11.6370973936883,24.7965658676201,-39.4635085075869));
#52565=CARTESIAN_POINT('Ctrl Pts',(11.6370973936883,32.1300371876035,-7.33347131998335));
#52566=CARTESIAN_POINT('Ctrl Pts',(11.6370973936883,39.4635085075869,24.7965658676201));
#52567=CARTESIAN_POINT('Ctrl Pts',(11.6370973936883,7.33347131998335,32.1300371876035));
#52568=CARTESIAN_POINT('Ctrl Pts',(11.6370973936883,-24.7965658676201,39.4635085075869));
#52569=CARTESIAN_POINT('Ctrl Pts',(11.6370973936883,-32.1300371876035,7.33347131998335));
#52570=CARTESIAN_POINT('Ctrl Pts',(11.6370973936883,-34.403834952449,-2.62868760228581));
#52571=CARTESIAN_POINT('Ctrl Pts',(11.6370973936883,-30.6429141327405,-12.1297528718146));
#52572=CARTESIAN_POINT('Ctrl Pts',(10.7155646400367,-31.3665139069702,-12.4161840644057));
#52573=CARTESIAN_POINT('Ctrl Pts',(10.7155646400367,-24.8275237307087,-28.9353758899551));
#52574=CARTESIAN_POINT('Ctrl Pts',(10.7155646400367,-7.50664343306871,-32.8887537885844));
#52575=CARTESIAN_POINT('Ctrl Pts',(10.7155646400367,25.3821103555157,-40.3953972216531));
#52576=CARTESIAN_POINT('Ctrl Pts',(10.7155646400367,32.8887537885844,-7.50664343306871));
#52577=CARTESIAN_POINT('Ctrl Pts',(10.7155646400367,40.3953972216531,25.3821103555157));
#52578=CARTESIAN_POINT('Ctrl Pts',(10.7155646400367,7.50664343306871,32.8887537885844));
#52579=CARTESIAN_POINT('Ctrl Pts',(10.7155646400367,-25.3821103555157,40.3953972216531));
#52580=CARTESIAN_POINT('Ctrl Pts',(10.7155646400367,-32.8887537885844,7.50664343306871));
#52581=CARTESIAN_POINT('Ctrl Pts',(10.7155646400367,-35.2162448654354,-2.6907612597485));
#52582=CARTESIAN_POINT('Ctrl Pts',(10.7155646400367,-31.3665139069702,-12.4161840644057));
#52583=CARTESIAN_POINT('Ctrl Pts',(9.82859575068344,-32.1205853335902,-12.7146772172754));
#52584=CARTESIAN_POINT('Ctrl Pts',(9.82859575068344,-25.424393573962,-29.6310011749912));
#52585=CARTESIAN_POINT('Ctrl Pts',(9.82859575068344,-7.68710803106293,-33.6794208535527));
#52586=CARTESIAN_POINT('Ctrl Pts',(9.82859575068344,25.9923128224897,-41.3665288846156));
#52587=CARTESIAN_POINT('Ctrl Pts',(9.82859575068344,33.6794208535527,-7.68710803106293));
#52588=CARTESIAN_POINT('Ctrl Pts',(9.82859575068344,41.3665288846156,25.9923128224897));
#52589=CARTESIAN_POINT('Ctrl Pts',(9.82859575068344,7.68710803106293,33.6794208535527));
#52590=CARTESIAN_POINT('Ctrl Pts',(9.82859575068344,-25.9923128224897,41.3665288846156));
#52591=CARTESIAN_POINT('Ctrl Pts',(9.82859575068344,-33.6794208535527,7.68710803106293));
#52592=CARTESIAN_POINT('Ctrl Pts',(9.82859575068344,-36.0628663320299,-2.75544891320754));
#52593=CARTESIAN_POINT('Ctrl Pts',(9.82859575068344,-32.1205853335902,-12.7146772172754));
#52594=CARTESIAN_POINT('Ctrl Pts',(8.97989469943246,-32.9016913885774,-13.0238718119093));
#52595=CARTESIAN_POINT('Ctrl Pts',(8.97989469943246,-26.0426621253832,-30.3515657037115));
#52596=CARTESIAN_POINT('Ctrl Pts',(8.97989469943246,-7.87404256435505,-34.4984345571934));
#52597=CARTESIAN_POINT('Ctrl Pts',(8.97989469943246,26.6243919928384,-42.3724771215485));
#52598=CARTESIAN_POINT('Ctrl Pts',(8.97989469943246,34.4984345571934,-7.87404256435505));
#52599=CARTESIAN_POINT('Ctrl Pts',(8.97989469943246,42.3724771215485,26.6243919928384));
#52600=CARTESIAN_POINT('Ctrl Pts',(8.97989469943246,7.87404256435505,34.4984345571934));
#52601=CARTESIAN_POINT('Ctrl Pts',(8.97989469943246,-26.6243919928384,42.3724771215485));
#52602=CARTESIAN_POINT('Ctrl Pts',(8.97989469943246,-34.4984345571934,7.87404256435505));
#52603=CARTESIAN_POINT('Ctrl Pts',(8.97989469943246,-36.9398404892439,-2.82245571921564));
#52604=CARTESIAN_POINT('Ctrl Pts',(8.97989469943246,-32.9016913885774,-13.0238718119093));
#52605=CARTESIAN_POINT('Ctrl Pts',(8.1713316609345,-33.707318001253,-13.3427726735042));
#52606=CARTESIAN_POINT('Ctrl Pts',(8.1713316609345,-26.6803394236516,-31.0947502646053));
#52607=CARTESIAN_POINT('Ctrl Pts',(8.1713316609345,-8.06684536480278,-35.3431588191374));
#52608=CARTESIAN_POINT('Ctrl Pts',(8.1713316609345,27.2763134543346,-43.4100041839401));
#52609=CARTESIAN_POINT('Ctrl Pts',(8.1713316609345,35.3431588191374,-8.06684536480278));
#52610=CARTESIAN_POINT('Ctrl Pts',(8.1713316609345,43.4100041839401,27.2763134543346));
#52611=CARTESIAN_POINT('Ctrl Pts',(8.1713316609345,8.06684536480278,35.3431588191374));
#52612=CARTESIAN_POINT('Ctrl Pts',(8.1713316609345,-27.2763134543346,43.4100041839401));
#52613=CARTESIAN_POINT('Ctrl Pts',(8.1713316609345,-35.3431588191374,8.06684536480278));
#52614=CARTESIAN_POINT('Ctrl Pts',(8.1713316609345,-37.8443447049894,-2.89156600943276));
#52615=CARTESIAN_POINT('Ctrl Pts',(8.1713316609345,-33.707318001253,-13.3427726735042));
#52616=CARTESIAN_POINT('Ctrl Pts',(7.40358438374929,-34.5357194373629,-13.6706887670958));
#52617=CARTESIAN_POINT('Ctrl Pts',(7.40358438374929,-27.3360436684578,-31.8589444308015));
#52618=CARTESIAN_POINT('Ctrl Pts',(7.40358438374929,-8.26509864276548,-36.2117631833691));
#52619=CARTESIAN_POINT('Ctrl Pts',(7.40358438374929,27.9466645406036,-44.4768618261345));
#52620=CARTESIAN_POINT('Ctrl Pts',(7.40358438374929,36.2117631833691,-8.26509864276548));
#52621=CARTESIAN_POINT('Ctrl Pts',(7.40358438374929,44.4768618261345,27.9466645406036));
#52622=CARTESIAN_POINT('Ctrl Pts',(7.40358438374929,8.26509864276548,36.2117631833691));
#52623=CARTESIAN_POINT('Ctrl Pts',(7.40358438374929,-27.9466645406036,44.4768618261345));
#52624=CARTESIAN_POINT('Ctrl Pts',(7.40358438374929,-36.2117631833691,8.26509864276548));
#52625=CARTESIAN_POINT('Ctrl Pts',(7.40358438374929,-38.7744189844407,-2.9626300268883));
#52626=CARTESIAN_POINT('Ctrl Pts',(7.40358438374929,-34.5357194373629,-13.6706887670958));
#52627=CARTESIAN_POINT('Ctrl Pts',(6.82198164612729,-35.215801161671,-13.9398936871227));
#52628=CARTESIAN_POINT('Ctrl Pts',(6.82198164612729,-27.8743484733577,-32.4863147655192));
#52629=CARTESIAN_POINT('Ctrl Pts',(6.82198164612729,-8.42785600320626,-36.9248497716085));
#52630=CARTESIAN_POINT('Ctrl Pts',(6.82198164612729,28.4969937684022,-45.3527057748147));
#52631=CARTESIAN_POINT('Ctrl Pts',(6.82198164612729,36.9248497716085,-8.42785600320626));
#52632=CARTESIAN_POINT('Ctrl Pts',(6.82198164612729,45.3527057748147,28.4969937684022));
#52633=CARTESIAN_POINT('Ctrl Pts',(6.82198164612729,8.42785600320626,36.9248497716085));
#52634=CARTESIAN_POINT('Ctrl Pts',(6.82198164612729,-28.4969937684022,45.3527057748147));
#52635=CARTESIAN_POINT('Ctrl Pts',(6.82198164612729,-36.9248497716085,8.42785600320626));
#52636=CARTESIAN_POINT('Ctrl Pts',(6.82198164612729,-39.5379697125444,-3.02097050943789));
#52637=CARTESIAN_POINT('Ctrl Pts',(6.82198164612729,-35.215801161671,-13.9398936871227));
#52638=CARTESIAN_POINT('Ctrl Pts',(6.40395249919757,-35.7353867802651,-14.1455675052848));
#52639=CARTESIAN_POINT('Ctrl Pts',(6.40395249919757,-28.285615862333,-32.9656286358978));
#52640=CARTESIAN_POINT('Ctrl Pts',(6.40395249919757,-8.55220338791416,-37.4696512606331));
#52641=CARTESIAN_POINT('Ctrl Pts',(6.40395249919757,28.9174478727189,-46.0218546485472));
#52642=CARTESIAN_POINT('Ctrl Pts',(6.40395249919757,37.4696512606331,-8.55220338791416));
#52643=CARTESIAN_POINT('Ctrl Pts',(6.40395249919757,46.0218546485472,28.9174478727189));
#52644=CARTESIAN_POINT('Ctrl Pts',(6.40395249919757,8.55220338791416,37.4696512606331));
#52645=CARTESIAN_POINT('Ctrl Pts',(6.40395249919757,-28.9174478727189,46.0218546485472));
#52646=CARTESIAN_POINT('Ctrl Pts',(6.40395249919757,-37.4696512606331,8.55220338791416));
#52647=CARTESIAN_POINT('Ctrl Pts',(6.40395249919757,-40.1213260404818,-3.06554291100543));
#52648=CARTESIAN_POINT('Ctrl Pts',(6.40395249919757,-35.7353867802651,-14.1455675052848));
#52649=CARTESIAN_POINT('Ctrl Pts',(6.13331019225912,-36.0859930662305,-14.2843522039477));
#52650=CARTESIAN_POINT('Ctrl Pts',(6.13331019225912,-28.563131110306,-33.2890603281757));
#52651=CARTESIAN_POINT('Ctrl Pts',(6.13331019225912,-8.63611058850205,-37.8372727263161));
#52652=CARTESIAN_POINT('Ctrl Pts',(6.13331019225912,29.201162137814,-46.4733833148181));
#52653=CARTESIAN_POINT('Ctrl Pts',(6.13331019225912,37.8372727263161,-8.63611058850205));
#52654=CARTESIAN_POINT('Ctrl Pts',(6.13331019225912,46.4733833148181,29.201162137814));
#52655=CARTESIAN_POINT('Ctrl Pts',(6.13331019225912,8.63611058850205,37.8372727263161));
#52656=CARTESIAN_POINT('Ctrl Pts',(6.13331019225912,-29.201162137814,46.4733833148181));
#52657=CARTESIAN_POINT('Ctrl Pts',(6.13331019225912,-37.8372727263161,8.63611058850205));
#52658=CARTESIAN_POINT('Ctrl Pts',(6.13331019225912,-40.5149635627942,-3.09561950206359));
#52659=CARTESIAN_POINT('Ctrl Pts',(6.13331019225912,-36.0859930662305,-14.2843522039477));
#52660=CARTESIAN_POINT('Ctrl Pts',(6.,-36.2623501753963,-14.3541617573767));
#52661=CARTESIAN_POINT('Ctrl Pts',(6.,-28.7027229797079,-33.4517484502831));
#52662=CARTESIAN_POINT('Ctrl Pts',(6.,-8.67831642429627,-38.0221885750911));
#52663=CARTESIAN_POINT('Ctrl Pts',(6.,29.3438721507948,-46.7005049993874));
#52664=CARTESIAN_POINT('Ctrl Pts',(6.,38.0221885750911,-8.67831642429627));
#52665=CARTESIAN_POINT('Ctrl Pts',(6.,46.7005049993874,29.3438721507948));
#52666=CARTESIAN_POINT('Ctrl Pts',(6.,8.67831642429627,38.0221885750911));
#52667=CARTESIAN_POINT('Ctrl Pts',(6.,-29.3438721507948,46.7005049993874));
#52668=CARTESIAN_POINT('Ctrl Pts',(6.,-38.0221885750911,8.67831642429627));
#52669=CARTESIAN_POINT('Ctrl Pts',(6.,-40.712965647392,-3.11074821157311));
#52670=CARTESIAN_POINT('Ctrl Pts',(6.,-36.2623501753963,-14.3541617573767));
#52671=CARTESIAN_POINT('Ctrl Pts',(24.5,-25.1047038636482,-9.93749686382478));
#52672=CARTESIAN_POINT('Ctrl Pts',(23.5178991898112,-24.1800618375919,-12.7285921692414));
#52673=CARTESIAN_POINT('Ctrl Pts',(22.3947886245986,-22.9066712578981,-15.3368782056101));
#52674=CARTESIAN_POINT('Ctrl Pts',(21.1743874927566,-21.4014661870157,-17.7488090012037));
#52675=CARTESIAN_POINT('Ctrl Pts',(20.5031871793432,-20.5736284466467,-19.0753308010405));
#52676=CARTESIAN_POINT('Ctrl Pts',(19.8411792966404,-19.6547951629279,-20.3436164685197));
#52677=CARTESIAN_POINT('Ctrl Pts',(19.1295827650255,-18.6997631766802,-21.5506695935102));
#52678=CARTESIAN_POINT('Ctrl Pts',(18.8261415870909,-18.292515504724,-22.0653848932679));
#52679=CARTESIAN_POINT('Ctrl Pts',(18.5104994276269,-17.8755457477642,-22.5733182213923));
#52680=CARTESIAN_POINT('Ctrl Pts',(18.2016639423759,-17.4841653683043,-23.0425019325362));
#52681=CARTESIAN_POINT('Ctrl Pts',(17.6747132403632,-16.8163723990388,-23.8430468756124));
#52682=CARTESIAN_POINT('Ctrl Pts',(17.2016343370993,-16.1924367304962,-24.5348117442123));
#52683=CARTESIAN_POINT('Ctrl Pts',(16.8729352926459,-15.7719583526041,-24.9977071274998));
#52684=CARTESIAN_POINT('Ctrl Pts',(16.6342454025477,-15.4666214813799,-25.3338457626079));
#52685=CARTESIAN_POINT('Ctrl Pts',(16.5014949770664,-15.3003859066593,-25.5143555186366));
#52686=CARTESIAN_POINT('Ctrl Pts',(16.3424569562979,-15.103934966335,-25.7283911089022));
#52687=CARTESIAN_POINT('Ctrl Pts',(15.993118510103,-14.6724163526426,-26.1985356703879));
#52688=CARTESIAN_POINT('Ctrl Pts',(15.6312480487537,-14.2444422357772,-26.6631523446855));
#52689=CARTESIAN_POINT('Ctrl Pts',(15.2503296894305,-13.8328224068278,-27.1265358149189));
#52690=CARTESIAN_POINT('Ctrl Pts',(14.7484414179076,-13.2904826654642,-27.737078003909));
#52691=CARTESIAN_POINT('Ctrl Pts',(14.2669345517206,-12.758775135315,-28.3184397273517));
#52692=CARTESIAN_POINT('Ctrl Pts',(13.7912435751455,-12.2785123659471,-28.871658502194));
#52693=CARTESIAN_POINT('Ctrl Pts',(13.5533980868579,-12.0383809812632,-29.1482678896151));
#52694=CARTESIAN_POINT('Ctrl Pts',(13.3161115657262,-11.8096746112359,-29.419343552208));
#52695=CARTESIAN_POINT('Ctrl Pts',(13.0766514227367,-11.5950868162136,-29.6877400273009));
#52696=CARTESIAN_POINT('Ctrl Pts',(12.9188702359555,-11.4536941128406,-29.8645874718875));
#52697=CARTESIAN_POINT('Ctrl Pts',(12.7601526360409,-11.3184278068389,-30.040278209103));
#52698=CARTESIAN_POINT('Ctrl Pts',(12.5997389313808,-11.1901315770832,-30.2157244086246));
#52699=CARTESIAN_POINT('Ctrl Pts',(12.5166971934814,-11.1237161675805,-30.3065480533187));
#52700=CARTESIAN_POINT('Ctrl Pts',(12.4397215765388,-11.06399531631,-30.3902672848899));
#52701=CARTESIAN_POINT('Ctrl Pts',(12.3478597934844,-10.9956710033332,-30.4895250762857));
#52702=CARTESIAN_POINT('Ctrl Pts',(11.9116121727781,-10.6712018064435,-30.960896019601));
#52703=CARTESIAN_POINT('Ctrl Pts',(10.7144663992385,-9.70825252947211,-32.2726748359188));
#52704=CARTESIAN_POINT('Ctrl Pts',(9.56604185022483,-9.37660667840678,-33.5284562887129));
#52705=CARTESIAN_POINT('Ctrl Pts',(9.07284645450859,-9.23418007589791,-34.0677565249154));
#52706=CARTESIAN_POINT('Ctrl Pts',(8.57333454992948,-9.18540482457354,-34.6139675361444));
#52707=CARTESIAN_POINT('Ctrl Pts',(8.00348148263344,-9.19403997702536,-35.280177286954));
#52708=CARTESIAN_POINT('Ctrl Pts',(7.6391942896614,-9.19956012884711,-35.7060619473711));
#52709=CARTESIAN_POINT('Ctrl Pts',(7.24388644384717,-9.23557279050204,-36.1897100386463));
#52710=CARTESIAN_POINT('Ctrl Pts',(6.94254646282512,-9.27355849403497,-36.5754634389434));
#52711=CARTESIAN_POINT('Ctrl Pts',(6.91433564865251,-9.27711463557301,-36.6115768595899));
#52712=CARTESIAN_POINT('Ctrl Pts',(6.88669635040545,-9.28069538863599,-36.6471093116181));
#52713=CARTESIAN_POINT('Ctrl Pts',(6.85962514029878,-9.28428605044135,-36.6820512136157));
#52714=CARTESIAN_POINT('Ctrl Pts',(6.4400006207374,-9.33994406236788,-37.2236774941018));
#52715=CARTESIAN_POINT('Ctrl Pts',(6.15412442492902,-9.43557095884828,-37.615340609517));
#52716=CARTESIAN_POINT('Ctrl Pts',(6.,-9.48407679455225,-37.8292517419395));
#52717=CARTESIAN_POINT('Ctrl Pts',(2.09999999999998,-3.03601716990075,-9.25709704779465));
#52718=CARTESIAN_POINT('Ctrl Pts',(2.73333333333332,-3.03601716990075,-9.25709704779465));
#52719=CARTESIAN_POINT('Ctrl Pts',(3.36700010948328,-3.03596462825959,-9.25711949436599));
#52720=CARTESIAN_POINT('Ctrl Pts',(4.12580403847648,-3.035948752271,-9.25712636633026));
#52721=CARTESIAN_POINT('Ctrl Pts',(4.38276376087194,-3.034724599393,-9.25754213874175));
#52722=CARTESIAN_POINT('Ctrl Pts',(4.88872719354341,-3.02930124281597,-9.25939165981087));
#52723=CARTESIAN_POINT('Ctrl Pts',(5.76577603006097,-3.01680014358279,-9.26367065608843));
#52724=CARTESIAN_POINT('Ctrl Pts',(6.49295950172122,-3.01700281594616,-9.2636387759413));
#52725=CARTESIAN_POINT('Ctrl Pts',(7.02336263943405,-3.03738330196137,-9.25654898425916));
#52726=CARTESIAN_POINT('Ctrl Pts',(7.14974440406645,-3.04241854797673,-9.25486655932582));
#52727=CARTESIAN_POINT('Ctrl Pts',(7.3995736148146,-3.05315049883967,-9.25139226428141));
#52728=CARTESIAN_POINT('Ctrl Pts',(7.71336783445791,-3.06825567663682,-9.24666612381336));
#52729=CARTESIAN_POINT('Ctrl Pts',(8.08762134632205,-3.08956528022687,-9.24001026491592));
#52730=CARTESIAN_POINT('Ctrl Pts',(8.58204140724159,-3.12288355797465,-9.22935038479259));
#52731=CARTESIAN_POINT('Ctrl Pts',(9.18586634302998,-3.17504806239954,-9.21173549473203));
#52732=CARTESIAN_POINT('Ctrl Pts',(9.64253482836406,-3.23031373876087,-9.19124308846978));
#52733=CARTESIAN_POINT('Ctrl Pts',(10.3691868352069,-3.33481918503072,-9.15051861370346));
#52734=CARTESIAN_POINT('Ctrl Pts',(11.1024062533893,-3.4863313251209,-9.09516757635316));
#52735=CARTESIAN_POINT('Ctrl Pts',(12.0425597052338,-3.73241232718711,-8.9976503328513));
#52736=CARTESIAN_POINT('Ctrl Pts',(12.4996009342521,-3.86235209382665,-8.9414277018268));
#52737=CARTESIAN_POINT('Ctrl Pts',(13.0011558990775,-4.00644645143633,-8.874918979412));
#52738=CARTESIAN_POINT('Ctrl Pts',(13.5006112777572,-4.1651105541745,-8.79993648213644));
#52739=CARTESIAN_POINT('Ctrl Pts',(14.4710715650308,-4.52003869162835,-8.62597550507522));
#52740=CARTESIAN_POINT('Ctrl Pts',(15.1518211493114,-4.80485184597868,-8.4717928050839));
#52741=CARTESIAN_POINT('Ctrl Pts',(15.8845703284776,-5.10582280931469,-8.28722797188002));
#52742=CARTESIAN_POINT('Ctrl Pts',(16.3869968088152,-5.32489776769872,-8.14702496307046));
#52743=CARTESIAN_POINT('Ctrl Pts',(17.3639569585992,-5.78783984375356,-7.83062294262033));
#52744=CARTESIAN_POINT('Ctrl Pts',(18.0500309778779,-6.13616822192816,-7.5603268394043));
#52745=CARTESIAN_POINT('Ctrl Pts',(18.7841811416569,-6.49299855871679,-7.24692816530861));
#52746=CARTESIAN_POINT('Ctrl Pts',(19.2877130443133,-6.74580743680106,-7.01244208981508));
#52747=CARTESIAN_POINT('Ctrl Pts',(20.2708116551819,-7.25764700376677,-6.49248945683397));
#52748=CARTESIAN_POINT('Ctrl Pts',(20.9685591537265,-7.61989877001792,-6.05996067164741));
#52749=CARTESIAN_POINT('Ctrl Pts',(22.6570098912121,-8.41829456543365,-4.95637665599812));
#52750=CARTESIAN_POINT('Ctrl Pts',(23.7241254823866,-8.86254721730646,-4.07948871958989));
#52751=CARTESIAN_POINT('Ctrl Pts',(24.6950729185821,-9.21040909328162,-3.09630974804701));
#52752=CARTESIAN_POINT('Ctrl Pts',(2.09999999999998,-3.65672665621579,-11.9766029963153));
#52753=CARTESIAN_POINT('Ctrl Pts',(2.73333333333332,-3.65672665621579,-11.9766029963153));
#52754=CARTESIAN_POINT('Ctrl Pts',(3.36712120601687,-3.65665584340833,-11.9766315438739));
#52755=CARTESIAN_POINT('Ctrl Pts',(4.12606819216906,-3.65663454744001,-11.9766402477875));
#52756=CARTESIAN_POINT('Ctrl Pts',(4.38492925999049,-3.65504218826977,-11.9771449683934));
#52757=CARTESIAN_POINT('Ctrl Pts',(4.89215030047201,-3.64800886033491,-11.9793835290183));
#52758=CARTESIAN_POINT('Ctrl Pts',(5.76872623835731,-3.63183832461054,-11.9845504064978));
#52759=CARTESIAN_POINT('Ctrl Pts',(6.48937126159138,-3.63217364414716,-11.9844905633463));
#52760=CARTESIAN_POINT('Ctrl Pts',(7.01201831810172,-3.65824051638801,-11.976019521284));
#52761=CARTESIAN_POINT('Ctrl Pts',(7.13827913651891,-3.66474966328796,-11.973992649138));
#52762=CARTESIAN_POINT('Ctrl Pts',(7.38675263276647,-3.67857740242105,-11.9698307262182));
#52763=CARTESIAN_POINT('Ctrl Pts',(7.69894445702103,-3.69804158026563,-11.9641827355297));
#52764=CARTESIAN_POINT('Ctrl Pts',(8.07058283408763,-3.72546787164587,-11.9562412019396));
#52765=CARTESIAN_POINT('Ctrl Pts',(8.5609042839681,-3.76830356997935,-11.9435176419542));
#52766=CARTESIAN_POINT('Ctrl Pts',(9.15816221625486,-3.83525991280854,-11.9224539215507));
#52767=CARTESIAN_POINT('Ctrl Pts',(9.60779259539962,-3.90596474603746,-11.8978913861869));
#52768=CARTESIAN_POINT('Ctrl Pts',(10.3209229382447,-4.0393084045542,-11.8490818060896));
#52769=CARTESIAN_POINT('Ctrl Pts',(11.0425587715381,-4.23303562018289,-11.7830103781896));
#52770=CARTESIAN_POINT('Ctrl Pts',(11.9743044133905,-4.5497935018951,-11.6653836085843));
#52771=CARTESIAN_POINT('Ctrl Pts',(12.4288874618463,-4.71763528480831,-11.5970273246365));
#52772=CARTESIAN_POINT('Ctrl Pts',(12.9286787374574,-4.90408555889076,-11.5157778410948));
#52773=CARTESIAN_POINT('Ctrl Pts',(13.4199974526641,-5.10750718068235,-11.4251100220548));
#52774=CARTESIAN_POINT('Ctrl Pts',(14.3833031177915,-5.5657285644765,-11.2131707854604));
#52775=CARTESIAN_POINT('Ctrl Pts',(15.0609019352795,-5.93504727306437,-11.0239005734077));
#52776=CARTESIAN_POINT('Ctrl Pts',(15.7927804449946,-6.32674632713181,-10.7954801539631));
#52777=CARTESIAN_POINT('Ctrl Pts',(16.2911437356496,-6.61047183230131,-10.6230415607221));
#52778=CARTESIAN_POINT('Ctrl Pts',(17.2659647556227,-7.21340018457687,-10.2311373480415));
#52779=CARTESIAN_POINT('Ctrl Pts',(17.9510657357558,-7.6687887141322,-9.89424383461141));
#52780=CARTESIAN_POINT('Ctrl Pts',(18.6848815503035,-8.13642726571135,-9.50186505396924));
#52781=CARTESIAN_POINT('Ctrl Pts',(19.1880112925449,-8.46802605481274,-9.20863204572925));
#52782=CARTESIAN_POINT('Ctrl Pts',(20.1723367890838,-9.14185982964497,-8.5552931434037));
#52783=CARTESIAN_POINT('Ctrl Pts',(20.8704681776515,-9.62058702907129,-8.00953397034699));
#52784=CARTESIAN_POINT('Ctrl Pts',(22.5588081046095,-10.6788873378614,-6.61393451767592));
#52785=CARTESIAN_POINT('Ctrl Pts',(23.6292145427077,-11.2779081469627,-5.49853642353553));
#52786=CARTESIAN_POINT('Ctrl Pts',(24.6070641578141,-11.7565436874769,-4.23746132912074));
#52787=CARTESIAN_POINT('Ctrl Pts',(2.09999999999998,-4.89814562884588,-17.4156148933567));
#52788=CARTESIAN_POINT('Ctrl Pts',(2.73333333333332,-4.89814562884588,-17.4156148933567));
#52789=CARTESIAN_POINT('Ctrl Pts',(3.36737232571569,-4.89802150608842,-17.4156658916616));
#52790=CARTESIAN_POINT('Ctrl Pts',(4.12660787609934,-4.89798436968063,-17.4156813973428));
#52791=CARTESIAN_POINT('Ctrl Pts',(4.38927320923596,-4.89563957363679,-17.4163681981935));
#52792=CARTESIAN_POINT('Ctrl Pts',(4.89900603841974,-4.88535460251535,-17.4193932655343));
#52793=CARTESIAN_POINT('Ctrl Pts',(5.77465260126722,-4.86184729038438,-17.4263372104577));
#52794=CARTESIAN_POINT('Ctrl Pts',(6.48219688444387,-4.8625594972863,-17.4262048870286));
#52795=CARTESIAN_POINT('Ctrl Pts',(6.98943485738849,-4.89946344728588,-17.4150979412944));
#52796=CARTESIAN_POINT('Ctrl Pts',(7.11545613477531,-4.90891054226745,-17.4123848398668));
#52797=CARTESIAN_POINT('Ctrl Pts',(7.36123936390851,-4.92882868688397,-17.4068717375096));
#52798=CARTESIAN_POINT('Ctrl Pts',(7.6702627990277,-4.95686731223262,-17.3994166487763));
#52799=CARTESIAN_POINT('Ctrl Pts',(8.0367413968953,-4.99627118676861,-17.388965573053));
#52800=CARTESIAN_POINT('Ctrl Pts',(8.51903353084918,-5.05765076313434,-17.3722391830899));
#52801=CARTESIAN_POINT('Ctrl Pts',(9.10355742307647,-5.15323263978595,-17.3445211388576));
#52802=CARTESIAN_POINT('Ctrl Pts',(9.53998094727572,-5.2533971526662,-17.3122002900072));
#52803=CARTESIAN_POINT('Ctrl Pts',(10.2287061596417,-5.44121042790069,-17.248118841033));
#52804=CARTESIAN_POINT('Ctrl Pts',(10.9322684728187,-5.71569213117839,-17.161803418548));
#52805=CARTESIAN_POINT('Ctrl Pts',(11.853432502986,-6.17162681919986,-17.0050023819074));
#52806=CARTESIAN_POINT('Ctrl Pts',(12.3052534899461,-6.41468310776573,-16.9128099061716));
#52807=CARTESIAN_POINT('Ctrl Pts',(12.8031221556086,-6.68546702830436,-16.8024678490713));
#52808=CARTESIAN_POINT('Ctrl Pts',(13.2871761296055,-6.97708915103167,-16.6812571176895));
#52809=CARTESIAN_POINT('Ctrl Pts',(14.2486052139259,-7.64348346076381,-16.3934928083832));
#52810=CARTESIAN_POINT('Ctrl Pts',(14.9265811207677,-8.1832906380615,-16.1339663223503));
#52811=CARTESIAN_POINT('Ctrl Pts',(15.6586876395449,-8.75682074682074,-15.8182194362082));
#52812=CARTESIAN_POINT('Ctrl Pts',(16.1598454115811,-9.17372704265915,-15.5797361779835));
#52813=CARTESIAN_POINT('Ctrl Pts',(17.1407792334809,-10.0631541608939,-15.0333575221981));
#52814=CARTESIAN_POINT('Ctrl Pts',(17.8296148723165,-10.7357158426118,-14.5611645715286));
#52815=CARTESIAN_POINT('Ctrl Pts',(18.5645831613832,-11.4254945580397,-14.0102872287392));
#52816=CARTESIAN_POINT('Ctrl Pts',(19.0747832425015,-11.9208360855031,-13.594485353105));
#52817=CARTESIAN_POINT('Ctrl Pts',(20.0668692671653,-12.924375055063,-12.6673387976086));
#52818=CARTESIAN_POINT('Ctrl Pts',(20.7688147271569,-13.6377206973786,-11.8912879181046));
#52819=CARTESIAN_POINT('Ctrl Pts',(22.460121536001,-15.2149112429765,-9.90766328280056));
#52820=CARTESIAN_POINT('Ctrl Pts',(23.5475247071985,-16.1319458054889,-8.29734249637728));
#52821=CARTESIAN_POINT('Ctrl Pts',(24.5367270315052,-16.8702662262976,-6.46720007277371));
#52822=CARTESIAN_POINT('Ctrl Pts',(2.09999999999998,-7.07062883094854,-26.9338857131792));
#52823=CARTESIAN_POINT('Ctrl Pts',(2.73333333333332,-7.07062883094854,-26.9338857131792));
#52824=CARTESIAN_POINT('Ctrl Pts',(3.36789866008651,-7.07046463114355,-26.933951186598));
#52825=CARTESIAN_POINT('Ctrl Pts',(4.12766416179872,-7.07041695394235,-26.9339707016016));
#52826=CARTESIAN_POINT('Ctrl Pts',(4.39699933335947,-7.0667088058488,-26.934985849138));
#52827=CARTESIAN_POINT('Ctrl Pts',(4.91111167246882,-7.05064293531159,-26.9394051279664));
#52828=CARTESIAN_POINT('Ctrl Pts',(5.78524431219031,-7.01434026039855,-26.9494462503479));
#52829=CARTESIAN_POINT('Ctrl Pts',(6.46975410539064,-7.01623847673174,-26.9490470248394));
#52830=CARTESIAN_POINT('Ctrl Pts',(6.95069999511141,-7.07036165458142,-26.93372166352));
#52831=CARTESIAN_POINT('Ctrl Pts',(7.0763178603825,-7.08492048653749,-26.9298148743264));
#52832=CARTESIAN_POINT('Ctrl Pts',(7.31752917791793,-7.11516421888208,-26.9220146572799));
#52833=CARTESIAN_POINT('Ctrl Pts',(7.62124943258259,-7.15777761960928,-26.9114950065043));
#52834=CARTESIAN_POINT('Ctrl Pts',(7.97914075673115,-7.21732108737006,-26.8968488632838));
#52835=CARTESIAN_POINT('Ctrl Pts',(8.44843546348636,-7.30970068233947,-26.8734648474066));
#52836=CARTESIAN_POINT('Ctrl Pts',(9.01308885010149,-7.45261747655674,-26.834787200002));
#52837=CARTESIAN_POINT('Ctrl Pts',(9.43131294671769,-7.60102319336957,-26.7897594463226));
#52838=CARTESIAN_POINT('Ctrl Pts',(10.0907596971815,-7.87860422770284,-26.7004946164726));
#52839=CARTESIAN_POINT('Ctrl Pts',(10.783467320144,-8.29417685100599,-26.5791525451474));
#52840=CARTESIAN_POINT('Ctrl Pts',(11.7034138999861,-8.99870155634605,-26.3527123769869));
#52841=CARTESIAN_POINT('Ctrl Pts',(12.1558320275245,-9.37558967844092,-26.2182079026623));
#52842=CARTESIAN_POINT('Ctrl Pts',(12.6542336070705,-9.7957041418195,-26.0565093323377));
#52843=CARTESIAN_POINT('Ctrl Pts',(13.1437514887892,-10.2520206694373,-25.8782496367525));
#52844=CARTESIAN_POINT('Ctrl Pts',(14.1171197855423,-11.298685793984,-25.4510876928653));
#52845=CARTESIAN_POINT('Ctrl Pts',(14.801673515149,-12.1453574316379,-25.0635325427391));
#52846=CARTESIAN_POINT('Ctrl Pts',(15.5357864365759,-13.0393873617087,-24.5925527412693));
#52847=CARTESIAN_POINT('Ctrl Pts',(16.048368284242,-13.7028332567132,-24.2302701739799));
#52848=CARTESIAN_POINT('Ctrl Pts',(17.0412321177376,-15.1050304906995,-23.4030485209266));
#52849=CARTESIAN_POINT('Ctrl Pts',(17.7361726306612,-16.1624249607158,-22.6867927333657));
#52850=CARTESIAN_POINT('Ctrl Pts',(18.4727161996985,-17.2407120307395,-21.854310708133));
#52851=CARTESIAN_POINT('Ctrl Pts',(18.992653507987,-18.0297266688986,-21.2147361058502));
#52852=CARTESIAN_POINT('Ctrl Pts',(19.993201743462,-19.6118718391751,-19.7977134333265));
#52853=CARTESIAN_POINT('Ctrl Pts',(20.6988514049915,-20.7341708993179,-18.6120452244264));
#52854=CARTESIAN_POINT('Ctrl Pts',(22.392495758694,-23.2107201272583,-15.588579749096));
#52855=CARTESIAN_POINT('Ctrl Pts',(23.493455201073,-24.679434474049,-13.0976556158903));
#52856=CARTESIAN_POINT('Ctrl Pts',(24.4910959878399,-25.8615426952525,-10.2656936020237));
#52857=CARTESIAN_POINT('Ctrl Pts',(2.09999999999998,-8.62240254673614,-33.7326505844809));
#52858=CARTESIAN_POINT('Ctrl Pts',(2.73333333333332,-8.62240254673614,-33.7326505844809));
#52859=CARTESIAN_POINT('Ctrl Pts',(3.36827652301208,-8.62225231332109,-33.7327142066686));
#52860=CARTESIAN_POINT('Ctrl Pts',(4.12841844272612,-8.62221062515808,-33.7327327108703));
#52861=CARTESIAN_POINT('Ctrl Pts',(4.40252493993054,-8.61748756225129,-33.7339916386456));
#52862=CARTESIAN_POINT('Ctrl Pts',(4.91972290753806,-8.59720819332077,-33.7394252545322));
#52863=CARTESIAN_POINT('Ctrl Pts',(5.79289024162273,-8.55181496845626,-33.7516673236045));
#52864=CARTESIAN_POINT('Ctrl Pts',(6.46065121315474,-8.55498795191946,-33.7509749771614));
#52865=CARTESIAN_POINT('Ctrl Pts',(6.92361646112076,-8.61993893328495,-33.7329735018433));
#52866=CARTESIAN_POINT('Ctrl Pts',(7.04896306476174,-8.63812452107151,-33.7282202863535));
#52867=CARTESIAN_POINT('Ctrl Pts',(7.28707567322587,-8.6754667244593,-33.7188513918404));
#52868=CARTESIAN_POINT('Ctrl Pts',(7.58726936452363,-8.72814137561322,-33.7062253222916));
#52869=CARTESIAN_POINT('Ctrl Pts',(7.93957047450264,-8.80142249811336,-33.6887386990264));
#52870=CARTESIAN_POINT('Ctrl Pts',(8.4007825112503,-8.91487937592376,-33.6608602352034));
#52871=CARTESIAN_POINT('Ctrl Pts',(8.95401946717244,-9.0897746461696,-33.6148182100539));
#52872=CARTESIAN_POINT('Ctrl Pts',(9.36430401987977,-9.27132051394991,-33.5610861019821));
#52873=CARTESIAN_POINT('Ctrl Pts',(10.0148540524883,-9.61284682840088,-33.4539650268594));
#52874=CARTESIAN_POINT('Ctrl Pts',(10.7127161292919,-10.1356319642981,-33.3060111863704));
#52875=CARTESIAN_POINT('Ctrl Pts',(11.6387106704067,-11.0248489283853,-33.027535101029));
#52876=CARTESIAN_POINT('Ctrl Pts',(12.0933528256764,-11.499599242688,-32.8619317339318));
#52877=CARTESIAN_POINT('Ctrl Pts',(12.5933109512149,-12.0280110081881,-32.6628317330708));
#52878=CARTESIAN_POINT('Ctrl Pts',(13.0908899144144,-12.6103513701059,-32.4405637422004));
#52879=CARTESIAN_POINT('Ctrl Pts',(14.0727400062371,-13.9365257971833,-31.9095619676101));
#52880=CARTESIAN_POINT('Ctrl Pts',(14.7612410141007,-15.0052037777513,-31.428066405722));
#52881=CARTESIAN_POINT('Ctrl Pts',(15.4964903549183,-16.1284628018935,-30.8447244672));
#52882=CARTESIAN_POINT('Ctrl Pts',(16.0148660701553,-16.9719590519182,-30.3908356683825));
#52883=CARTESIAN_POINT('Ctrl Pts',(17.0124971364499,-18.7417950627702,-29.3593075139289));
#52884=CARTESIAN_POINT('Ctrl Pts',(17.7100001824936,-20.0739603594528,-28.46645334904));
#52885=CARTESIAN_POINT('Ctrl Pts',(18.4472556019989,-21.4286595752151,-27.4310110272601));
#52886=CARTESIAN_POINT('Ctrl Pts',(18.970741165076,-22.4274147758341,-26.6295389239519));
#52887=CARTESIAN_POINT('Ctrl Pts',(19.9740132395736,-24.4205958470129,-24.8598580553113));
#52888=CARTESIAN_POINT('Ctrl Pts',(20.6810428764808,-25.8331306408346,-23.3798043172822));
#52889=CARTESIAN_POINT('Ctrl Pts',(22.3757637844863,-28.9472763223035,-19.6095668360326));
#52890=CARTESIAN_POINT('Ctrl Pts',(23.4815899075194,-30.8056241230732,-16.4879028202221));
#52891=CARTESIAN_POINT('Ctrl Pts',(24.4815088739376,-32.299518402771,-12.9405938991905));
#52892=CARTESIAN_POINT('Ctrl Pts',(2.09999999999998,-9.55346677620871,-37.8119095072619));
#52893=CARTESIAN_POINT('Ctrl Pts',(2.73333333333332,-9.55346677620871,-37.8119095072619));
#52894=CARTESIAN_POINT('Ctrl Pts',(3.36850564609381,-9.55333227030529,-37.8119692060198));
#52895=CARTESIAN_POINT('Ctrl Pts',(4.12887280195021,-9.55329634226044,-37.8119862483609));
#52896=CARTESIAN_POINT('Ctrl Pts',(4.40584576278457,-9.54794955963462,-37.8133947479414));
#52897=CARTESIAN_POINT('Ctrl Pts',(4.92487357234802,-9.5251083652532,-37.8194443413709));
#52898=CARTESIAN_POINT('Ctrl Pts',(5.79752076681712,-9.47428442849641,-37.833001467378));
#52899=CARTESIAN_POINT('Ctrl Pts',(6.45508636861402,-9.47833876217847,-37.8321045685465));
#52900=CARTESIAN_POINT('Ctrl Pts',(6.9076663195535,-9.54931802126756,-37.8126045589407));
#52901=CARTESIAN_POINT('Ctrl Pts',(7.03285856585593,-9.56967214728074,-37.8073454003161));
#52902=CARTESIAN_POINT('Ctrl Pts',(7.2691953296767,-9.61118811110219,-37.7970553432032));
#52903=CARTESIAN_POINT('Ctrl Pts',(7.56740105178408,-9.66979660166033,-37.7831896546061));
#52904=CARTESIAN_POINT('Ctrl Pts',(7.91660842131089,-9.75114654641155,-37.7640408695922));
#52905=CARTESIAN_POINT('Ctrl Pts',(8.37351535097609,-9.87701212539291,-37.7335242639715));
#52906=CARTESIAN_POINT('Ctrl Pts',(8.92109193346782,-10.070823088101,-37.6831357925027));
#52907=CARTESIAN_POINT('Ctrl Pts',(9.3283399907512,-10.2725679422737,-37.6241111672603));
#52908=CARTESIAN_POINT('Ctrl Pts',(9.97668494845576,-10.6540371711336,-37.5058782148325));
#52909=CARTESIAN_POINT('Ctrl Pts',(10.6788554165274,-11.2439508033002,-37.3411579803345));
#52910=CARTESIAN_POINT('Ctrl Pts',(11.6082441119523,-12.2454537985995,-37.030864103448));
#52911=CARTESIAN_POINT('Ctrl Pts',(12.0641366410534,-12.7793441548631,-36.8463749959916));
#52912=CARTESIAN_POINT('Ctrl Pts',(12.5649391142128,-13.3729973335818,-36.6246423121547));
#52913=CARTESIAN_POINT('Ctrl Pts',(13.0665672847697,-14.0319733807286,-36.3754643696926));
#52914=CARTESIAN_POINT('Ctrl Pts',(14.052339822417,-15.5260272045887,-35.7817417873778));
#52915=CARTESIAN_POINT('Ctrl Pts',(14.7427747351421,-16.7279921888766,-35.2435532673183));
#52916=CARTESIAN_POINT('Ctrl Pts',(15.478585307449,-17.9887566041688,-34.5924957389832));
#52917=CARTESIAN_POINT('Ctrl Pts',(15.9996615571876,-18.9401568844199,-34.0834579338314));
#52918=CARTESIAN_POINT('Ctrl Pts',(16.9995120437242,-20.9301248352716,-32.9291013640743));
#52919=CARTESIAN_POINT('Ctrl Pts',(17.6981753134392,-22.4269478260738,-31.9300105678004));
#52920=CARTESIAN_POINT('Ctrl Pts',(18.4357263982027,-23.9473093246625,-30.7724847771855));
#52921=CARTESIAN_POINT('Ctrl Pts',(18.9608339174453,-25.0715521287826,-29.8738096356868));
#52922=CARTESIAN_POINT('Ctrl Pts',(19.9653539792613,-27.310810104301,-27.8923455557466));
#52923=CARTESIAN_POINT('Ctrl Pts',(20.6729500616029,-28.8971249702565,-26.2354633096799));
#52924=CARTESIAN_POINT('Ctrl Pts',(22.3680345174968,-32.3930758837889,-22.016595619137));
#52925=CARTESIAN_POINT('Ctrl Pts',(23.4757593035169,-34.4841356290003,-18.5166596137722));
#52926=CARTESIAN_POINT('Ctrl Pts',(24.4767076204831,-36.1644175597347,-14.5403550674526));
#52927=CARTESIAN_POINT('',(3.2,-9.24182505978395,-36.4465179346992));
#52928=CARTESIAN_POINT('Ctrl Pts',(3.2,-9.24182505978396,-36.4465179346992));
#52929=CARTESIAN_POINT('Ctrl Pts',(3.45174020132946,-9.06882103761919,-35.6885377881604));
#52930=CARTESIAN_POINT('Ctrl Pts',(3.71840125362201,-8.8937755557219,-34.9216134221298));
#52931=CARTESIAN_POINT('Ctrl Pts',(4.,-8.71775829923915,-34.1504314334527));
#52932=CARTESIAN_POINT('Ctrl Pts',(4.62816481100596,-8.32511505038087,-32.4301489591897));
#52933=CARTESIAN_POINT('Ctrl Pts',(5.3258296688808,-7.87421940038907,-30.7255530003983));
#52934=CARTESIAN_POINT('Ctrl Pts',(6.03866107788435,-7.51769424249301,-29.1403169479585));
#52935=CARTESIAN_POINT('Ctrl Pts',(6.32798217848354,-7.37298926769682,-28.4969078141739));
#52936=CARTESIAN_POINT('Ctrl Pts',(6.61604116639212,-7.24664165658202,-27.8802695301434));
#52937=CARTESIAN_POINT('Ctrl Pts',(6.89476148100327,-7.14787574329671,-27.300072414889));
#52938=CARTESIAN_POINT('Ctrl Pts',(7.65522892931241,-6.87840036558412,-25.7170481549983));
#52939=CARTESIAN_POINT('Ctrl Pts',(8.35226709412095,-6.70318404327883,-24.4283041728914));
#52940=CARTESIAN_POINT('Ctrl Pts',(8.78926323759003,-6.62195963494359,-23.6418688208757));
#52941=CARTESIAN_POINT('Ctrl Pts',(8.99031957655721,-6.58458932305704,-23.2800399693545));
#52942=CARTESIAN_POINT('Ctrl Pts',(9.18275521872759,-6.55559338009954,-22.9406688489254));
#52943=CARTESIAN_POINT('Ctrl Pts',(9.37496045616592,-6.53433836529711,-22.6068036124997));
#52944=CARTESIAN_POINT('Ctrl Pts',(9.48075232992955,-6.52263937169636,-22.4230405193771));
#52945=CARTESIAN_POINT('Ctrl Pts',(9.5862609074853,-6.51335864091999,-22.2413624031642));
#52946=CARTESIAN_POINT('Ctrl Pts',(9.69257910363365,-6.50683293166549,-22.0596557590578));
#52947=CARTESIAN_POINT('Ctrl Pts',(10.0319880466963,-6.48600033516701,-21.4795776326612));
#52948=CARTESIAN_POINT('Ctrl Pts',(10.3788056739135,-6.49425759660125,-20.8988170113787));
#52949=CARTESIAN_POINT('Ctrl Pts',(10.7756849082151,-6.52753448251735,-20.2533506733983));
#52950=CARTESIAN_POINT('Ctrl Pts',(10.8890930402954,-6.53704334351844,-20.0689088447904));
#52951=CARTESIAN_POINT('Ctrl Pts',(11.0576203521665,-6.55312978036577,-19.7960739175289));
#52952=CARTESIAN_POINT('Ctrl Pts',(11.2725125494692,-6.57904145901406,-19.4548645888988));
#52953=CARTESIAN_POINT('Ctrl Pts',(11.5968279594503,-6.61814737718885,-18.9399113021204));
#52954=CARTESIAN_POINT('Ctrl Pts',(12.025567884427,-6.6827471737312,-18.2703586753637));
#52955=CARTESIAN_POINT('Ctrl Pts',(12.532035905153,-6.75393793425464,-17.5203993948461));
#52956=CARTESIAN_POINT('Ctrl Pts',(13.0988763177885,-6.83361483076056,-16.6810428893375));
#52957=CARTESIAN_POINT('Ctrl Pts',(13.7495416920733,-6.97877204198315,-15.7393500659831));
#52958=CARTESIAN_POINT('Ctrl Pts',(14.4398764944186,-7.14095491661005,-14.7876869742977));
#52959=CARTESIAN_POINT('Ctrl Pts',(14.7901814040927,-7.2232533275461,-14.3047731008548));
#52960=CARTESIAN_POINT('Ctrl Pts',(15.1459546154366,-7.30586903884694,-13.8278491968692));
#52961=CARTESIAN_POINT('Ctrl Pts',(15.4570717747561,-7.37026799935016,-13.4241590170948));
#52962=CARTESIAN_POINT('Ctrl Pts',(15.7998231401197,-7.44121500750863,-12.9794218621136));
#52963=CARTESIAN_POINT('Ctrl Pts',(16.0676294483849,-7.50355110660171,-12.637469237209));
#52964=CARTESIAN_POINT('Ctrl Pts',(16.3615307957941,-7.57387201213481,-12.2669409047598));
#52965=CARTESIAN_POINT('Ctrl Pts',(17.0296616012911,-7.73373369249551,-11.4246127038138));
#52966=CARTESIAN_POINT('Ctrl Pts',(17.7084691868929,-7.91242588701926,-10.5936031634317));
#52967=CARTESIAN_POINT('Ctrl Pts',(18.4207032016838,-8.06194162094658,-9.78641628469765));
#52968=CARTESIAN_POINT('Ctrl Pts',(18.8298642041889,-8.14783474920716,-9.32270718677038));
#52969=CARTESIAN_POINT('Ctrl Pts',(19.2113759272395,-8.23555418397616,-8.8952152917086));
#52970=CARTESIAN_POINT('Ctrl Pts',(19.5701113607057,-8.31748924110769,-8.49743627926558));
#52971=CARTESIAN_POINT('Ctrl Pts',(20.121547602182,-8.44343710054603,-7.88598353973464));
#52972=CARTESIAN_POINT('Ctrl Pts',(20.6514912601917,-8.57040043767199,-7.29974693210948));
#52973=CARTESIAN_POINT('Ctrl Pts',(21.3979544325339,-8.70094314511465,-6.5286488228905));
#52974=CARTESIAN_POINT('Ctrl Pts',(21.8107631282201,-8.77313580884871,-6.10221652655357));
#52975=CARTESIAN_POINT('Ctrl Pts',(22.3076315955579,-8.85489558536126,-5.5960154347174));
#52976=CARTESIAN_POINT('Ctrl Pts',(22.8472772295406,-8.93355440585529,-5.03999075031881));
#52977=CARTESIAN_POINT('Ctrl Pts',(23.3953136568816,-9.01343626952248,-4.47532059946028));
#52978=CARTESIAN_POINT('Ctrl Pts',(23.9608264583214,-9.08615837741543,-3.88432348473261));
#52979=CARTESIAN_POINT('Ctrl Pts',(24.5,-9.13966689904905,-3.29104195297002));
#52980=CARTESIAN_POINT('Ctrl Pts',(2.7975955995408,-9.45110532887384,-37.363642330079));
#52981=CARTESIAN_POINT('Ctrl Pts',(2.93204421046394,-9.3813783568972,-37.0582190820374));
#52982=CARTESIAN_POINT('Ctrl Pts',(3.06669822891363,-9.31156415154198,-36.7524257548829));
#52983=CARTESIAN_POINT('Ctrl Pts',(3.20140554545437,-9.24173281535836,-36.4465583754197));
#52984=CARTESIAN_POINT('Origin',(2.9,0.,0.));
#52985=CARTESIAN_POINT('Origin',(3.2,0.,0.));
#52986=CARTESIAN_POINT('Ctrl Pts',(2.1,-8.3510594145214,-5.02058289194443));
#52987=CARTESIAN_POINT('Ctrl Pts',(2.73333333333334,-8.3510594145214,-5.02058289194443));
#52988=CARTESIAN_POINT('Ctrl Pts',(3.36630413798689,-8.35107248850531,-5.02053567019918));
#52989=CARTESIAN_POINT('Ctrl Pts',(4.124157833359,-8.35107634006013,-5.0205214484641));
#52990=CARTESIAN_POINT('Ctrl Pts',(4.36790635424917,-8.3504576041077,-5.02157407473443));
#52991=CARTESIAN_POINT('Ctrl Pts',(4.86513593837425,-8.34763711932882,-5.02638994376713));
#52992=CARTESIAN_POINT('Ctrl Pts',(5.74555319889928,-8.3409895121078,-5.03776769314777));
#52993=CARTESIAN_POINT('Ctrl Pts',(6.51831486887852,-8.34088452878131,-5.03795859267391));
#52994=CARTESIAN_POINT('Ctrl Pts',(7.10304244324289,-8.35279167464714,-5.01737867305202));
#52995=CARTESIAN_POINT('Ctrl Pts',(7.23019749510073,-8.35551879167041,-5.01278329615679));
#52996=CARTESIAN_POINT('Ctrl Pts',(7.4248770951455,-8.36007698205955,-5.00525711413222));
#52997=CARTESIAN_POINT('Ctrl Pts',(7.61944598119582,-8.36505833151271,-4.99715327807895));
#52998=CARTESIAN_POINT('Ctrl Pts',(8.0106922175681,-8.37596024104948,-4.97952710685782));
#52999=CARTESIAN_POINT('Ctrl Pts',(8.6007456943798,-8.39597936834588,-4.94716218491378));
#53000=CARTESIAN_POINT('Ctrl Pts',(9.25144198408345,-8.42603538580927,-4.89603670853206));
#53001=CARTESIAN_POINT('Ctrl Pts',(9.7625585744136,-8.45565760052341,-4.84294672360393));
#53002=CARTESIAN_POINT('Ctrl Pts',(10.014053299629,-8.47250040429509,-4.81175577398779));
#53003=CARTESIAN_POINT('Ctrl Pts',(10.7175941211066,-8.52323302742723,-4.71611549795234));
#53004=CARTESIAN_POINT('Ctrl Pts',(11.8206443092623,-8.6410972085384,-4.50214846820936));
#53005=CARTESIAN_POINT('Ctrl Pts',(12.8076886876858,-8.77604098409547,-4.23317354676162));
#53006=CARTESIAN_POINT('Ctrl Pts',(13.5599769262593,-8.87234107283724,-4.01612216898111));
#53007=CARTESIAN_POINT('Ctrl Pts',(14.1409849758931,-8.95311652054028,-3.82954437668286));
#53008=CARTESIAN_POINT('Ctrl Pts',(15.2001160349016,-9.11712726893695,-3.42890798831576));
#53009=CARTESIAN_POINT('Ctrl Pts',(15.9274644685005,-9.23361588248013,-3.10300037073481));
#53010=CARTESIAN_POINT('Ctrl Pts',(16.5321322282548,-9.3168092748402,-2.82432638267735));
#53011=CARTESIAN_POINT('Ctrl Pts',(16.8247613473468,-9.35683848526952,-2.68420632115728));
#53012=CARTESIAN_POINT('Ctrl Pts',(17.3791193144645,-9.43288731616673,-2.40020239788725));
#53013=CARTESIAN_POINT('Ctrl Pts',(18.3031725170504,-9.55581141304687,-1.88358773747688));
#53014=CARTESIAN_POINT('Ctrl Pts',(19.0238031811775,-9.63350132918122,-1.42657286581671));
#53015=CARTESIAN_POINT('Ctrl Pts',(19.7685846204969,-9.68548144316729,-0.948296989745364));
#53016=CARTESIAN_POINT('Ctrl Pts',(20.3333458124559,-9.71634622220616,-0.563870996202872));
#53017=CARTESIAN_POINT('Ctrl Pts',(21.3725234028357,-9.73790831668593,0.208452027128235));
#53018=CARTESIAN_POINT('Ctrl Pts',(22.0963502964542,-9.70493456228337,0.792620452508349));
#53019=CARTESIAN_POINT('Ctrl Pts',(23.2302898490711,-9.58941316697602,1.6990553747534));
#53020=CARTESIAN_POINT('Ctrl Pts',(23.8854423668127,-9.47051557491202,2.24929142641503));
#53021=CARTESIAN_POINT('Ctrl Pts',(24.5000000001022,-9.30357389606071,2.79427645741834));
#53022=CARTESIAN_POINT('Ctrl Pts',(2.1,-12.1206304302549,-6.83591261691419));
#53023=CARTESIAN_POINT('Ctrl Pts',(2.73333333333334,-12.1206304302549,-6.83591261691419));
#53024=CARTESIAN_POINT('Ctrl Pts',(3.36610615421361,-12.1206479194635,-6.83586470096514));
#53025=CARTESIAN_POINT('Ctrl Pts',(4.12374023994246,-12.1206529672983,-6.83585065866281));
#53026=CARTESIAN_POINT('Ctrl Pts',(4.36463581418031,-12.119818089853,-6.83736864158517));
#53027=CARTESIAN_POINT('Ctrl Pts',(4.85997530319406,-12.1159950337854,-6.84434016223762));
#53028=CARTESIAN_POINT('Ctrl Pts',(5.74109948643887,-12.1069511492505,-6.86086278899071));
#53029=CARTESIAN_POINT('Ctrl Pts',(6.52363773254301,-12.1067466533597,-6.8612742309798));
#53030=CARTESIAN_POINT('Ctrl Pts',(7.12000347701033,-12.1231781285262,-6.83101297830123));
#53031=CARTESIAN_POINT('Ctrl Pts',(7.24730650466272,-12.1268928519257,-6.82433786894958));
#53032=CARTESIAN_POINT('Ctrl Pts',(7.44359013132278,-12.1331371694334,-6.81335481350602));
#53033=CARTESIAN_POINT('Ctrl Pts',(7.63950249952398,-12.1399592237706,-6.80153737160822));
#53034=CARTESIAN_POINT('Ctrl Pts',(8.03411798341277,-12.1549085762698,-6.77580415828938));
#53035=CARTESIAN_POINT('Ctrl Pts',(8.63043086897818,-12.1823946115809,-6.72851622753706));
#53036=CARTESIAN_POINT('Ctrl Pts',(9.29097699605177,-12.2237061185676,-6.65361492414508));
#53037=CARTESIAN_POINT('Ctrl Pts',(9.81195534428169,-12.2644669019274,-6.57562981851048));
#53038=CARTESIAN_POINT('Ctrl Pts',(10.0691242294032,-12.2876662270862,-6.5297284806116));
#53039=CARTESIAN_POINT('Ctrl Pts',(10.7899280908924,-12.3576002597858,-6.38885954025546));
#53040=CARTESIAN_POINT('Ctrl Pts',(11.9161536741519,-12.5198279076047,-6.07413534771085));
#53041=CARTESIAN_POINT('Ctrl Pts',(12.9129363927331,-12.7028957202776,-5.68195632485753));
#53042=CARTESIAN_POINT('Ctrl Pts',(13.6692202156514,-12.8320205003908,-5.36700676384535));
#53043=CARTESIAN_POINT('Ctrl Pts',(14.2625054221329,-12.9416375398882,-5.09326044189235));
#53044=CARTESIAN_POINT('Ctrl Pts',(15.3322025816006,-13.1612208212938,-4.50953050507395));
#53045=CARTESIAN_POINT('Ctrl Pts',(16.0642045996111,-13.314626073984,-4.0376815807855));
#53046=CARTESIAN_POINT('Ctrl Pts',(16.6699064173536,-13.4217056458658,-3.63594477391126));
#53047=CARTESIAN_POINT('Ctrl Pts',(16.9656071732736,-13.4736500463097,-3.43229235011708));
#53048=CARTESIAN_POINT('Ctrl Pts',(17.5230947907728,-13.5709657994867,-3.02137001298369));
#53049=CARTESIAN_POINT('Ctrl Pts',(18.4506751005994,-13.7254773647144,-2.27570397276808));
#53050=CARTESIAN_POINT('Ctrl Pts',(19.1721322371942,-13.817061020641,-1.61983850524452));
#53051=CARTESIAN_POINT('Ctrl Pts',(19.9178174487373,-13.8707061847774,-0.934528745352126));
#53052=CARTESIAN_POINT('Ctrl Pts',(20.4828456339096,-13.8989929725084,-0.38350142317537));
#53053=CARTESIAN_POINT('Ctrl Pts',(21.519673087749,-13.8969871998656,0.719259828124072));
#53054=CARTESIAN_POINT('Ctrl Pts',(22.2434457172006,-13.8253355648101,1.55134793540283));
#53055=CARTESIAN_POINT('Ctrl Pts',(23.3781345297088,-13.6212597999766,2.84098795851428));
#53056=CARTESIAN_POINT('Ctrl Pts',(24.0312127056184,-13.4291220347533,3.62028744621722));
#53057=CARTESIAN_POINT('Ctrl Pts',(24.6419825553303,-13.1689424018865,4.38882031378994));
#53058=CARTESIAN_POINT('Ctrl Pts',(2.1,-20.916296133633,-11.071681975177));
#53059=CARTESIAN_POINT('Ctrl Pts',(2.73333333333333,-20.916296133633,-11.071681975177));
#53060=CARTESIAN_POINT('Ctrl Pts',(3.36563013999952,-20.9163457636086,-11.0715181247485));
#53061=CARTESIAN_POINT('Ctrl Pts',(4.12274830451023,-20.9163601418624,-11.0714694821853));
#53062=CARTESIAN_POINT('Ctrl Pts',(4.35698360829913,-20.9150398098762,-11.0740285474474));
#53063=CARTESIAN_POINT('Ctrl Pts',(4.84792376014415,-20.9089149916327,-11.085938742644));
#53064=CARTESIAN_POINT('Ctrl Pts',(5.73065667640276,-20.89427786353,-11.1144517034764));
#53065=CARTESIAN_POINT('Ctrl Pts',(6.536083377971,-20.8937138528347,-11.1155451125587));
#53066=CARTESIAN_POINT('Ctrl Pts',(7.15933923661711,-20.9213295292238,-11.0613487798922));
#53067=CARTESIAN_POINT('Ctrl Pts',(7.2869825297321,-20.9273577920289,-11.0497993277066));
#53068=CARTESIAN_POINT('Ctrl Pts',(7.48696545484876,-20.9376292512005,-11.0305502319027));
#53069=CARTESIAN_POINT('Ctrl Pts',(7.68596619463735,-20.9488334483803,-11.0098765165954));
#53070=CARTESIAN_POINT('Ctrl Pts',(8.0883162475225,-20.9734544781764,-10.9647379230039));
#53071=CARTESIAN_POINT('Ctrl Pts',(8.6988777287627,-21.0188908195159,-10.881420270716));
#53072=CARTESIAN_POINT('Ctrl Pts',(9.38136707068581,-21.0875686323605,-10.7485587482729));
#53073=CARTESIAN_POINT('Ctrl Pts',(9.92336660942117,-21.1557256018479,-10.6092802056132));
#53074=CARTESIAN_POINT('Ctrl Pts',(10.192104163104,-21.1946784819422,-10.5269158804284));
#53075=CARTESIAN_POINT('Ctrl Pts',(10.9468601756432,-21.312453368427,-10.2732554098091));
#53076=CARTESIAN_POINT('Ctrl Pts',(12.1070011864937,-21.5827620184303,-9.71110981143062));
#53077=CARTESIAN_POINT('Ctrl Pts',(13.1090760677711,-21.877961857721,-9.02824401297635));
#53078=CARTESIAN_POINT('Ctrl Pts',(13.8680231110403,-22.0833622460056,-8.48292378218801));
#53079=CARTESIAN_POINT('Ctrl Pts',(14.4653877431462,-22.2597779663279,-8.00456661480236));
#53080=CARTESIAN_POINT('Ctrl Pts',(15.5287361352249,-22.6051540387014,-7.00111172304811));
#53081=CARTESIAN_POINT('Ctrl Pts',(16.2553457094708,-22.8424976951966,-6.1930675108659));
#53082=CARTESIAN_POINT('Ctrl Pts',(16.859621896458,-23.0044889456917,-5.50458274371019));
#53083=CARTESIAN_POINT('Ctrl Pts',(17.1500351055466,-23.0826150095401,-5.1590775027475));
#53084=CARTESIAN_POINT('Ctrl Pts',(17.6990188169006,-23.2273294355939,-4.46234792132739));
#53085=CARTESIAN_POINT('Ctrl Pts',(18.611272879964,-23.452715685408,-3.20153979794507));
#53086=CARTESIAN_POINT('Ctrl Pts',(19.3245661130779,-23.5769499724595,-2.09052262543805));
#53087=CARTESIAN_POINT('Ctrl Pts',(20.0670920275141,-23.6354019998513,-0.924514657719357));
#53088=CARTESIAN_POINT('Ctrl Pts',(20.6170292347668,-23.6585283665091,-0.00486191135603094));
#53089=CARTESIAN_POINT('Ctrl Pts',(21.6396453273267,-23.6076069577787,1.84844937703413));
#53090=CARTESIAN_POINT('Ctrl Pts',(22.3556274201432,-23.4509610643206,3.24991333715251));
#53091=CARTESIAN_POINT('Ctrl Pts',(23.4868198684743,-23.0476613191845,5.43142402662265));
#53092=CARTESIAN_POINT('Ctrl Pts',(24.1253594022045,-22.6935861225115,6.72605099589447));
#53093=CARTESIAN_POINT('Ctrl Pts',(24.7277792021545,-22.2267622806559,8.00674483047698));
#53094=CARTESIAN_POINT('Ctrl Pts',(2.1,-29.7119618370111,-15.3074513334397));
#53095=CARTESIAN_POINT('Ctrl Pts',(2.73333333333334,-29.7119618370111,-15.3074513334397));
#53096=CARTESIAN_POINT('Ctrl Pts',(3.36509601826733,-29.7119996481889,-15.3073119398028));
#53097=CARTESIAN_POINT('Ctrl Pts',(4.12168472859039,-29.712009343078,-15.3072731750119));
#53098=CARTESIAN_POINT('Ctrl Pts',(4.34924335783325,-29.7102392280698,-15.3108028413304));
#53099=CARTESIAN_POINT('Ctrl Pts',(4.83584443000053,-29.7018839707635,-15.3275145646124));
#53100=CARTESIAN_POINT('Ctrl Pts',(5.71997740106937,-29.6816141052182,-15.3681101299536));
#53101=CARTESIAN_POINT('Ctrl Pts',(6.5487109251882,-29.6802918349395,-15.3707901137388));
#53102=CARTESIAN_POINT('Ctrl Pts',(7.19748317953822,-29.7204144003175,-15.2899276431913));
#53103=CARTESIAN_POINT('Ctrl Pts',(7.32544141258867,-29.7287738602123,-15.2734650442013));
#53104=CARTESIAN_POINT('Ctrl Pts',(7.52889917711157,-29.7432671926898,-15.2455421685912));
#53105=CARTESIAN_POINT('Ctrl Pts',(7.73075278971052,-29.7590297130559,-15.2156417671467));
#53106=CARTESIAN_POINT('Ctrl Pts',(8.14018479960674,-29.7937920094793,-15.1501008270889));
#53107=CARTESIAN_POINT('Ctrl Pts',(8.76324628290073,-29.858127960699,-15.028769624718));
#53108=CARTESIAN_POINT('Ctrl Pts',(9.46271315458471,-29.9559850568587,-14.8339981039036));
#53109=CARTESIAN_POINT('Ctrl Pts',(10.0175769787051,-30.0531863854985,-14.6296699075059));
#53110=CARTESIAN_POINT('Ctrl Pts',(10.2918333022463,-30.1086127962716,-14.5091281203088));
#53111=CARTESIAN_POINT('Ctrl Pts',(11.0595910066927,-30.2757018898991,-14.139070342574));
#53112=CARTESIAN_POINT('Ctrl Pts',(12.2112473457141,-30.648937612004,-13.3398925023309));
#53113=CARTESIAN_POINT('Ctrl Pts',(13.2033007010659,-31.0506537341638,-12.3812952012109));
#53114=CARTESIAN_POINT('Ctrl Pts',(13.9586007016383,-31.3305216353669,-11.6113351262395));
#53115=CARTESIAN_POINT('Ctrl Pts',(14.542598746085,-31.5670881163489,-10.9487986651389));
#53116=CARTESIAN_POINT('Ctrl Pts',(15.5913195536334,-32.0323898578073,-9.55125247564053));
#53117=CARTESIAN_POINT('Ctrl Pts',(16.3119173380708,-32.3531230926996,-8.41971069656156));
#53118=CARTESIAN_POINT('Ctrl Pts',(16.9149851983179,-32.5715645453592,-7.44764363908721));
#53119=CARTESIAN_POINT('Ctrl Pts',(17.2005121433669,-32.6749740884606,-6.96982244605168));
#53120=CARTESIAN_POINT('Ctrl Pts',(17.7438798901797,-32.8675630371451,-5.99886958229992));
#53121=CARTESIAN_POINT('Ctrl Pts',(18.6483251207895,-33.1666438231165,-4.23939596515499));
#53122=CARTESIAN_POINT('Ctrl Pts',(19.3595640666469,-33.3289092906231,-2.67776204570037));
#53123=CARTESIAN_POINT('Ctrl Pts',(20.101201047881,-33.3977844233599,-1.03303550949749));
#53124=CARTESIAN_POINT('Ctrl Pts',(20.6467829307123,-33.420235639171,0.247408307787539));
#53125=CARTESIAN_POINT('Ctrl Pts',(21.6665635858478,-33.3304451498286,2.84833137837582));
#53126=CARTESIAN_POINT('Ctrl Pts',(22.3811269169302,-33.0965818169693,4.81920574759241));
#53127=CARTESIAN_POINT('Ctrl Pts',(23.5117933107515,-32.5060407355254,7.89489191625015));
#53128=CARTESIAN_POINT('Ctrl Pts',(24.1480627906507,-31.997321521606,9.70668778292231));
#53129=CARTESIAN_POINT('Ctrl Pts',(24.7493903499091,-31.3302490010767,11.5032773646064));
#53130=CARTESIAN_POINT('Ctrl Pts',(2.1,-34.7380565246557,-17.7278909667327));
#53131=CARTESIAN_POINT('Ctrl Pts',(2.73333333333334,-34.7380565246557,-17.7278909667327));
#53132=CARTESIAN_POINT('Ctrl Pts',(3.36477003909008,-34.7380878504292,-17.7277685453303));
#53133=CARTESIAN_POINT('Ctrl Pts',(4.12105218050017,-34.7380950530209,-17.7277361764495));
#53134=CARTESIAN_POINT('Ctrl Pts',(4.34478769127088,-34.7360800768833,-17.7317954189765));
#53135=CARTESIAN_POINT('Ctrl Pts',(4.82894448622196,-34.7264782440274,-17.7511938998242));
#53136=CARTESIAN_POINT('Ctrl Pts',(5.71376767624365,-34.7029725862593,-17.798729519981));
#53137=CARTESIAN_POINT('Ctrl Pts',(6.55605736789038,-34.7011333795005,-17.8024966972734));
#53138=CARTESIAN_POINT('Ctrl Pts',(7.21867968559155,-34.7487778314302,-17.70561610612));
#53139=CARTESIAN_POINT('Ctrl Pts',(7.34680477302365,-34.758474208368,-17.6863351682917));
#53140=CARTESIAN_POINT('Ctrl Pts',(7.55212973160944,-34.7754330759594,-17.6533440413737));
#53141=CARTESIAN_POINT('Ctrl Pts',(7.75549216232999,-34.7938463390146,-17.6180735588395));
#53142=CARTESIAN_POINT('Ctrl Pts',(8.16863486466037,-34.8345191663954,-17.5406274875346));
#53143=CARTESIAN_POINT('Ctrl Pts',(8.79798512181356,-34.9098733771466,-17.3971072068904));
#53144=CARTESIAN_POINT('Ctrl Pts',(9.50495252296997,-35.0246122080616,-17.1664851984444));
#53145=CARTESIAN_POINT('Ctrl Pts',(10.0643544361655,-35.1382513636705,-16.9253010933509));
#53146=CARTESIAN_POINT('Ctrl Pts',(10.3400749108932,-35.2028268310511,-16.78351345817));
#53147=CARTESIAN_POINT('Ctrl Pts',(11.1102097451852,-35.3969765538676,-16.3494142249521));
#53148=CARTESIAN_POINT('Ctrl Pts',(12.2544661012045,-35.8260061974632,-15.4220345473532));
#53149=CARTESIAN_POINT('Ctrl Pts',(13.2427201344581,-36.2882744174662,-14.3078780733756));
#53150=CARTESIAN_POINT('Ctrl Pts',(13.9962152001074,-36.6106546545614,-13.410529882366));
#53151=CARTESIAN_POINT('Ctrl Pts',(14.5751544918282,-36.8812387280998,-12.6446491994453));
#53152=CARTESIAN_POINT('Ctrl Pts',(15.6190053721497,-37.4158411932568,-11.0215866115973));
#53153=CARTESIAN_POINT('Ctrl Pts',(16.3369858202403,-37.7847218374664,-9.7052068333357));
#53154=CARTESIAN_POINT('Ctrl Pts',(16.9394528589127,-38.0357988868014,-8.57126361777627));
#53155=CARTESIAN_POINT('Ctrl Pts',(17.2231900082674,-38.1539748657828,-8.01721712860961));
#53156=CARTESIAN_POINT('Ctrl Pts',(17.7643466428736,-38.3744634463336,-6.88860604294098));
#53157=CARTESIAN_POINT('Ctrl Pts',(18.665416776174,-38.7164782056892,-4.8425562907444));
#53158=CARTESIAN_POINT('Ctrl Pts',(19.3755688464135,-38.9009629285056,-3.02324311837983));
#53159=CARTESIAN_POINT('Ctrl Pts',(20.1168542434801,-38.9762754008698,-1.10510187804403));
#53160=CARTESIAN_POINT('Ctrl Pts',(20.6601247471566,-38.9987110260548,0.382680871312569));
#53161=CARTESIAN_POINT('Ctrl Pts',(21.6779306238709,-38.8871436088383,3.41175861162423));
#53162=CARTESIAN_POINT('Ctrl Pts',(22.3918707612037,-38.6096537271056,5.70820384366463));
#53163=CARTESIAN_POINT('Ctrl Pts',(23.5225369684879,-37.9128210548167,9.29489384117657));
#53164=CARTESIAN_POINT('Ctrl Pts',(24.157514841919,-37.3161464202365,11.4028407975047));
#53165=CARTESIAN_POINT('Ctrl Pts',(24.7577717974218,-36.5347967417974,13.4945033583609));
#53166=CARTESIAN_POINT('',(24.5,-9.30357389617668,2.7942764573609));
#53167=CARTESIAN_POINT('Ctrl Pts',(24.5,-9.30357389617668,2.7942764573609));
#53168=CARTESIAN_POINT('Ctrl Pts',(23.8274939346328,-9.6593359457179,2.26301432768217));
#53169=CARTESIAN_POINT('Ctrl Pts',(23.3366347313422,-9.90209213544415,1.88769087309693));
#53170=CARTESIAN_POINT('Ctrl Pts',(22.5855494187791,-10.2761542512457,1.30496983260268));
#53171=CARTESIAN_POINT('Ctrl Pts',(22.2454144272606,-10.4455512724061,1.04107994839));
#53172=CARTESIAN_POINT('Ctrl Pts',(21.838266074389,-10.649002408715,0.713024067302568));
#53173=CARTESIAN_POINT('Ctrl Pts',(21.380215694946,-10.8812747542395,0.336360818335602));
#53174=CARTESIAN_POINT('Ctrl Pts',(20.7694693292298,-11.1909775669692,-0.165867147691021));
#53175=CARTESIAN_POINT('Ctrl Pts',(20.162900303303,-11.5043313797733,-0.671800812422079));
#53176=CARTESIAN_POINT('Ctrl Pts',(19.5574857571565,-11.8416668907066,-1.16282656860098));
#53177=CARTESIAN_POINT('Ctrl Pts',(18.6418529409967,-12.3518552663123,-1.90545705014252));
#53178=CARTESIAN_POINT('Ctrl Pts',(17.7734813310041,-12.8807069946298,-2.69008889779871));
#53179=CARTESIAN_POINT('Ctrl Pts',(16.9621253090967,-13.4407209233415,-3.40811169367996));
#53180=CARTESIAN_POINT('Ctrl Pts',(16.8133360656621,-13.5434181937333,-3.53978517077668));
#53181=CARTESIAN_POINT('Ctrl Pts',(16.6656205363151,-13.6476856017606,-3.67035910850337));
#53182=CARTESIAN_POINT('Ctrl Pts',(16.5183901926363,-13.7540617624745,-3.80017688100675));
#53183=CARTESIAN_POINT('Ctrl Pts',(15.7264522887166,-14.3262489328485,-4.49845423388844));
#53184=CARTESIAN_POINT('Ctrl Pts',(14.9462259719641,-14.9411217657404,-5.26355621040781));
#53185=CARTESIAN_POINT('Ctrl Pts',(14.2963150415374,-15.5054551326937,-5.88914684389902));
#53186=CARTESIAN_POINT('Ctrl Pts',(13.9908350934413,-15.7707107540026,-6.18319543625432));
#53187=CARTESIAN_POINT('Ctrl Pts',(13.7077063567062,-16.0287137800868,-6.45459111782661));
#53188=CARTESIAN_POINT('Ctrl Pts',(13.4460198946299,-16.2769490901149,-6.70287044942663));
#53189=CARTESIAN_POINT('Ctrl Pts',(12.8373295405702,-16.8543516716327,-7.28037542640655));
#53190=CARTESIAN_POINT('Ctrl Pts',(12.3530827409722,-17.3494543756252,-7.77107105609639));
#53191=CARTESIAN_POINT('Ctrl Pts',(11.9770275688693,-17.7511354620811,-8.14810202886081));
#53192=CARTESIAN_POINT('Ctrl Pts',(11.6553972429219,-18.0946829741158,-8.4705669320408));
#53193=CARTESIAN_POINT('Ctrl Pts',(11.3684205615655,-18.4156350281444,-8.75884371968927));
#53194=CARTESIAN_POINT('Ctrl Pts',(11.071085678131,-18.7646456855957,-9.05375641021996));
#53195=CARTESIAN_POINT('Ctrl Pts',(10.8141787015647,-19.0662022058381,-9.30857053360867));
#53196=CARTESIAN_POINT('Ctrl Pts',(10.5576802661827,-19.3800705526631,-9.56028590215235));
#53197=CARTESIAN_POINT('Ctrl Pts',(10.2957959918397,-19.7169417339605,-9.81194913646659));
#53198=CARTESIAN_POINT('Ctrl Pts',(9.71459276345257,-20.4645643951982,-10.370468675743));
#53199=CARTESIAN_POINT('Ctrl Pts',(9.09527967376236,-21.3374886981073,-10.9426578680836));
#53200=CARTESIAN_POINT('Ctrl Pts',(8.43168033652658,-22.3859163093067,-11.5697730332091));
#53201=CARTESIAN_POINT('Ctrl Pts',(7.97964340480273,-23.1000942385303,-11.9969573282713));
#53202=CARTESIAN_POINT('Ctrl Pts',(7.52291961074464,-23.8750386166862,-12.4359459480503));
#53203=CARTESIAN_POINT('Ctrl Pts',(7.10363554125516,-24.632641914712,-12.8547349765663));
#53204=CARTESIAN_POINT('Ctrl Pts',(6.5632779955478,-25.6090125629922,-13.3944545320783));
#53205=CARTESIAN_POINT('Ctrl Pts',(6.08559840022222,-26.564462963399,-13.8602159500353));
#53206=CARTESIAN_POINT('Ctrl Pts',(5.6170867082795,-27.5711979548747,-14.333880928108));
#53207=CARTESIAN_POINT('Ctrl Pts',(5.04102956503258,-28.8090259390419,-14.9162742788338));
#53208=CARTESIAN_POINT('Ctrl Pts',(4.50102820503081,-30.086306522799,-15.4877262328007));
#53209=CARTESIAN_POINT('Ctrl Pts',(4.,-31.3543250987725,-16.098371795166));
#53210=CARTESIAN_POINT('Ctrl Pts',(3.72183418897184,-32.0583162354846,-16.4373960584719));
#53211=CARTESIAN_POINT('Ctrl Pts',(3.45538353518254,-32.7656113591521,-16.7780114380366));
#53212=CARTESIAN_POINT('Ctrl Pts',(3.2,-33.4762280926097,-17.1202264205697));
#53213=CARTESIAN_POINT('',(24.5,-25.5759818995428,8.65269610435146));
#53214=CARTESIAN_POINT('Ctrl Pts',(24.5,-25.5759818995428,8.65269610435144));
#53215=CARTESIAN_POINT('Ctrl Pts',(24.5,-24.4075774169203,8.24137805333807));
#53216=CARTESIAN_POINT('Ctrl Pts',(24.5,-23.2592813076738,7.83618130765631));
#53217=CARTESIAN_POINT('Ctrl Pts',(24.5,-18.5158678907521,6.15728495615527));
#53218=CARTESIAN_POINT('Ctrl Pts',(24.5,-13.4830088728325,4.36655158825629));
#53219=CARTESIAN_POINT('Ctrl Pts',(24.5,-9.30357389617668,2.7942764573609));
#53220=CARTESIAN_POINT('',(10.2670750393577,-30.770480162676,-14.8182822548653));
#53221=CARTESIAN_POINT('Ctrl Pts',(10.2670750393577,-30.770480162676,-14.8182822548653));
#53222=CARTESIAN_POINT('Ctrl Pts',(11.2293198185888,-30.1791102527654,-14.0169036234914));
#53223=CARTESIAN_POINT('Ctrl Pts',(12.092802582344,-29.8393707151449,-13.0968030075364));
#53224=CARTESIAN_POINT('Ctrl Pts',(14.3080979519049,-29.1888831332163,-10.4908414553475));
#53225=CARTESIAN_POINT('Ctrl Pts',(14.8952017874601,-29.0927432444532,-9.72024139342426));
#53226=CARTESIAN_POINT('Ctrl Pts',(17.0803363586062,-28.7592866386632,-6.39544722949815));
#53227=CARTESIAN_POINT('Ctrl Pts',(17.6922811489506,-28.6652489345692,-5.38383065662599));
#53228=CARTESIAN_POINT('Ctrl Pts',(19.0755427322033,-28.4267546017089,-2.90463394754129));
#53229=CARTESIAN_POINT('Ctrl Pts',(20.2687424742408,-28.1812035390717,-0.681869641908761));
#53230=CARTESIAN_POINT('Ctrl Pts',(22.3267279388309,-27.2670721892073,3.7530051527172));
#53231=CARTESIAN_POINT('Ctrl Pts',(23.4192562717209,-26.6256746472157,6.1252840113241));
#53232=CARTESIAN_POINT('Ctrl Pts',(24.5,-25.5759818995428,8.65269610435144));
#53233=CARTESIAN_POINT('Ctrl Pts',(6.,-34.705361282547,-17.7915119719457));
#53234=CARTESIAN_POINT('Ctrl Pts',(7.51604047332548,-32.7628371673734,-16.8524804320582));
#53235=CARTESIAN_POINT('Ctrl Pts',(9.08449301626627,-31.5752575158279,-15.7405257307418));
#53236=CARTESIAN_POINT('Ctrl Pts',(9.8624969752411,-31.0279962027639,-15.1470785535203));
#53237=CARTESIAN_POINT('Ctrl Pts',(10.0667253012216,-30.8936097541786,-14.9851379265292));
#53238=CARTESIAN_POINT('Ctrl Pts',(10.2670750393577,-30.770480162676,-14.8182822548653));
#53239=CARTESIAN_POINT('Origin',(24.5,-7.65823537717056,-3.68801178249924));
#53240=CARTESIAN_POINT('',(24.5,-8.27152931289795,5.09374822578144));
#53241=CARTESIAN_POINT('Ctrl Pts',(24.5,-8.27152931289795,5.09374822578144));
#53242=CARTESIAN_POINT('Ctrl Pts',(24.5,-8.44222149420361,4.81656817710801));
#53243=CARTESIAN_POINT('Ctrl Pts',(24.5,-8.59911506421257,4.53059124178116));
#53244=CARTESIAN_POINT('Ctrl Pts',(24.5,-8.96745037775474,3.77063565908301));
#53245=CARTESIAN_POINT('Ctrl Pts',(24.5,-9.15522875621099,3.28819321644671));
#53246=CARTESIAN_POINT('Ctrl Pts',(24.5,-9.30357389617668,2.7942764573609));
#53247=CARTESIAN_POINT('',(24.5,-23.4219747427337,13.431719888039));
#53248=CARTESIAN_POINT('Ctrl Pts',(24.5,-8.27152931289795,5.09374822578144));
#53249=CARTESIAN_POINT('Ctrl Pts',(24.5,-12.0766273202602,7.113542304172));
#53250=CARTESIAN_POINT('Ctrl Pts',(24.5,-17.1057664725757,9.89787449294439));
#53251=CARTESIAN_POINT('Ctrl Pts',(24.5,-23.4219747427337,13.4317198880391));
#53252=CARTESIAN_POINT('Origin',(24.5,0.,0.));
#53253=CARTESIAN_POINT('Ctrl Pts',(24.5,-23.4219746022546,13.4317201330038));
#53254=CARTESIAN_POINT('Ctrl Pts',(24.5,-30.4957974083931,1.09652430807625));
#53255=CARTESIAN_POINT('Ctrl Pts',(24.5,-24.3261594333653,-11.7148609561741));
#53256=CARTESIAN_POINT('Ctrl Pts',(24.5,-12.6112984771912,-36.0410203895394));
#53257=CARTESIAN_POINT('Ctrl Pts',(24.5,11.7148609561741,-24.3261594333653));
#53258=CARTESIAN_POINT('Ctrl Pts',(24.5,36.0410203895394,-12.6112984771912));
#53259=CARTESIAN_POINT('Ctrl Pts',(24.5,24.3261594333653,11.7148609561741));
#53260=CARTESIAN_POINT('Ctrl Pts',(24.5,12.6112984771912,36.0410203895394));
#53261=CARTESIAN_POINT('Ctrl Pts',(24.5,-11.7148609561741,24.3261594333653));
#53262=CARTESIAN_POINT('Ctrl Pts',(24.5,-19.2573690718243,20.6938789627184));
#53263=CARTESIAN_POINT('Ctrl Pts',(24.5,-23.4219746022546,13.4317201330038));
#53264=CARTESIAN_POINT('Ctrl Pts',(24.3078118955742,-23.4504162085652,13.4480304442642));
#53265=CARTESIAN_POINT('Ctrl Pts',(24.3078118955742,-30.5328288491125,1.09785583170779));
#53266=CARTESIAN_POINT('Ctrl Pts',(24.3078118955742,-24.355699002996,-11.7290864631587));
#53267=CARTESIAN_POINT('Ctrl Pts',(24.3078118955742,-12.6266125398373,-36.0847854661547));
#53268=CARTESIAN_POINT('Ctrl Pts',(24.3078118955742,11.7290864631587,-24.355699002996));
#53269=CARTESIAN_POINT('Ctrl Pts',(24.3078118955742,36.0847854661547,-12.6266125398373));
#53270=CARTESIAN_POINT('Ctrl Pts',(24.3078118955742,24.355699002996,11.7290864631587));
#53271=CARTESIAN_POINT('Ctrl Pts',(24.3078118955742,12.6266125398373,36.0847854661547));
#53272=CARTESIAN_POINT('Ctrl Pts',(24.3078118955742,-11.7290864631587,24.355699002996));
#53273=CARTESIAN_POINT('Ctrl Pts',(24.3078118955742,-19.2807535438433,20.7190078072539));
#53274=CARTESIAN_POINT('Ctrl Pts',(24.3078118955742,-23.4504162085652,13.4480304442642));
#53275=CARTESIAN_POINT('Ctrl Pts',(23.9225830034177,-23.5109122482986,13.4827229024644));
#53276=CARTESIAN_POINT('Ctrl Pts',(23.9225830034177,-30.6115956910654,1.10068801726159));
#53277=CARTESIAN_POINT('Ctrl Pts',(23.9225830034177,-24.4185304393985,-11.7593444881934));
#53278=CARTESIAN_POINT('Ctrl Pts',(23.9225830034177,-12.6591859512051,-36.1778749275919));
#53279=CARTESIAN_POINT('Ctrl Pts',(23.9225830034177,11.7593444881934,-24.4185304393985));
#53280=CARTESIAN_POINT('Ctrl Pts',(23.9225830034177,36.1778749275919,-12.6591859512051));
#53281=CARTESIAN_POINT('Ctrl Pts',(23.9225830034177,24.4185304393985,11.7593444881934));
#53282=CARTESIAN_POINT('Ctrl Pts',(23.9225830034177,12.6591859512051,36.1778749275919));
#53283=CARTESIAN_POINT('Ctrl Pts',(23.9225830034177,-11.7593444881934,24.4185304393985));
#53284=CARTESIAN_POINT('Ctrl Pts',(23.9225830034177,-19.330492926808,20.7724575161375));
#53285=CARTESIAN_POINT('Ctrl Pts',(23.9225830034177,-23.5109122482986,13.4827229024644));
#53286=CARTESIAN_POINT('Ctrl Pts',(23.3421815947946,-23.6124947526602,13.5409770758279));
#53287=CARTESIAN_POINT('Ctrl Pts',(23.3421815947946,-30.7438577879148,1.10544370875214));
#53288=CARTESIAN_POINT('Ctrl Pts',(23.3421815947946,-24.5240344474382,-11.8101525406477));
#53289=CARTESIAN_POINT('Ctrl Pts',(23.3421815947946,-12.7138819067904,-36.3341869880859));
#53290=CARTESIAN_POINT('Ctrl Pts',(23.3421815947946,11.8101525406477,-24.5240344474382));
#53291=CARTESIAN_POINT('Ctrl Pts',(23.3421815947946,36.3341869880859,-12.7138819067904));
#53292=CARTESIAN_POINT('Ctrl Pts',(23.3421815947946,24.5240344474382,11.8101525406477));
#53293=CARTESIAN_POINT('Ctrl Pts',(23.3421815947946,12.7138819067904,36.3341869880859));
#53294=CARTESIAN_POINT('Ctrl Pts',(23.3421815947946,-11.8101525406477,24.5240344474382));
#53295=CARTESIAN_POINT('Ctrl Pts',(23.3421815947946,-19.4140132879625,20.8622081065845));
#53296=CARTESIAN_POINT('Ctrl Pts',(23.3421815947946,-23.6124947526602,13.5409770758279));
#53297=CARTESIAN_POINT('Ctrl Pts',(22.5631762070947,-23.7697037387964,13.631131178547));
#53298=CARTESIAN_POINT('Ctrl Pts',(22.5631762070947,-30.9485464819043,1.11280361233302));
#53299=CARTESIAN_POINT('Ctrl Pts',(22.5631762070947,-24.6873123488983,-11.8887830338031));
#53300=CARTESIAN_POINT('Ctrl Pts',(22.5631762070947,-12.7985293150952,-36.5760953827013));
#53301=CARTESIAN_POINT('Ctrl Pts',(22.5631762070947,11.8887830338031,-24.6873123488983));
#53302=CARTESIAN_POINT('Ctrl Pts',(22.5631762070947,36.5760953827013,-12.7985293150952));
#53303=CARTESIAN_POINT('Ctrl Pts',(22.5631762070947,24.6873123488983,11.8887830338031));
#53304=CARTESIAN_POINT('Ctrl Pts',(22.5631762070947,12.7985293150952,36.5760953827013));
#53305=CARTESIAN_POINT('Ctrl Pts',(22.5631762070947,-11.8887830338031,24.6873123488983));
#53306=CARTESIAN_POINT('Ctrl Pts',(22.5631762070947,-19.5432693186279,21.0011060341163));
#53307=CARTESIAN_POINT('Ctrl Pts',(22.5631762070947,-23.7697037387964,13.631131178547));
#53308=CARTESIAN_POINT('Ctrl Pts',(21.5808622776984,-24.0031263055443,13.764991224189));
#53309=CARTESIAN_POINT('Ctrl Pts',(21.5808622776984,-31.2524665154187,1.12373153462988));
#53310=CARTESIAN_POINT('Ctrl Pts',(21.5808622776984,-24.929745989549,-12.0055329218856));
#53311=CARTESIAN_POINT('Ctrl Pts',(21.5808622776984,-12.9242130676634,-36.9352789114346));
#53312=CARTESIAN_POINT('Ctrl Pts',(21.5808622776984,12.0055329218856,-24.929745989549));
#53313=CARTESIAN_POINT('Ctrl Pts',(21.5808622776984,36.9352789114346,-12.9242130676634));
#53314=CARTESIAN_POINT('Ctrl Pts',(21.5808622776984,24.929745989549,12.0055329218856));
#53315=CARTESIAN_POINT('Ctrl Pts',(21.5808622776984,12.9242130676634,36.9352789114346));
#53316=CARTESIAN_POINT('Ctrl Pts',(21.5808622776984,-12.0055329218856,24.929745989549));
#53317=CARTESIAN_POINT('Ctrl Pts',(21.5808622776984,-19.73518757462,21.2073404966446));
#53318=CARTESIAN_POINT('Ctrl Pts',(21.5808622776984,-24.0031263055443,13.764991224189));
#53319=CARTESIAN_POINT('Ctrl Pts',(20.5902243197586,-24.2744594023058,13.9205916925702));
#53320=CARTESIAN_POINT('Ctrl Pts',(20.5902243197586,-31.6057466845567,1.13643427815331));
#53321=CARTESIAN_POINT('Ctrl Pts',(20.5902243197586,-25.2115536630461,-12.141244344827));
#53322=CARTESIAN_POINT('Ctrl Pts',(20.5902243197586,-13.0703093182191,-37.3527980078731));
#53323=CARTESIAN_POINT('Ctrl Pts',(20.5902243197586,12.141244344827,-25.2115536630461));
#53324=CARTESIAN_POINT('Ctrl Pts',(20.5902243197586,37.3527980078731,-13.0703093182191));
#53325=CARTESIAN_POINT('Ctrl Pts',(20.5902243197586,25.2115536630461,12.141244344827));
#53326=CARTESIAN_POINT('Ctrl Pts',(20.5902243197586,13.0703093182191,37.3527980078731));
#53327=CARTESIAN_POINT('Ctrl Pts',(20.5902243197586,-12.141244344827,25.2115536630461));
#53328=CARTESIAN_POINT('Ctrl Pts',(20.5902243197586,-19.9582755795585,21.4470698259737));
#53329=CARTESIAN_POINT('Ctrl Pts',(20.5902243197586,-24.2744594023058,13.9205916925702));
#53330=CARTESIAN_POINT('Ctrl Pts',(19.591895069338,-24.5849847342196,14.098667598778));
#53331=CARTESIAN_POINT('Ctrl Pts',(19.591895069338,-32.0100557905577,1.15097184727372));
#53332=CARTESIAN_POINT('Ctrl Pts',(19.591895069338,-25.5340665536333,-12.296558367172));
#53333=CARTESIAN_POINT('Ctrl Pts',(19.591895069338,-13.2375081864613,-37.8306249208053));
#53334=CARTESIAN_POINT('Ctrl Pts',(19.591895069338,12.296558367172,-25.5340665536333));
#53335=CARTESIAN_POINT('Ctrl Pts',(19.591895069338,37.8306249208053,-13.2375081864613));
#53336=CARTESIAN_POINT('Ctrl Pts',(19.591895069338,25.5340665536333,12.296558367172));
#53337=CARTESIAN_POINT('Ctrl Pts',(19.591895069338,13.2375081864613,37.8306249208053));
#53338=CARTESIAN_POINT('Ctrl Pts',(19.591895069338,-12.296558367172,25.5340665536333));
#53339=CARTESIAN_POINT('Ctrl Pts',(19.591895069338,-20.2135871416434,21.721426439479));
#53340=CARTESIAN_POINT('Ctrl Pts',(19.591895069338,-24.5849847342196,14.098667598778));
#53341=CARTESIAN_POINT('Ctrl Pts',(18.5871162949016,-24.9361756654508,14.3000638679505));
#53342=CARTESIAN_POINT('Ctrl Pts',(18.5871162949016,-32.4673121778761,1.16741321907992));
#53343=CARTESIAN_POINT('Ctrl Pts',(18.5871162949016,-25.8988149034099,-12.4722119146764));
#53344=CARTESIAN_POINT('Ctrl Pts',(18.5871162949016,-13.4266029887335,-38.3710268180862));
#53345=CARTESIAN_POINT('Ctrl Pts',(18.5871162949016,12.4722119146764,-25.8988149034099));
#53346=CARTESIAN_POINT('Ctrl Pts',(18.5871162949016,38.3710268180862,-13.4266029887335));
#53347=CARTESIAN_POINT('Ctrl Pts',(18.5871162949016,25.8988149034099,12.4722119146764));
#53348=CARTESIAN_POINT('Ctrl Pts',(18.5871162949016,13.4266029887335,38.3710268180862));
#53349=CARTESIAN_POINT('Ctrl Pts',(18.5871162949016,-12.4722119146764,25.8988149034099));
#53350=CARTESIAN_POINT('Ctrl Pts',(18.5871162949016,-20.502333649666,22.0317120899042));
#53351=CARTESIAN_POINT('Ctrl Pts',(18.5871162949016,-24.9361756654508,14.3000638679505));
#53352=CARTESIAN_POINT('Ctrl Pts',(17.577868433379,-25.329524499683,14.5256362864067));
#53353=CARTESIAN_POINT('Ctrl Pts',(17.577868433379,-32.9794588505319,1.1858282573341));
#53354=CARTESIAN_POINT('Ctrl Pts',(17.577868433379,-26.3073486251372,-12.6689513859872));
#53355=CARTESIAN_POINT('Ctrl Pts',(17.577868433379,-13.63839723915,-38.9763000111244));
#53356=CARTESIAN_POINT('Ctrl Pts',(17.577868433379,12.6689513859872,-26.3073486251372));
#53357=CARTESIAN_POINT('Ctrl Pts',(17.577868433379,38.9763000111244,-13.63839723915));
#53358=CARTESIAN_POINT('Ctrl Pts',(17.577868433379,26.3073486251372,12.6689513859872));
#53359=CARTESIAN_POINT('Ctrl Pts',(17.577868433379,13.63839723915,38.9763000111244));
#53360=CARTESIAN_POINT('Ctrl Pts',(17.577868433379,-12.6689513859872,26.3073486251372));
#53361=CARTESIAN_POINT('Ctrl Pts',(17.577868433379,-20.8257420643457,22.3792452635139));
#53362=CARTESIAN_POINT('Ctrl Pts',(17.577868433379,-25.329524499683,14.5256362864067));
#53363=CARTESIAN_POINT('Ctrl Pts',(16.5668667015923,-25.7662789188368,14.7761003580551));
#53364=CARTESIAN_POINT('Ctrl Pts',(16.5668667015923,-33.5481203109731,1.20627537357407));
#53365=CARTESIAN_POINT('Ctrl Pts',(16.5668667015923,-26.7609635664043,-12.8874008284133));
#53366=CARTESIAN_POINT('Ctrl Pts',(16.5668667015923,-13.873562737991,-39.6483643948176));
#53367=CARTESIAN_POINT('Ctrl Pts',(16.5668667015923,12.8874008284133,-26.7609635664043));
#53368=CARTESIAN_POINT('Ctrl Pts',(16.5668667015923,39.6483643948176,-13.873562737991));
#53369=CARTESIAN_POINT('Ctrl Pts',(16.5668667015923,26.7609635664043,12.8874008284133));
#53370=CARTESIAN_POINT('Ctrl Pts',(16.5668667015923,13.873562737991,39.6483643948176));
#53371=CARTESIAN_POINT('Ctrl Pts',(16.5668667015923,-12.8874008284133,26.7609635664043));
#53372=CARTESIAN_POINT('Ctrl Pts',(16.5668667015923,-21.1848382202515,22.7651283173505));
#53373=CARTESIAN_POINT('Ctrl Pts',(16.5668667015923,-25.7662789188368,14.7761003580551));
#53374=CARTESIAN_POINT('Ctrl Pts',(15.5576189940876,-26.2471324113782,15.0518537753682));
#53375=CARTESIAN_POINT('Ctrl Pts',(15.5576189940876,-34.1741994926254,1.22878703418975));
#53376=CARTESIAN_POINT('Ctrl Pts',(15.5576189940876,-27.2603799871926,-13.1279071008807));
#53377=CARTESIAN_POINT('Ctrl Pts',(15.5576189940876,-14.132472886312,-40.3882870880733));
#53378=CARTESIAN_POINT('Ctrl Pts',(15.5576189940876,13.1279071008807,-27.2603799871926));
#53379=CARTESIAN_POINT('Ctrl Pts',(15.5576189940876,40.3882870880733,-14.132472886312));
#53380=CARTESIAN_POINT('Ctrl Pts',(15.5576189940876,27.2603799871926,13.1279071008807));
#53381=CARTESIAN_POINT('Ctrl Pts',(15.5576189940876,14.132472886312,40.3882870880733));
#53382=CARTESIAN_POINT('Ctrl Pts',(15.5576189940876,-13.1279071008807,27.2603799871926));
#53383=CARTESIAN_POINT('Ctrl Pts',(15.5576189940876,-21.580192298317,23.1899739651847));
#53384=CARTESIAN_POINT('Ctrl Pts',(15.5576189940876,-26.2471324113782,15.0518537753682));
#53385=CARTESIAN_POINT('Ctrl Pts',(14.5544447688713,-26.7719304659624,15.3528079312506));
#53386=CARTESIAN_POINT('Ctrl Pts',(14.5544447688713,-34.8574952191684,1.25335600557047));
#53387=CARTESIAN_POINT('Ctrl Pts',(14.5544447688713,-27.805437411382,-13.3903929221629));
#53388=CARTESIAN_POINT('Ctrl Pts',(14.5544447688713,-14.4150444892191,-41.1958303335449));
#53389=CARTESIAN_POINT('Ctrl Pts',(14.5544447688713,13.3903929221629,-27.805437411382));
#53390=CARTESIAN_POINT('Ctrl Pts',(14.5544447688713,41.1958303335449,-14.4150444892191));
#53391=CARTESIAN_POINT('Ctrl Pts',(14.5544447688713,27.805437411382,13.3903929221629));
#53392=CARTESIAN_POINT('Ctrl Pts',(14.5544447688713,14.4150444892191,41.1958303335449));
#53393=CARTESIAN_POINT('Ctrl Pts',(14.5544447688713,-13.3903929221629,27.805437411382));
#53394=CARTESIAN_POINT('Ctrl Pts',(14.5544447688713,-22.0116772604913,23.6536456925202));
#53395=CARTESIAN_POINT('Ctrl Pts',(14.5544447688713,-26.7719304659624,15.3528079312506));
#53396=CARTESIAN_POINT('Ctrl Pts',(13.5625963827217,-27.3391811060136,15.6781072269685));
#53397=CARTESIAN_POINT('Ctrl Pts',(13.5625963827217,-35.596064912482,1.27991243926791));
#53398=CARTESIAN_POINT('Ctrl Pts',(13.5625963827217,-28.3945862659469,-13.6741120572209));
#53399=CARTESIAN_POINT('Ctrl Pts',(13.5625963827217,-14.720474208726,-42.0686983231678));
#53400=CARTESIAN_POINT('Ctrl Pts',(13.5625963827217,13.6741120572209,-28.3945862659469));
#53401=CARTESIAN_POINT('Ctrl Pts',(13.5625963827217,42.0686983231678,-14.720474208726));
#53402=CARTESIAN_POINT('Ctrl Pts',(13.5625963827217,28.3945862659469,13.6741120572209));
#53403=CARTESIAN_POINT('Ctrl Pts',(13.5625963827217,14.720474208726,42.0686983231678));
#53404=CARTESIAN_POINT('Ctrl Pts',(13.5625963827217,-13.6741120572209,28.3945862659469));
#53405=CARTESIAN_POINT('Ctrl Pts',(13.5625963827217,-22.4780664150012,24.1548253021));
#53406=CARTESIAN_POINT('Ctrl Pts',(13.5625963827217,-27.3391811060136,15.6781072269685));
#53407=CARTESIAN_POINT('Ctrl Pts',(12.5880795783847,-27.9460475476476,16.0261248617137));
#53408=CARTESIAN_POINT('Ctrl Pts',(12.5880795783847,-36.3862150331401,1.30832352826907));
#53409=CARTESIAN_POINT('Ctrl Pts',(12.5880795783847,-29.0248802554437,-13.9776456449495));
#53410=CARTESIAN_POINT('Ctrl Pts',(12.5880795783847,-15.0472346104942,-43.0025259003932));
#53411=CARTESIAN_POINT('Ctrl Pts',(12.5880795783847,13.9776456449495,-29.0248802554437));
#53412=CARTESIAN_POINT('Ctrl Pts',(12.5880795783847,43.0025259003932,-15.0472346104942));
#53413=CARTESIAN_POINT('Ctrl Pts',(12.5880795783847,29.0248802554437,13.9776456449495));
#53414=CARTESIAN_POINT('Ctrl Pts',(12.5880795783847,15.0472346104942,43.0025259003932));
#53415=CARTESIAN_POINT('Ctrl Pts',(12.5880795783847,-13.9776456449495,29.0248802554437));
#53416=CARTESIAN_POINT('Ctrl Pts',(12.5880795783847,-22.9770273797494,24.691006427004));
#53417=CARTESIAN_POINT('Ctrl Pts',(12.5880795783847,-27.9460475476476,16.0261248617137));
#53418=CARTESIAN_POINT('Ctrl Pts',(11.6370973936883,-28.5889671307382,16.394817768898));
#53419=CARTESIAN_POINT('Ctrl Pts',(11.6370973936883,-37.2233069388725,1.33842248290329));
#53420=CARTESIAN_POINT('Ctrl Pts',(11.6370973936883,-29.6926191863701,-14.2992117660733));
#53421=CARTESIAN_POINT('Ctrl Pts',(11.6370973936883,-15.3934074202968,-43.9918309524434));
#53422=CARTESIAN_POINT('Ctrl Pts',(11.6370973936883,14.2992117660733,-29.6926191863701));
#53423=CARTESIAN_POINT('Ctrl Pts',(11.6370973936883,43.9918309524434,-15.3934074202968));
#53424=CARTESIAN_POINT('Ctrl Pts',(11.6370973936883,29.6926191863701,14.2992117660733));
#53425=CARTESIAN_POINT('Ctrl Pts',(11.6370973936883,15.3934074202968,43.9918309524434));
#53426=CARTESIAN_POINT('Ctrl Pts',(11.6370973936883,-14.2992117660733,29.6926191863701));
#53427=CARTESIAN_POINT('Ctrl Pts',(11.6370973936883,-23.5056309627235,25.259041371161));
#53428=CARTESIAN_POINT('Ctrl Pts',(11.6370973936883,-28.5889671307382,16.394817768898));
#53429=CARTESIAN_POINT('Ctrl Pts',(10.7155646400367,-29.2640651345263,16.7819639255827));
#53430=CARTESIAN_POINT('Ctrl Pts',(10.7155646400367,-38.1022956793159,1.37002790405408));
#53431=CARTESIAN_POINT('Ctrl Pts',(10.7155646400367,-30.3937787577631,-14.6368724193901));
#53432=CARTESIAN_POINT('Ctrl Pts',(10.7155646400367,-15.756906338373,-45.0306511771533));
#53433=CARTESIAN_POINT('Ctrl Pts',(10.7155646400367,14.6368724193901,-30.3937787577631));
#53434=CARTESIAN_POINT('Ctrl Pts',(10.7155646400367,45.0306511771533,-15.756906338373));
#53435=CARTESIAN_POINT('Ctrl Pts',(10.7155646400367,30.3937787577631,14.6368724193901));
#53436=CARTESIAN_POINT('Ctrl Pts',(10.7155646400367,15.756906338373,45.0306511771533));
#53437=CARTESIAN_POINT('Ctrl Pts',(10.7155646400367,-14.6368724193901,30.3937787577631));
#53438=CARTESIAN_POINT('Ctrl Pts',(10.7155646400367,-24.0606913980357,25.8555067254108));
#53439=CARTESIAN_POINT('Ctrl Pts',(10.7155646400367,-29.2640651345263,16.7819639255827));
#53440=CARTESIAN_POINT('Ctrl Pts',(9.82859575068344,-29.9675923231116,17.1854132702049));
#53441=CARTESIAN_POINT('Ctrl Pts',(9.82859575068344,-39.0182996874633,1.40296426731023));
#53442=CARTESIAN_POINT('Ctrl Pts',(9.82859575068344,-31.1244649977519,-14.9887523668806));
#53443=CARTESIAN_POINT('Ctrl Pts',(9.82859575068344,-16.1357126308712,-46.1132173646325));
#53444=CARTESIAN_POINT('Ctrl Pts',(9.82859575068344,14.9887523668806,-31.1244649977519));
#53445=CARTESIAN_POINT('Ctrl Pts',(9.82859575068344,46.1132173646325,-16.1357126308712));
#53446=CARTESIAN_POINT('Ctrl Pts',(9.82859575068344,31.1244649977519,14.9887523668806));
#53447=CARTESIAN_POINT('Ctrl Pts',(9.82859575068344,16.1357126308712,46.1132173646325));
#53448=CARTESIAN_POINT('Ctrl Pts',(9.82859575068344,-14.9887523668806,31.1244649977519));
#53449=CARTESIAN_POINT('Ctrl Pts',(9.82859575068344,-24.6391260924933,26.4770899494897));
#53450=CARTESIAN_POINT('Ctrl Pts',(9.82859575068344,-29.9675923231116,17.1854132702049));
#53451=CARTESIAN_POINT('Ctrl Pts',(8.97989469943246,-30.6963420508599,17.6033268985962));
#53452=CARTESIAN_POINT('Ctrl Pts',(8.97989469943246,-39.9671438577877,1.43708145019297));
#53453=CARTESIAN_POINT('Ctrl Pts',(8.97989469943246,-31.8813474709538,-15.3532477553949));
#53454=CARTESIAN_POINT('Ctrl Pts',(8.97989469943246,-16.5280997155589,-47.2345952263487));
#53455=CARTESIAN_POINT('Ctrl Pts',(8.97989469943246,15.3532477553949,-31.8813474709538));
#53456=CARTESIAN_POINT('Ctrl Pts',(8.97989469943246,47.2345952263487,-16.5280997155589));
#53457=CARTESIAN_POINT('Ctrl Pts',(8.97989469943246,31.8813474709538,15.3532477553949));
#53458=CARTESIAN_POINT('Ctrl Pts',(8.97989469943246,16.5280997155589,47.2345952263487));
#53459=CARTESIAN_POINT('Ctrl Pts',(8.97989469943246,-15.3532477553949,31.8813474709538));
#53460=CARTESIAN_POINT('Ctrl Pts',(8.97989469943246,-25.2382985664866,27.1209578947093));
#53461=CARTESIAN_POINT('Ctrl Pts',(8.97989469943246,-30.6963420508599,17.6033268985962));
#53462=CARTESIAN_POINT('Ctrl Pts',(8.1713316609345,-31.4479687613503,18.0343597124917));
#53463=CARTESIAN_POINT('Ctrl Pts',(8.1713316609345,-40.9457742371258,1.47226964301821));
#53464=CARTESIAN_POINT('Ctrl Pts',(8.1713316609345,-32.6619900727951,-15.7291854188016));
#53465=CARTESIAN_POINT('Ctrl Pts',(8.1713316609345,-16.9328046539935,-48.3911754915967));
#53466=CARTESIAN_POINT('Ctrl Pts',(8.1713316609345,15.7291854188016,-32.6619900727951));
#53467=CARTESIAN_POINT('Ctrl Pts',(8.1713316609345,48.3911754915967,-16.9328046539935));
#53468=CARTESIAN_POINT('Ctrl Pts',(8.1713316609345,32.6619900727951,15.7291854188016));
#53469=CARTESIAN_POINT('Ctrl Pts',(8.1713316609345,16.9328046539935,48.3911754915967));
#53470=CARTESIAN_POINT('Ctrl Pts',(8.1713316609345,-15.7291854188016,32.6619900727951));
#53471=CARTESIAN_POINT('Ctrl Pts',(8.1713316609345,-25.8562803213964,27.7850382054503));
#53472=CARTESIAN_POINT('Ctrl Pts',(8.1713316609345,-31.4479687613503,18.0343597124917));
#53473=CARTESIAN_POINT('Ctrl Pts',(7.40358438374929,-32.2208437341878,18.4775776951444));
#53474=CARTESIAN_POINT('Ctrl Pts',(7.40358438374929,-41.9520702046485,1.50845259553232));
#53475=CARTESIAN_POINT('Ctrl Pts',(7.40358438374929,-33.4647012075554,-16.1157507275363));
#53476=CARTESIAN_POINT('Ctrl Pts',(7.40358438374929,-17.3489504800191,-49.5804519350917));
#53477=CARTESIAN_POINT('Ctrl Pts',(7.40358438374929,16.1157507275363,-33.4647012075554));
#53478=CARTESIAN_POINT('Ctrl Pts',(7.40358438374929,49.5804519350917,-17.3489504800191));
#53479=CARTESIAN_POINT('Ctrl Pts',(7.40358438374929,33.4647012075554,16.1157507275363));
#53480=CARTESIAN_POINT('Ctrl Pts',(7.40358438374929,17.3489504800191,49.5804519350917));
#53481=CARTESIAN_POINT('Ctrl Pts',(7.40358438374929,-16.1157507275363,33.4647012075554));
#53482=CARTESIAN_POINT('Ctrl Pts',(7.40358438374929,-26.4917322357228,28.4678918679965));
#53483=CARTESIAN_POINT('Ctrl Pts',(7.40358438374929,-32.2208437341878,18.4775776951444));
#53484=CARTESIAN_POINT('Ctrl Pts',(6.82198164612729,-32.8553406354367,18.8414404756127));
#53485=CARTESIAN_POINT('Ctrl Pts',(6.82198164612729,-42.778195639644,1.53815723348166));
#53486=CARTESIAN_POINT('Ctrl Pts',(6.82198164612729,-34.1236923063789,-16.4331041147498));
#53487=CARTESIAN_POINT('Ctrl Pts',(6.82198164612729,-17.6905881916291,-50.5567964211288));
#53488=CARTESIAN_POINT('Ctrl Pts',(6.82198164612729,16.4331041147498,-34.1236923063789));
#53489=CARTESIAN_POINT('Ctrl Pts',(6.82198164612729,50.5567964211288,-17.6905881916291));
#53490=CARTESIAN_POINT('Ctrl Pts',(6.82198164612729,34.1236923063789,16.4331041147498));
#53491=CARTESIAN_POINT('Ctrl Pts',(6.82198164612729,17.6905881916291,50.5567964211288));
#53492=CARTESIAN_POINT('Ctrl Pts',(6.82198164612729,-16.4331041147498,34.1236923063789));
#53493=CARTESIAN_POINT('Ctrl Pts',(6.82198164612729,-27.013410753857,29.0284851697842));
#53494=CARTESIAN_POINT('Ctrl Pts',(6.82198164612729,-32.8553406354367,18.8414404756127));
#53495=CARTESIAN_POINT('Ctrl Pts',(6.40395249919757,-33.3400992359811,19.1194333419337));
#53496=CARTESIAN_POINT('Ctrl Pts',(6.40395249919757,-43.4093593363527,1.56085171582452));
#53497=CARTESIAN_POINT('Ctrl Pts',(6.40395249919757,-34.627164588447,-16.6755635870669));
#53498=CARTESIAN_POINT('Ctrl Pts',(6.40395249919757,-17.9516010013801,-51.3027281755139));
#53499=CARTESIAN_POINT('Ctrl Pts',(6.40395249919757,16.6755635870669,-34.627164588447));
#53500=CARTESIAN_POINT('Ctrl Pts',(6.40395249919757,51.3027281755139,-17.9516010013801));
#53501=CARTESIAN_POINT('Ctrl Pts',(6.40395249919757,34.627164588447,16.6755635870669));
#53502=CARTESIAN_POINT('Ctrl Pts',(6.40395249919757,17.9516010013801,51.3027281755139));
#53503=CARTESIAN_POINT('Ctrl Pts',(6.40395249919757,-16.6755635870669,34.627164588447));
#53504=CARTESIAN_POINT('Ctrl Pts',(6.40395249919757,-27.4119755819704,29.4567810746408));
#53505=CARTESIAN_POINT('Ctrl Pts',(6.40395249919757,-33.3400992359811,19.1194333419337));
#53506=CARTESIAN_POINT('Ctrl Pts',(6.13331019225912,-33.6672049264476,19.3070175299823));
#53507=CARTESIAN_POINT('Ctrl Pts',(6.13331019225912,-43.835256342775,1.57616551182155));
#53508=CARTESIAN_POINT('Ctrl Pts',(6.13331019225912,-34.9668979078181,-16.8391705308393));
#53509=CARTESIAN_POINT('Ctrl Pts',(6.13331019225912,-18.1277273769788,-51.8060684386574));
#53510=CARTESIAN_POINT('Ctrl Pts',(6.13331019225912,16.8391705308393,-34.9668979078181));
#53511=CARTESIAN_POINT('Ctrl Pts',(6.13331019225912,51.8060684386574,-18.1277273769788));
#53512=CARTESIAN_POINT('Ctrl Pts',(6.13331019225912,34.9668979078181,16.8391705308393));
#53513=CARTESIAN_POINT('Ctrl Pts',(6.13331019225912,18.1277273769788,51.8060684386574));
#53514=CARTESIAN_POINT('Ctrl Pts',(6.13331019225912,-16.8391705308393,34.9668979078181));
#53515=CARTESIAN_POINT('Ctrl Pts',(6.13331019225912,-27.6809193885357,29.745786834466));
#53516=CARTESIAN_POINT('Ctrl Pts',(6.13331019225912,-33.6672049264476,19.3070175299823));
#53517=CARTESIAN_POINT('Ctrl Pts',(6.,-33.8317410921456,19.4013735254499));
#53518=CARTESIAN_POINT('Ctrl Pts',(6.,-44.0494851454566,1.58386844499903));
#53519=CARTESIAN_POINT('Ctrl Pts',(6.,-35.1377858481943,-16.9214658255848));
#53520=CARTESIAN_POINT('Ctrl Pts',(6.,-18.2163200226096,-52.0592516737791));
#53521=CARTESIAN_POINT('Ctrl Pts',(6.,16.9214658255848,-35.1377858481943));
#53522=CARTESIAN_POINT('Ctrl Pts',(6.,52.0592516737791,-18.2163200226096));
#53523=CARTESIAN_POINT('Ctrl Pts',(6.,35.1377858481943,16.9214658255848));
#53524=CARTESIAN_POINT('Ctrl Pts',(6.,18.2163200226096,52.0592516737791));
#53525=CARTESIAN_POINT('Ctrl Pts',(6.,-16.9214658255848,35.1377858481943));
#53526=CARTESIAN_POINT('Ctrl Pts',(6.,-27.8161997704128,29.8911585017043));
#53527=CARTESIAN_POINT('Ctrl Pts',(6.,-33.8317410921456,19.4013735254499));
#53528=CARTESIAN_POINT('Ctrl Pts',(24.5,-23.4219747427337,13.431719888039));
#53529=CARTESIAN_POINT('Ctrl Pts',(23.5178991898112,-25.0276360494611,10.9685861831122));
#53530=CARTESIAN_POINT('Ctrl Pts',(22.3947886245986,-26.2729301477538,8.34676959442289));
#53531=CARTESIAN_POINT('Ctrl Pts',(21.1743874927566,-27.2201735658818,5.66613862859487));
#53532=CARTESIAN_POINT('Ctrl Pts',(20.5031871793434,-27.7411416824604,4.19183620665813));
#53533=CARTESIAN_POINT('Ctrl Pts',(19.8411792966408,-28.1598441640515,2.68270023879079));
#53534=CARTESIAN_POINT('Ctrl Pts',(19.1295827650261,-28.508103594306,1.18344085144545));
#53535=CARTESIAN_POINT('Ctrl Pts',(18.8261415870913,-28.6566094498694,0.544122060088292));
#53536=CARTESIAN_POINT('Ctrl Pts',(18.5104994276271,-28.7937513256439,-0.0985692732500806));
#53537=CARTESIAN_POINT('Ctrl Pts',(18.2016639423759,-28.9165522468366,-0.697094034628921));
#53538=CARTESIAN_POINT('Ctrl Pts',(17.6747132403633,-29.1260813803741,-1.718327209709));
#53539=CARTESIAN_POINT('Ctrl Pts',(17.2016343370993,-29.2779074067587,-2.63744809926651));
#53540=CARTESIAN_POINT('Ctrl Pts',(16.872935292646,-29.3776496099841,-3.25480188360693));
#53541=CARTESIAN_POINT('Ctrl Pts',(16.6342454025477,-29.4500789520458,-3.703102873289));
#53542=CARTESIAN_POINT('Ctrl Pts',(16.5014949770664,-29.4875609766571,-3.94561707113168));
#53543=CARTESIAN_POINT('Ctrl Pts',(16.3424569562979,-29.5324155816376,-4.23265760880312));
#53544=CARTESIAN_POINT('Ctrl Pts',(15.993118510103,-29.6309419461689,-4.86316278574444));
#53545=CARTESIAN_POINT('Ctrl Pts',(15.6312480487537,-29.7273563920893,-5.48745018218933));
#53546=CARTESIAN_POINT('Ctrl Pts',(15.2503296894305,-29.8330034119802,-6.09818239131044));
#53547=CARTESIAN_POINT('Ctrl Pts',(14.7484414179076,-29.9722012188248,-6.90286750374191));
#53548=CARTESIAN_POINT('Ctrl Pts',(14.2669345517206,-30.0952138942946,-7.68104629603547));
#53549=CARTESIAN_POINT('Ctrl Pts',(13.7912435751455,-30.2282988102454,-8.40145711329548));
#53550=CARTESIAN_POINT('Ctrl Pts',(13.5533980868579,-30.2948412682208,-8.76166252192548));
#53551=CARTESIAN_POINT('Ctrl Pts',(13.3161115657262,-30.3641806660347,-9.10948527341258));
#53552=CARTESIAN_POINT('Ctrl Pts',(13.0766514227367,-30.440228178246,-9.44459923238964));
#53553=CARTESIAN_POINT('Ctrl Pts',(12.9188702359555,-30.4903361694075,-9.66540707746248));
#53554=CARTESIAN_POINT('Ctrl Pts',(12.7601526360409,-30.5433595566134,-9.88070391694664));
#53555=CARTESIAN_POINT('Ctrl Pts',(12.5997389313808,-30.6005375280091,-10.0903988646281));
#53556=CARTESIAN_POINT('Ctrl Pts',(12.5166971934814,-30.6301369822723,-10.1989521389328));
#53557=CARTESIAN_POINT('Ctrl Pts',(12.4397215765388,-30.6583559714772,-10.29784186772));
#53558=CARTESIAN_POINT('Ctrl Pts',(12.3478597934844,-30.6933593253107,-10.4131461873135));
#53559=CARTESIAN_POINT('Ctrl Pts',(11.9116121727781,-30.8595887334372,-10.9607213965826));
#53560=CARTESIAN_POINT('Ctrl Pts',(10.7144663992386,-31.2847896561702,-12.5314661716072));
#53561=CARTESIAN_POINT('Ctrl Pts',(9.56604185022482,-32.0598213250961,-13.5737242681804));
#53562=CARTESIAN_POINT('Ctrl Pts',(9.07284645450724,-32.3926616940849,-14.0213260673763));
#53563=CARTESIAN_POINT('Ctrl Pts',(8.57333454992668,-32.7892957869518,-14.4000170895921));
#53564=CARTESIAN_POINT('Ctrl Pts',(8.00348148262884,-33.3155434735552,-14.8086408410792));
#53565=CARTESIAN_POINT('Ctrl Pts',(7.63919428965855,-33.6519552673337,-15.0698597551337));
#53566=CARTESIAN_POINT('Ctrl Pts',(7.24388644384666,-34.0525400988056,-15.3432535750814));
#53567=CARTESIAN_POINT('Ctrl Pts',(6.94254646282606,-34.3778179503946,-15.5540684672922));
#53568=CARTESIAN_POINT('Ctrl Pts',(6.91433564865313,-34.4082697775789,-15.5738045133651));
#53569=CARTESIAN_POINT('Ctrl Pts',(6.88669635040576,-34.4382827302419,-15.5931590893644));
#53570=CARTESIAN_POINT('Ctrl Pts',(6.85962514029878,-34.4678401502989,-15.6121377164754));
#53571=CARTESIAN_POINT('Ctrl Pts',(6.44000062073739,-34.9260028309428,-15.9063209928014));
#53572=CARTESIAN_POINT('Ctrl Pts',(6.15412442492902,-35.2918397798349,-16.0757548327879));
#53573=CARTESIAN_POINT('Ctrl Pts',(6.,-35.4893251315053,-16.1712028529206));
#53574=CARTESIAN_POINT('Ctrl Pts',(2.09999999999999,-9.13041565192885,-3.39805179937466));
#53575=CARTESIAN_POINT('Ctrl Pts',(2.73333333333332,-9.13041565192885,-3.39805179937466));
#53576=CARTESIAN_POINT('Ctrl Pts',(3.36701317451252,-9.13040108347824,-3.39810652799444));
#53577=CARTESIAN_POINT('Ctrl Pts',(4.12582101723434,-9.13039676871029,-3.39812307912054));
#53578=CARTESIAN_POINT('Ctrl Pts',(4.3827813081152,-9.12995863034688,-3.39933937508568));
#53579=CARTESIAN_POINT('Ctrl Pts',(4.88874880886513,-9.12802340460705,-3.40473249825757));
#53580=CARTESIAN_POINT('Ctrl Pts',(5.76579688899393,-9.12357463561424,-3.4171742341258));
#53581=CARTESIAN_POINT('Ctrl Pts',(6.49301772180469,-9.12367746676099,-3.41699407326797));
#53582=CARTESIAN_POINT('Ctrl Pts',(7.02339624162716,-9.13084124181946,-3.39664052379125));
#53583=CARTESIAN_POINT('Ctrl Pts',(7.1498562830745,-9.13266683983108,-3.3916514191029));
#53584=CARTESIAN_POINT('Ctrl Pts',(7.33704059907056,-9.13564437529334,-3.38374208606773));
#53585=CARTESIAN_POINT('Ctrl Pts',(7.52531480017061,-9.13893394226214,-3.37518464965992));
#53586=CARTESIAN_POINT('Ctrl Pts',(7.90079264373577,-9.14610157643292,-3.35670170902175));
#53587=CARTESIAN_POINT('Ctrl Pts',(8.46123456943149,-9.15912772542386,-3.32321177104627));
#53588=CARTESIAN_POINT('Ctrl Pts',(9.06500753118942,-9.177875904121,-3.27146172501592));
#53589=CARTESIAN_POINT('Ctrl Pts',(9.52838216794511,-9.19546305542652,-3.21908622722073));
#53590=CARTESIAN_POINT('Ctrl Pts',(9.75197533530386,-9.20509907063539,-3.18893300462712));
#53591=CARTESIAN_POINT('Ctrl Pts',(10.3692809660311,-9.23340523376178,-3.09795413997167));
#53592=CARTESIAN_POINT('Ctrl Pts',(11.3477650727983,-9.30172686747984,-2.89373436722122));
#53593=CARTESIAN_POINT('Ctrl Pts',(12.2736167934301,-9.38175751450599,-2.62467429855293));
#53594=CARTESIAN_POINT('Ctrl Pts',(13.0004869538322,-9.43659420895444,-2.40131121191103));
#53595=CARTESIAN_POINT('Ctrl Pts',(13.5002202963651,-9.47692561134844,-2.23041445466345));
#53596=CARTESIAN_POINT('Ctrl Pts',(14.4706182485369,-9.56220626799283,-1.84447625067277));
#53597=CARTESIAN_POINT('Ctrl Pts',(15.1515663737436,-9.61926188953974,-1.52559606535566));
#53598=CARTESIAN_POINT('Ctrl Pts',(15.884389511088,-9.66262454675229,-1.17518401443769));
#53599=CARTESIAN_POINT('Ctrl Pts',(16.3868780638063,-9.68960774126478,-0.916464713226361));
#53600=CARTESIAN_POINT('Ctrl Pts',(17.3638496496076,-9.73087588269211,-0.357244332963071));
#53601=CARTESIAN_POINT('Ctrl Pts',(18.0499776434112,-9.73673515107644,0.0836392175228933));
#53602=CARTESIAN_POINT('Ctrl Pts',(18.7841567244697,-9.71419302093459,0.55803484097089));
#53603=CARTESIAN_POINT('Ctrl Pts',(19.2877100748509,-9.68849014881372,0.901898771721124));
#53604=CARTESIAN_POINT('Ctrl Pts',(20.2708126431919,-9.60110184256547,1.62625821337173));
#53605=CARTESIAN_POINT('Ctrl Pts',(20.968566991788,-9.48879837203063,2.17915797653068));
#53606=CARTESIAN_POINT('Ctrl Pts',(22.6570657765617,-9.12376585269189,3.49147880528747));
#53607=CARTESIAN_POINT('Ctrl Pts',(23.7241254823866,-8.71518052183065,4.38549881588758));
#53608=CARTESIAN_POINT('Ctrl Pts',(24.6950729185821,-8.16338858110383,5.27047024423429));
#53609=CARTESIAN_POINT('Ctrl Pts',(2.09999999999999,-12.9002177548493,-5.21349281006839));
#53610=CARTESIAN_POINT('Ctrl Pts',(2.73333333333332,-12.9002177548493,-5.21349281006839));
#53611=CARTESIAN_POINT('Ctrl Pts',(3.36720848131827,-12.9001975910235,-5.21355448519127));
#53612=CARTESIAN_POINT('Ctrl Pts',(4.12623507204341,-12.9001917132969,-5.21357280295523));
#53613=CARTESIAN_POINT('Ctrl Pts',(4.38604826009982,-12.8995138670331,-5.21530251739604));
#53614=CARTESIAN_POINT('Ctrl Pts',(4.89390545898918,-12.8965300720384,-5.2229435076951));
#53615=CARTESIAN_POINT('Ctrl Pts',(5.77024592040542,-12.8896918237525,-5.24051394682823));
#53616=CARTESIAN_POINT('Ctrl Pts',(6.48768609145402,-12.8898924702624,-5.24012227121644));
#53617=CARTESIAN_POINT('Ctrl Pts',(7.00642437533162,-12.900756463832,-5.21179807239735));
#53618=CARTESIAN_POINT('Ctrl Pts',(7.13273638677672,-12.9035579301272,-5.20475518479158));
#53619=CARTESIAN_POINT('Ctrl Pts',(7.3183164241747,-12.9080992926691,-5.19364592987697));
#53620=CARTESIAN_POINT('Ctrl Pts',(7.50524686034319,-12.9131151672861,-5.18161674063603));
#53621=CARTESIAN_POINT('Ctrl Pts',(7.87735507332389,-12.9240283057097,-5.15566801581097));
#53622=CARTESIAN_POINT('Ctrl Pts',(8.4315346972579,-12.9438386062717,-5.10870296150625));
#53623=CARTESIAN_POINT('Ctrl Pts',(9.02545493458829,-12.9723788727574,-5.03636407240455));
#53624=CARTESIAN_POINT('Ctrl Pts',(9.47896581078012,-12.99918743678,-4.96340069318231));
#53625=CARTESIAN_POINT('Ctrl Pts',(9.69688367867189,-13.0138864528649,-4.92150249520299));
#53626=CARTESIAN_POINT('Ctrl Pts',(10.2969185301416,-13.0570771398965,-4.79527718202436));
#53627=CARTESIAN_POINT('Ctrl Pts',(11.2522144952412,-13.1613303391514,-4.51147447372354));
#53628=CARTESIAN_POINT('Ctrl Pts',(12.16830830149,-13.2859456545432,-4.13360457116113));
#53629=CARTESIAN_POINT('Ctrl Pts',(12.8911660496029,-13.3731353575996,-3.81822327297548));
#53630=CARTESIAN_POINT('Ctrl Pts',(13.3786040775802,-13.4368505094726,-3.58035741471442));
#53631=CARTESIAN_POINT('Ctrl Pts',(14.3384175365999,-13.574070267889,-3.03828527802715));
#53632=CARTESIAN_POINT('Ctrl Pts',(15.0146631063079,-13.6690362785393,-2.58739886270306));
#53633=CARTESIAN_POINT('Ctrl Pts',(15.7460539088381,-13.7458705357116,-2.0894399940261));
#53634=CARTESIAN_POINT('Ctrl Pts',(16.2427389372309,-13.7954928643336,-1.7249477173051));
#53635=CARTESIAN_POINT('Ctrl Pts',(17.2171500502893,-13.8792388914454,-0.931039998810538));
#53636=CARTESIAN_POINT('Ctrl Pts',(17.901657841902,-13.9071495118269,-0.302213557964748));
#53637=CARTESIAN_POINT('Ctrl Pts',(18.6350521995774,-13.89566421944,0.376020800248144));
#53638=CARTESIAN_POINT('Ctrl Pts',(19.138387973248,-13.8747909549584,0.867348303200731));
#53639=CARTESIAN_POINT('Ctrl Pts',(20.1238445925502,-13.782576518031,1.90675272254023));
#53640=CARTESIAN_POINT('Ctrl Pts',(20.822005894914,-13.6464379916399,2.70212764346435));
#53641=CARTESIAN_POINT('Ctrl Pts',(22.5097447039609,-13.1821252157743,4.59209198679041));
#53642=CARTESIAN_POINT('Ctrl Pts',(23.5814142719248,-12.6388162011058,5.8901716529331));
#53643=CARTESIAN_POINT('Ctrl Pts',(24.5630597774301,-11.882904360092,7.18919796098686));
#53644=CARTESIAN_POINT('Ctrl Pts',(2.09999999999999,-21.6964226616636,-9.44952183502042));
#53645=CARTESIAN_POINT('Ctrl Pts',(2.73333333333332,-21.6964226616636,-9.44952183502042));
#53646=CARTESIAN_POINT('Ctrl Pts',(3.36768851389112,-21.6963695414677,-9.44970316559896));
#53647=CARTESIAN_POINT('Ctrl Pts',(4.12723220823948,-21.6963540844379,-9.44975722375134));
#53648=CARTESIAN_POINT('Ctrl Pts',(4.39370635937899,-21.6950981950085,-9.45272881112924));
#53649=CARTESIAN_POINT('Ctrl Pts',(4.90596400000984,-21.6896305544311,-9.46570382276018));
#53650=CARTESIAN_POINT('Ctrl Pts',(5.78069669373953,-21.6772192778768,-9.49525285207215));
#53651=CARTESIAN_POINT('Ctrl Pts',(6.47525361359603,-21.677778366334,-9.49418418263408));
#53652=CARTESIAN_POINT('Ctrl Pts',(6.96710249362278,-21.6966497719658,-9.44860121784704));
#53653=CARTESIAN_POINT('Ctrl Pts',(7.09307430585892,-21.7017191773118,-9.43678759087601));
#53654=CARTESIAN_POINT('Ctrl Pts',(7.27495509380485,-21.7098167389422,-9.4184111745766));
#53655=CARTESIAN_POINT('Ctrl Pts',(7.45879739148957,-21.7187736697537,-9.39847144082777));
#53656=CARTESIAN_POINT('Ctrl Pts',(7.823170843205,-21.7381987850423,-9.35559078117172));
#53657=CARTESIAN_POINT('Ctrl Pts',(8.36310684327955,-21.7733135823236,-9.27838002203018));
#53658=CARTESIAN_POINT('Ctrl Pts',(8.93508744882405,-21.823600521285,-9.16047238005773));
#53659=CARTESIAN_POINT('Ctrl Pts',(9.36757815131443,-21.87052047451,-9.04266937137984));
#53660=CARTESIAN_POINT('Ctrl Pts',(9.57392762477484,-21.8961119122116,-8.97550203198768));
#53661=CARTESIAN_POINT('Ctrl Pts',(10.140021954483,-21.9710011903251,-8.77426004522114));
#53662=CARTESIAN_POINT('Ctrl Pts',(11.0614193925012,-22.1545360362948,-8.31703872507497));
#53663=CARTESIAN_POINT('Ctrl Pts',(11.9722628052669,-22.3833575412528,-7.68838929295787));
#53664=CARTESIAN_POINT('Ctrl Pts',(12.6924971605734,-22.5463694958218,-7.16015059826062));
#53665=CARTESIAN_POINT('Ctrl Pts',(13.1758960402558,-22.6651639298491,-6.76712693131451));
#53666=CARTESIAN_POINT('Ctrl Pts',(14.142076411012,-22.9274558453913,-5.85324663451816));
#53667=CARTESIAN_POINT('Ctrl Pts',(14.8238713096107,-23.1131579009961,-5.08951620479052));
#53668=CARTESIAN_POINT('Ctrl Pts',(15.5572563628566,-23.269163089777,-4.24668378099617));
#53669=CARTESIAN_POINT('Ctrl Pts',(16.0655853887807,-23.3748818615298,-3.62213679367982));
#53670=CARTESIAN_POINT('Ctrl Pts',(17.0554277769773,-23.5604115991072,-2.2604717975477));
#53671=CARTESIAN_POINT('Ctrl Pts',(17.749227444809,-23.639780747396,-1.18295910400568));
#53672=CARTESIAN_POINT('Ctrl Pts',(18.4856283652679,-23.6530822724334,-0.0267264997289242));
#53673=CARTESIAN_POINT('Ctrl Pts',(19.0039954021354,-23.642532945262,0.828874446381748));
#53674=CARTESIAN_POINT('Ctrl Pts',(20.0037042032201,-23.5329875501118,2.62392419000413));
#53675=CARTESIAN_POINT('Ctrl Pts',(20.7092095322358,-23.3355002606907,3.994145223667));
#53676=CARTESIAN_POINT('Ctrl Pts',(22.4031068849489,-22.6280521158487,7.2370377336757));
#53677=CARTESIAN_POINT('Ctrl Pts',(23.504475912352,-21.746935009538,9.5200949784719));
#53678=CARTESIAN_POINT('Ctrl Pts',(24.5018373925611,-20.4887878955378,11.7966817146722));
#53679=CARTESIAN_POINT('Ctrl Pts',(2.09999999999999,-30.492627568478,-13.6855508599725));
#53680=CARTESIAN_POINT('Ctrl Pts',(2.73333333333332,-30.492627568478,-13.6855508599725));
#53681=CARTESIAN_POINT('Ctrl Pts',(3.36822682214226,-30.4925870569924,-13.6857046438341));
#53682=CARTESIAN_POINT('Ctrl Pts',(4.12830119635636,-30.4925765273047,-13.6857478663648));
#53683=CARTESIAN_POINT('Ctrl Pts',(4.40145272754258,-30.4907070441319,-13.6900312837157));
#53684=CARTESIAN_POINT('Ctrl Pts',(4.91805056385413,-30.4826845293831,-13.7084761779709));
#53685=CARTESIAN_POINT('Ctrl Pts',(5.791384213593,-30.4647401208151,-13.7499098195501));
#53686=CARTESIAN_POINT('Ctrl Pts',(6.46263952973601,-30.4660585960359,-13.7472501476117));
#53687=CARTESIAN_POINT('Ctrl Pts',(6.92897284878534,-30.4916153574711,-13.6871363494999));
#53688=CARTESIAN_POINT('Ctrl Pts',(7.05462978588519,-30.4989350691117,-13.6705906736548));
#53689=CARTESIAN_POINT('Ctrl Pts',(7.2330357976122,-30.5103941645259,-13.64535449053));
#53690=CARTESIAN_POINT('Ctrl Pts',(7.41402545512323,-30.5231160748026,-13.6178741235955));
#53691=CARTESIAN_POINT('Ctrl Pts',(7.77131680307424,-30.550583615613,-13.5590581898128));
#53692=CARTESIAN_POINT('Ctrl Pts',(8.29875758008135,-30.6000551322046,-13.4535786484538));
#53693=CARTESIAN_POINT('Ctrl Pts',(8.85376435941124,-30.6702769361216,-13.2940463367281));
#53694=CARTESIAN_POINT('Ctrl Pts',(9.27339243591186,-30.7356605585286,-13.1351572273555));
#53695=CARTESIAN_POINT('Ctrl Pts',(9.4742240152269,-30.7714246498893,-13.0444339073219));
#53696=CARTESIAN_POINT('Ctrl Pts',(10.0273297328825,-30.8765426957254,-12.7717645325826));
#53697=CARTESIAN_POINT('Ctrl Pts',(10.9572339063684,-31.1445192227213,-12.1307089623794));
#53698=CARTESIAN_POINT('Ctrl Pts',(11.8781426048001,-31.4831753576899,-11.2362716678478));
#53699=CARTESIAN_POINT('Ctrl Pts',(12.6020626440135,-31.7238287379969,-10.4893969835164));
#53700=CARTESIAN_POINT('Ctrl Pts',(13.0988736704966,-31.9043633305436,-9.92073242692073));
#53701=CARTESIAN_POINT('Ctrl Pts',(14.0796979680275,-32.2976015767017,-8.60937463783709));
#53702=CARTESIAN_POINT('Ctrl Pts',(14.767676431986,-32.5746344119006,-7.51992611358519));
#53703=CARTESIAN_POINT('Ctrl Pts',(15.5027273811337,-32.8079808305111,-6.32795870904283));
#53704=CARTESIAN_POINT('Ctrl Pts',(16.0202991032636,-32.9710575408164,-5.42474240090243));
#53705=CARTESIAN_POINT('Ctrl Pts',(17.0170548288356,-33.2543208336152,-3.48039388031436));
#53706=CARTESIAN_POINT('Ctrl Pts',(17.7141669052032,-33.3803196556765,-1.94722345366041));
#53707=CARTESIAN_POINT('Ctrl Pts',(18.451391136466,-33.4127835371598,-0.311140673056842));
#53708=CARTESIAN_POINT('Ctrl Pts',(18.9741597084201,-33.4081197665559,0.916672237872836));
#53709=CARTESIAN_POINT('Ctrl Pts',(19.9767059515643,-33.2711886970384,3.47029956120117));
#53710=CARTESIAN_POINT('Ctrl Pts',(20.683600748323,-33.0046898829411,5.4153715482179));
#53711=CARTESIAN_POINT('Ctrl Pts',(22.3785099788158,-32.036142933647,10.0079986575605));
#53712=CARTESIAN_POINT('Ctrl Pts',(23.4839952293235,-30.8044868476372,13.2681438080948));
#53713=CARTESIAN_POINT('Ctrl Pts',(24.4831092917558,-29.0356277561782,16.5096970084821));
#53714=CARTESIAN_POINT('Ctrl Pts',(2.09999999999999,-35.5190303723719,-16.1061388742308));
#53715=CARTESIAN_POINT('Ctrl Pts',(2.73333333333332,-35.5190303723719,-16.1061388742308));
#53716=CARTESIAN_POINT('Ctrl Pts',(3.3685529499539,-35.5189963826913,-16.1062755303871));
#53717=CARTESIAN_POINT('Ctrl Pts',(4.12893389176798,-35.5189883555912,-16.1063123113306));
#53718=CARTESIAN_POINT('Ctrl Pts',(4.40590876805926,-35.5167560554967,-16.1113705287801));
#53719=CARTESIAN_POINT('Ctrl Pts',(4.92495106442005,-35.5072455660771,-16.1329983700014));
#53720=CARTESIAN_POINT('Ctrl Pts',(5.79759451343229,-35.4861563499845,-16.181187912636));
#53721=CARTESIAN_POINT('Ctrl Pts',(6.4552933171533,-35.4879918202634,-16.1774408228987));
#53722=CARTESIAN_POINT('Ctrl Pts',(6.90777589770066,-35.5169934210011,-16.1098049933539));
#53723=CARTESIAN_POINT('Ctrl Pts',(7.03326597379373,-35.5255942090726,-16.090566148091));
#53724=CARTESIAN_POINT('Ctrl Pts',(7.20980469627123,-35.5389211123446,-16.0615220192229));
#53725=CARTESIAN_POINT('Ctrl Pts',(7.38928547178791,-35.5537484109996,-16.0298305624976));
#53726=CARTESIAN_POINT('Ctrl Pts',(7.74286592221491,-35.5856960588913,-15.9621555487075));
#53727=CARTESIAN_POINT('Ctrl Pts',(8.26401794171908,-35.6431524329166,-15.840991390971));
#53728=CARTESIAN_POINT('Ctrl Pts',(8.81152408908925,-35.7245572865462,-15.6581486065571));
#53729=CARTESIAN_POINT('Ctrl Pts',(9.22661397401185,-35.8006503185216,-15.4754672744663));
#53730=CARTESIAN_POINT('Ctrl Pts',(9.42598140904611,-35.8424916660102,-15.3707139312043));
#53731=CARTESIAN_POINT('Ctrl Pts',(9.976710666656,-35.9660011697121,-15.0547620286962));
#53732=CARTESIAN_POINT('Ctrl Pts',(10.9140166500484,-36.2852504824252,-14.301418631492));
#53733=CARTESIAN_POINT('Ctrl Pts',(11.8387266298368,-36.6869798302323,-13.2531154851079));
#53734=CARTESIAN_POINT('Ctrl Pts',(12.5644537233057,-36.9720369099943,-12.380341222988));
#53735=CARTESIAN_POINT('Ctrl Pts',(13.0663236803827,-37.1882014264798,-11.7094275168349));
#53736=CARTESIAN_POINT('Ctrl Pts',(14.0520240221945,-37.65549414411,-10.1712590536084));
#53737=CARTESIAN_POINT('Ctrl Pts',(14.7426139091248,-37.9842005172013,-8.89575090186054));
#53738=CARTESIAN_POINT('Ctrl Pts',(15.4784727169398,-38.2612735354973,-7.50405020937324));
#53739=CARTESIAN_POINT('Ctrl Pts',(15.9995906107788,-38.456495327364,-6.44277625931302));
#53740=CARTESIAN_POINT('Ctrl Pts',(16.9994487463634,-38.7947103989691,-4.16721681261721));
#53741=CARTESIAN_POINT('Ctrl Pts',(17.6981454111525,-38.9468546317636,-2.37398192696008));
#53742=CARTESIAN_POINT('Ctrl Pts',(18.4357121346094,-38.9897987920051,-0.463585233612633));
#53743=CARTESIAN_POINT('Ctrl Pts',(18.9608308592025,-38.9881432373632,0.975716140749977));
#53744=CARTESIAN_POINT('Ctrl Pts',(19.9653528594919,-38.8351271359227,3.96186424955774));
#53745=CARTESIAN_POINT('Ctrl Pts',(20.6729531153352,-38.5287766299084,6.23514955400077));
#53746=CARTESIAN_POINT('Ctrl Pts',(22.3680492077458,-37.4100161862565,11.5988469917284));
#53747=CARTESIAN_POINT('Ctrl Pts',(23.4757593035169,-35.9774143267865,15.4158344467734));
#53748=CARTESIAN_POINT('Ctrl Pts',(24.4767076204831,-33.9162528966534,19.2087170933586));
#53749=CARTESIAN_POINT('',(3.2,-34.2572188230213,-15.4984824583453));
#53750=CARTESIAN_POINT('Ctrl Pts',(3.2,-34.2572188230213,-15.4984824583453));
#53751=CARTESIAN_POINT('Ctrl Pts',(3.45174020130992,-33.5567398379256,-15.1611495581151));
#53752=CARTESIAN_POINT('Ctrl Pts',(3.71840125360142,-32.8479951510644,-14.8198361057081));
#53753=CARTESIAN_POINT('Ctrl Pts',(4.,-32.1353158291841,-14.4766278329416));
#53754=CARTESIAN_POINT('Ctrl Pts',(4.62816481260912,-30.5455357665781,-13.7110301053043));
#53755=CARTESIAN_POINT('Ctrl Pts',(5.32582967254414,-28.9317001372407,-13.0007563214461));
#53756=CARTESIAN_POINT('Ctrl Pts',(6.03866108353657,-27.4700228811071,-12.2911204000068));
#53757=CARTESIAN_POINT('Ctrl Pts',(6.32798218217299,-26.8767632925494,-12.0030962736052));
#53758=CARTESIAN_POINT('Ctrl Pts',(6.61604116814955,-26.3158796257153,-11.717411134043));
#53759=CARTESIAN_POINT('Ctrl Pts',(6.89476148100327,-25.8006837185162,-11.4328824518093));
#53760=CARTESIAN_POINT('Ctrl Pts',(7.65522892841368,-24.3950103664284,-10.6565673046356));
#53761=CARTESIAN_POINT('Ctrl Pts',(8.35226709293656,-23.2781841584713,-9.99003821184204));
#53762=CARTESIAN_POINT('Ctrl Pts',(8.7892632371809,-22.6126816498706,-9.5632075888662));
#53763=CARTESIAN_POINT('Ctrl Pts',(8.99031957804211,-22.3064924512345,-9.36682827441841));
#53764=CARTESIAN_POINT('Ctrl Pts',(9.18275522061529,-22.0230827498019,-9.17790378245122));
#53765=CARTESIAN_POINT('Ctrl Pts',(9.37496045909766,-21.7488041106976,-8.9863600510071));
#53766=CARTESIAN_POINT('Ctrl Pts',(9.48075233189684,-21.5978381374038,-8.88093227894211));
#53767=CARTESIAN_POINT('Ctrl Pts',(9.58626090848609,-21.4500100268611,-8.77491379472231));
#53768=CARTESIAN_POINT('Ctrl Pts',(9.69257910363365,-21.3038773401306,-8.66672356115102));
#53769=CARTESIAN_POINT('Ctrl Pts',(10.0319880469606,-20.8373650867963,-8.32133834459649));
#53770=CARTESIAN_POINT('Ctrl Pts',(10.3788056742595,-20.3884564675231,-7.95278423285573));
#53771=CARTESIAN_POINT('Ctrl Pts',(10.7756849085126,-19.9045583626959,-7.52432563668368));
#53772=CARTESIAN_POINT('Ctrl Pts',(10.8890930405622,-19.7662846123093,-7.40189371064982));
#53773=CARTESIAN_POINT('Ctrl Pts',(11.0576203524086,-19.5630034060169,-7.21920703316946));
#53774=CARTESIAN_POINT('Ctrl Pts',(11.2725125496543,-19.3123908782387,-6.98620793040072));
#53775=CARTESIAN_POINT('Ctrl Pts',(11.5968279595885,-18.9341663278698,-6.63456556973203));
#53776=CARTESIAN_POINT('Ctrl Pts',(12.0255678845029,-18.4509663195227,-6.16660018051478));
#53777=CARTESIAN_POINT('Ctrl Pts',(12.532035905153,-17.9090112566991,-5.64334903954311));
#53778=CARTESIAN_POINT('Ctrl Pts',(13.0988763177203,-17.3024536481663,-5.05772491219147));
#53779=CARTESIAN_POINT('Ctrl Pts',(13.7495416918469,-16.6567125930623,-4.35710056287699));
#53780=CARTESIAN_POINT('Ctrl Pts',(14.4398764942141,-16.0137917956181,-3.63694865307657));
#53781=CARTESIAN_POINT('Ctrl Pts',(14.7901814038696,-15.6875467459813,-3.27151328919831));
#53782=CARTESIAN_POINT('Ctrl Pts',(15.1459546152778,-15.3661826765097,-2.90956453468361));
#53783=CARTESIAN_POINT('Ctrl Pts',(15.4570717747561,-15.0907170797824,-2.60751868956995));
#53784=CARTESIAN_POINT('Ctrl Pts',(15.7998231405479,-14.7872423062749,-2.27476100395055));
#53785=CARTESIAN_POINT('Ctrl Pts',(16.0676294492373,-14.5587589003322,-2.012820704421));
#53786=CARTESIAN_POINT('Ctrl Pts',(16.3615307970805,-14.3129125519894,-1.7268209695992));
#53787=CARTESIAN_POINT('Ctrl Pts',(17.029661602165,-13.754025973718,-1.07665303235506));
#53788=CARTESIAN_POINT('Ctrl Pts',(17.70846918735,-13.2157293141182,-0.418819875773385));
#53789=CARTESIAN_POINT('Ctrl Pts',(18.4207032016838,-12.6778667357551,0.201349018822154));
#53790=CARTESIAN_POINT('Ctrl Pts',(18.8298642042311,-12.368877853777,0.5576208642475));
#53791=CARTESIAN_POINT('Ctrl Pts',(19.2113759272833,-12.0893434047209,0.892739516924111));
#53792=CARTESIAN_POINT('Ctrl Pts',(19.5701113607632,-11.8294329222545,1.20481008177065));
#53793=CARTESIAN_POINT('Ctrl Pts',(20.1215476021955,-11.4299071264062,1.68451463080629));
#53794=CARTESIAN_POINT('Ctrl Pts',(20.6514912601791,-11.0507292363155,2.14929111120006));
#53795=CARTESIAN_POINT('Ctrl Pts',(21.3979544325339,-10.5292525052453,2.73212531702577));
#53796=CARTESIAN_POINT('Ctrl Pts',(21.8107631282044,-10.2408657004461,3.05444400227331));
#53797=CARTESIAN_POINT('Ctrl Pts',(22.3076315955317,-9.89607813725398,3.43397758799233));
#53798=CARTESIAN_POINT('Ctrl Pts',(22.8472772295076,-9.51040350637145,3.84215125052754));
#53799=CARTESIAN_POINT('Ctrl Pts',(23.3953136568588,-9.11873213256344,4.25667148690292));
#53800=CARTESIAN_POINT('Ctrl Pts',(23.9608264583105,-8.70201347485439,4.68200859429454));
#53801=CARTESIAN_POINT('Ctrl Pts',(24.5,-8.27152931289794,5.09374822578144));
#53802=CARTESIAN_POINT('Ctrl Pts',(2.7976100639101,-35.1047407419896,-15.9066763790287));
#53803=CARTESIAN_POINT('Ctrl Pts',(2.93206313032129,-34.8224775747036,-15.7707621775971));
#53804=CARTESIAN_POINT('Ctrl Pts',(3.06672198084968,-34.5398707717893,-15.6346853141056));
#53805=CARTESIAN_POINT('Ctrl Pts',(3.20143373635558,-34.2571954190233,-15.4985756754768));
#53806=CARTESIAN_POINT('Origin',(2.9,0.,0.));
#53807=CARTESIAN_POINT('Origin',(3.2,0.,0.));
#53808=CARTESIAN_POINT('Ctrl Pts',(2.1,-9.132050144933,3.39883892972008));
#53809=CARTESIAN_POINT('Ctrl Pts',(2.73333333333333,-9.132050144933,3.39883892972008));
#53810=CARTESIAN_POINT('Ctrl Pts',(3.3663079725943,-9.13201814031333,3.39888229101301));
#53811=CARTESIAN_POINT('Ctrl Pts',(4.12416251276081,-9.13200839072933,3.3988953533008));
#53812=CARTESIAN_POINT('Ctrl Pts',(4.36791120644981,-9.13244533410776,3.39775559897473));
#53813=CARTESIAN_POINT('Ctrl Pts',(4.86514190730704,-9.13445129820771,3.39254860847465));
#53814=CARTESIAN_POINT('Ctrl Pts',(5.74556055405348,-9.13920122500316,3.38025835485548));
#53815=CARTESIAN_POINT('Ctrl Pts',(6.51833360630206,-9.13927981015121,3.3800633150153));
#53816=CARTESIAN_POINT('Ctrl Pts',(7.10306547172688,-9.13061179056261,3.40220636614938));
#53817=CARTESIAN_POINT('Ctrl Pts',(7.2302207071034,-9.12871923506172,3.40720377175751));
#53818=CARTESIAN_POINT('Ctrl Pts',(7.42490086908427,-9.12567677829264,3.41546028383053));
#53819=CARTESIAN_POINT('Ctrl Pts',(7.61947075258487,-9.12244641117515,3.42440794243591));
#53820=CARTESIAN_POINT('Ctrl Pts',(8.01071766333096,-9.11546267897863,3.44392145121506));
#53821=CARTESIAN_POINT('Ctrl Pts',(8.60078557051619,-9.10263571479926,3.47975799428797));
#53822=CARTESIAN_POINT('Ctrl Pts',(9.2514949577206,-9.08139957335397,3.53513809773506));
#53823=CARTESIAN_POINT('Ctrl Pts',(9.76261946444148,-9.0583588320315,3.59140175594612));
#53824=CARTESIAN_POINT('Ctrl Pts',(10.0141181534512,-9.0444728354789,3.62401874784084));
#53825=CARTESIAN_POINT('Ctrl Pts',(10.7177011859537,-9.00131652348988,3.72332977624404));
#53826=CARTESIAN_POINT('Ctrl Pts',(11.8208115644903,-8.90749893786242,3.94890859650272));
#53827=CARTESIAN_POINT('Ctrl Pts',(12.8079858159913,-8.78130149362605,4.22216464532031));
#53828=CARTESIAN_POINT('Ctrl Pts',(13.5603938947108,-8.6716091455336,4.43282977440356));
#53829=CARTESIAN_POINT('Ctrl Pts',(14.1415289562624,-8.57605910539162,4.61236119395963));
#53830=CARTESIAN_POINT('Ctrl Pts',(15.2007183254417,-8.36507036120484,4.99040411635023));
#53831=CARTESIAN_POINT('Ctrl Pts',(15.9285075560867,-8.18274706597629,5.28485668422829));
#53832=CARTESIAN_POINT('Ctrl Pts',(16.6747842807949,-7.97783754058137,5.57956090150159));
#53833=CARTESIAN_POINT('Ctrl Pts',(17.2498051121831,-7.80376743378315,5.81968941516198));
#53834=CARTESIAN_POINT('Ctrl Pts',(18.2984823004268,-7.4319812814029,6.29489826615604));
#53835=CARTESIAN_POINT('Ctrl Pts',(19.0236998873884,-7.12174287391437,6.64228560049974));
#53836=CARTESIAN_POINT('Ctrl Pts',(19.7682368455845,-6.78029956366935,6.98103393296198));
#53837=CARTESIAN_POINT('Ctrl Pts',(20.3331957372982,-6.49893080008033,7.24492384682381));
#53838=CARTESIAN_POINT('Ctrl Pts',(21.3723377324311,-5.90855985872452,7.74330400682432));
#53839=CARTESIAN_POINT('Ctrl Pts',(22.0962735028998,-5.43125088344887,8.08178692215916));
#53840=CARTESIAN_POINT('Ctrl Pts',(23.2302665631601,-4.65052680131279,8.5566407190325));
#53841=CARTESIAN_POINT('Ctrl Pts',(23.8854423668127,-4.14620302888525,8.80675749744808));
#53842=CARTESIAN_POINT('Ctrl Pts',(24.5000000001022,-3.61603013990409,9.0160298461823));
#53843=CARTESIAN_POINT('Ctrl Pts',(2.1,-12.9016211606665,5.21416865468984));
#53844=CARTESIAN_POINT('Ctrl Pts',(2.73333333333333,-12.9016211606665,5.21416865468984));
#53845=CARTESIAN_POINT('Ctrl Pts',(3.3661091233326,-12.9015874618483,5.21422021700749));
#53846=CARTESIAN_POINT('Ctrl Pts',(4.12374360042828,-12.9015773813688,5.21423545286286));
#53847=CARTESIAN_POINT('Ctrl Pts',(4.36463922026465,-12.9022430853862,5.212636908042));
#53848=CARTESIAN_POINT('Ctrl Pts',(4.85997974089114,-12.9053085358418,5.20530291707169));
#53849=CARTESIAN_POINT('Ctrl Pts',(5.74110524153444,-12.9125858457571,5.18793249877815));
#53850=CARTESIAN_POINT('Ctrl Pts',(6.5236553961773,-12.912769153219,5.18752851193186));
#53851=CARTESIAN_POINT('Ctrl Pts',(7.12002561380569,-12.8993507043393,5.21924743609842));
#53852=CARTESIAN_POINT('Ctrl Pts',(7.24732883907975,-12.8964478351332,5.22631376259351));
#53853=CARTESIAN_POINT('Ctrl Pts',(7.44361306854449,-12.8917537205922,5.23804414925047));
#53854=CARTESIAN_POINT('Ctrl Pts',(7.63952655731801,-12.8867672451576,5.25074673477078));
#53855=CARTESIAN_POINT('Ctrl Pts',(8.03414277825582,-12.8759684345895,5.27847963617582));
#53856=CARTESIAN_POINT('Ctrl Pts',(8.6304721476858,-12.8561250346134,5.32946386238128));
#53857=CARTESIAN_POINT('Ctrl Pts',(9.29103328875621,-12.8233137230442,5.4084727122217));
#53858=CARTESIAN_POINT('Ctrl Pts',(9.8120207794755,-12.7877516418428,5.48896946217565));
#53859=CARTESIAN_POINT('Ctrl Pts',(10.0691942302806,-12.7663266344001,5.53572936280494));
#53860=CARTESIAN_POINT('Ctrl Pts',(10.790046981849,-12.6997688928597,5.67826660603544));
#53861=CARTESIAN_POINT('Ctrl Pts',(11.9163416059387,-12.5548183870822,6.00137237696006));
#53862=CARTESIAN_POINT('Ctrl Pts',(12.9132756635671,-12.3622653266479,6.38911209475131));
#53863=CARTESIAN_POINT('Ctrl Pts',(13.6696998405866,-12.1964669129034,6.68651744379352));
#53864=CARTESIAN_POINT('Ctrl Pts',(14.2631317779486,-12.0507099019981,6.94299161237581));
#53865=CARTESIAN_POINT('Ctrl Pts',(15.3329015938421,-11.7312148722742,7.47865016429502));
#53866=CARTESIAN_POINT('Ctrl Pts',(16.0654051873355,-11.4576547378963,7.89313324640987));
#53867=CARTESIAN_POINT('Ctrl Pts',(16.813125378213,-11.152369030053,8.30562093805636));
#53868=CARTESIAN_POINT('Ctrl Pts',(17.3939613704063,-10.8918326264795,8.64433036386289));
#53869=CARTESIAN_POINT('Ctrl Pts',(18.4451989758741,-10.3392458422533,9.30923518676035));
#53870=CARTESIAN_POINT('Ctrl Pts',(19.1720929876942,-9.88132720383576,9.79256593426711));
#53871=CARTESIAN_POINT('Ctrl Pts',(19.9174587712572,-9.3790868197873,10.2616497070843));
#53872=CARTESIAN_POINT('Ctrl Pts',(20.4827049382928,-8.96580926313345,10.6274510023226));
#53873=CARTESIAN_POINT('Ctrl Pts',(21.5194880485299,-8.10240134706929,11.3134235687948));
#53874=CARTESIAN_POINT('Ctrl Pts',(22.2433743515511,-7.40711512464527,11.7762751484356));
#53875=CARTESIAN_POINT('Ctrl Pts',(23.3781098890497,-6.27155818967328,12.4208354707857));
#53876=CARTESIAN_POINT('Ctrl Pts',(24.0312127056184,-5.54246593554869,12.7565226911889));
#53877=CARTESIAN_POINT('Ctrl Pts',(24.6419825553303,-4.77938339662506,13.0322784684415));
#53878=CARTESIAN_POINT('Ctrl Pts',(2.1,-21.6972868640446,9.4499380129526));
#53879=CARTESIAN_POINT('Ctrl Pts',(2.73333333333333,-21.6972868640446,9.4499380129526));
#53880=CARTESIAN_POINT('Ctrl Pts',(3.36562354525866,-21.6971828798135,9.45008587645688));
#53881=CARTESIAN_POINT('Ctrl Pts',(4.12273867778471,-21.697151611036,9.45012970586554));
#53882=CARTESIAN_POINT('Ctrl Pts',(4.35697313403335,-21.6983286095062,9.44750243336562));
#53883=CARTESIAN_POINT('Ctrl Pts',(4.84791259063805,-21.7038201038517,9.43528956102119));
#53884=CARTESIAN_POINT('Ctrl Pts',(5.7306447376668,-21.7169845344723,9.40607010718203));
#53885=CARTESIAN_POINT('Ctrl Pts',(6.53607333749491,-21.7174761488546,9.40495984396926));
#53886=CARTESIAN_POINT('Ctrl Pts',(7.15932985413337,-21.6923174381321,9.46034624187088));
#53887=CARTESIAN_POINT('Ctrl Pts',(7.28697322394794,-21.6870460982782,9.4722604919422));
#53888=CARTESIAN_POINT('Ctrl Pts',(7.48695635027016,-21.6784001614658,9.49229325078789));
#53889=CARTESIAN_POINT('Ctrl Pts',(7.68595777901539,-21.6692216654712,9.51394386312415));
#53890=CARTESIAN_POINT('Ctrl Pts',(8.0883081610984,-21.6492812399527,9.56133749836178));
#53891=CARTESIAN_POINT('Ctrl Pts',(8.69888136072734,-21.6124584984937,9.6488222621323));
#53892=CARTESIAN_POINT('Ctrl Pts',(9.381381730169,-21.5513928087426,9.78536670703229));
#53893=CARTESIAN_POINT('Ctrl Pts',(9.92338843691519,-21.4849895522994,9.92550005748472));
#53894=CARTESIAN_POINT('Ctrl Pts',(10.1921295368678,-21.4448781952111,10.0073116343241));
#53895=CARTESIAN_POINT('Ctrl Pts',(10.9469244149175,-21.3199576370334,10.257585612213));
#53896=CARTESIAN_POINT('Ctrl Pts',(12.1071221516794,-21.0489433681523,10.8194689670457));
#53897=CARTESIAN_POINT('Ctrl Pts',(13.1093104456794,-20.6990109732753,11.4761470369039));
#53898=CARTESIAN_POINT('Ctrl Pts',(13.8683648550469,-20.4006353577185,11.9768494012792));
#53899=CARTESIAN_POINT('Ctrl Pts',(14.4658363655178,-20.136535574814,12.413145511352));
#53900=CARTESIAN_POINT('Ctrl Pts',(15.5292386507845,-19.5672964049095,13.3088706944097));
#53901=CARTESIAN_POINT('Ctrl Pts',(16.2561779329736,-19.0831769560747,13.9986415819097));
#53902=CARTESIAN_POINT('Ctrl Pts',(17.0018880874651,-18.5434600004101,14.6847508610486));
#53903=CARTESIAN_POINT('Ctrl Pts',(17.5710595442823,-18.0894667653548,15.2426602928667));
#53904=CARTESIAN_POINT('Ctrl Pts',(18.6068613700326,-17.129093535584,16.3355437642704));
#53905=CARTESIAN_POINT('Ctrl Pts',(19.3243916655247,-16.3344548929372,17.1296950555117));
#53906=CARTESIAN_POINT('Ctrl Pts',(20.0666972723063,-15.4594613044778,17.9021666930174));
#53907=CARTESIAN_POINT('Ctrl Pts',(20.6168159622415,-14.7547166790696,18.4938305405518));
#53908=CARTESIAN_POINT('Ctrl Pts',(21.6393971978862,-13.274017342785,19.6095065175213));
#53909=CARTESIAN_POINT('Ctrl Pts',(22.3554713915253,-12.0805610478001,20.3609361957837));
#53910=CARTESIAN_POINT('Ctrl Pts',(23.4866975992548,-10.1234946186001,21.4058157420793));
#53911=CARTESIAN_POINT('Ctrl Pts',(24.125246467622,-8.89054296253175,21.9361966402162));
#53912=CARTESIAN_POINT('Ctrl Pts',(24.727666267572,-7.59819629859098,22.3697186090524));
#53913=CARTESIAN_POINT('Ctrl Pts',(2.1,-30.4929525674227,13.6857073712154));
#53914=CARTESIAN_POINT('Ctrl Pts',(2.73333333333333,-30.4929525674227,13.6857073712154));
#53915=CARTESIAN_POINT('Ctrl Pts',(3.36508111731483,-30.4928630358999,13.6858268427981));
#53916=CARTESIAN_POINT('Ctrl Pts',(4.12166372313058,-30.4928374222987,13.6858596139329));
#53917=CARTESIAN_POINT('Ctrl Pts',(4.34922070449677,-30.49449304522,13.6822752188327));
#53918=CARTESIAN_POINT('Ctrl Pts',(4.83581952795261,-30.5023484303467,13.6653239915311));
#53919=CARTESIAN_POINT('Ctrl Pts',(5.71994990272322,-30.5214481532399,13.6241663122579));
#53920=CARTESIAN_POINT('Ctrl Pts',(6.54867625091358,-30.5227115994799,13.6214678470964));
#53921=CARTESIAN_POINT('Ctrl Pts',(7.19744568466461,-30.4845039603552,13.7032562477442));
#53922=CARTESIAN_POINT('Ctrl Pts',(7.32540386607941,-30.4768448962739,13.7200563246537));
#53923=CARTESIAN_POINT('Ctrl Pts',(7.52886144254688,-30.4640499949291,13.7487976356855));
#53924=CARTESIAN_POINT('Ctrl Pts',(7.73071526159972,-30.4505000752736,13.7797645234549));
#53925=CARTESIAN_POINT('Ctrl Pts',(8.14014718867705,-30.4209316168907,13.8478073053149));
#53926=CARTESIAN_POINT('Ctrl Pts',(8.76321456595858,-30.3661751673437,13.9737656730329));
#53927=CARTESIAN_POINT('Ctrl Pts',(9.46268739969009,-30.274901687886,14.1717203974558));
#53928=CARTESIAN_POINT('Ctrl Pts',(10.017555629263,-30.1757507026565,14.3751176598203));
#53929=CARTESIAN_POINT('Ctrl Pts',(10.2918140826348,-30.1160627467491,14.4936111394812));
#53930=CARTESIAN_POINT('Ctrl Pts',(11.0595965108885,-29.9308924752226,14.8550046648317));
#53931=CARTESIAN_POINT('Ctrl Pts',(12.2112890847585,-29.538742900038,15.6451338086644));
#53932=CARTESIAN_POINT('Ctrl Pts',(13.2034136834303,-29.0396659631087,16.5569799806426));
#53933=CARTESIAN_POINT('Ctrl Pts',(13.9587824395507,-28.6121062675108,17.2559421918816));
#53934=CARTESIAN_POINT('Ctrl Pts',(14.5428434697006,-28.2415332240579,17.8540725971182));
#53935=CARTESIAN_POINT('Ctrl Pts',(15.5916053350762,-27.4389567528664,19.089267636165));
#53936=CARTESIAN_POINT('Ctrl Pts',(16.312366647535,-26.7539934204414,20.045818201422));
#53937=CARTESIAN_POINT('Ctrl Pts',(17.0564138076615,-25.9843342941303,21.0043101087993));
#53938=CARTESIAN_POINT('Ctrl Pts',(17.6163463570722,-25.3506638339921,21.7688212811574));
#53939=CARTESIAN_POINT('Ctrl Pts',(18.6452383036686,-23.9966999747395,23.2835440124754));
#53940=CARTESIAN_POINT('Ctrl Pts',(19.3594664110678,-22.873824767894,24.3879531932759));
#53941=CARTESIAN_POINT('Ctrl Pts',(20.100955640781,-21.6310467382024,25.4670642243813));
#53942=CARTESIAN_POINT('Ctrl Pts',(20.6466714554163,-20.6438263892792,26.2831266089234));
#53943=CARTESIAN_POINT('Ctrl Pts',(21.666430039865,-18.5543852156517,27.8345444051144));
#53944=CARTESIAN_POINT('Ctrl Pts',(22.3810701794161,-16.8676153595205,28.8806138340969));
#53945=CARTESIAN_POINT('Ctrl Pts',(23.5117719637955,-14.094719744574,30.3366076891904));
#53946=CARTESIAN_POINT('Ctrl Pts',(24.1480627906507,-12.3610095563398,31.0685341627222));
#53947=CARTESIAN_POINT('Ctrl Pts',(24.7493903499091,-10.540466346655,31.6671511473888));
#53948=CARTESIAN_POINT('Ctrl Pts',(2.1,-35.5190472550673,16.1061470045084));
#53949=CARTESIAN_POINT('Ctrl Pts',(2.73333333333333,-35.5190472550673,16.1061470045084));
#53950=CARTESIAN_POINT('Ctrl Pts',(3.36475413268099,-35.5189670351233,16.1062505100172));
#53951=CARTESIAN_POINT('Ctrl Pts',(4.12102956711596,-35.5189449021359,16.1062772345771));
#53952=CARTESIAN_POINT('Ctrl Pts',(4.34476326499953,-35.5208619030567,16.1021711888042));
#53953=CARTESIAN_POINT('Ctrl Pts',(4.82891764559021,-35.5300406854563,16.0825700940178));
#53954=CARTESIAN_POINT('Ctrl Pts',(5.71373811875233,-35.5525489027151,16.0345554335906));
#53955=CARTESIAN_POINT('Ctrl Pts',(6.55602060536393,-35.5543403393864,16.0307742128651));
#53956=CARTESIAN_POINT('Ctrl Pts',(7.21864005381085,-35.5082991666069,16.1284303018243));
#53957=CARTESIAN_POINT('Ctrl Pts',(7.34676507585227,-35.4992701924678,16.1480328226317));
#53958=CARTESIAN_POINT('Ctrl Pts',(7.55208983697808,-35.4840500176732,16.1818617453272));
#53959=CARTESIAN_POINT('Ctrl Pts',(7.75545246761066,-35.4679543088847,16.2182492540178));
#53960=CARTESIAN_POINT('Ctrl Pts',(8.16859508244807,-35.432763206004,16.2983357838761));
#53961=CARTESIAN_POINT('Ctrl Pts',(8.79795126468624,-35.3675282937919,16.4467433812652));
#53962=CARTESIAN_POINT('Ctrl Pts',(9.50492466084984,-35.2587512344281,16.6802493752873));
#53963=CARTESIAN_POINT('Ctrl Pts',(10.0643308640972,-35.1410338487819,16.9194777147605));
#53964=CARTESIAN_POINT('Ctrl Pts',(10.3400534304426,-35.0704395069489,17.0583708781951));
#53965=CARTESIAN_POINT('Ctrl Pts',(11.1102119878275,-34.8520710674395,17.4808514386373));
#53966=CARTESIAN_POINT('Ctrl Pts',(12.2545037825343,-34.3944746405569,18.3945372313141));
#53967=CARTESIAN_POINT('Ctrl Pts',(13.2428241044381,-33.8115307458597,19.45071368533));
#53968=CARTESIAN_POINT('Ctrl Pts',(13.996383095991,-33.3108813879676,20.2623381758305));
#53969=CARTESIAN_POINT('Ctrl Pts',(14.5753829446244,-32.8807198531287,20.9514986906474));
#53970=CARTESIAN_POINT('Ctrl Pts',(15.6192678372118,-31.9450395751563,22.3814785397995));
#53971=CARTESIAN_POINT('Ctrl Pts',(16.3374176744543,-31.1455802637508,23.4909182338773));
#53972=CARTESIAN_POINT('Ctrl Pts',(17.0806574874892,-30.2449968793303,24.6052817498839));
#53973=CARTESIAN_POINT('Ctrl Pts',(17.6370457520303,-29.5081260556649,25.4890808130937));
#53974=CARTESIAN_POINT('Ctrl Pts',(18.6628364663185,-27.9284442945199,27.2466455033113));
#53975=CARTESIAN_POINT('Ctrl Pts',(19.3754944079007,-26.618087896118,28.5289319062647));
#53976=CARTESIAN_POINT('Ctrl Pts',(20.1166524072473,-25.1655401045655,29.7835633599642));
#53977=CARTESIAN_POINT('Ctrl Pts',(20.6600335100608,-24.0162045057133,30.728885186263));
#53978=CARTESIAN_POINT('Ctrl Pts',(21.6778210050225,-21.5784381766374,32.5302297375723));
#53979=CARTESIAN_POINT('Ctrl Pts',(22.3918241741696,-19.6099219678105,33.7451822199181));
#53980=CARTESIAN_POINT('Ctrl Pts',(23.5225185291349,-16.371232079717,35.4366819891224));
#53981=CARTESIAN_POINT('Ctrl Pts',(24.157514841919,-14.3511368126248,36.2844930251905));
#53982=CARTESIAN_POINT('Ctrl Pts',(24.7577717974218,-12.2286456156553,36.977739523394));
#53983=CARTESIAN_POINT('',(24.5,-3.6160301400213,9.01602984623715));
#53984=CARTESIAN_POINT('Ctrl Pts',(24.5,-3.6160301400213,9.01602984623715));
#53985=CARTESIAN_POINT('Ctrl Pts',(23.8274939346415,-4.25320160821626,8.96293929686807));
#53986=CARTESIAN_POINT('Ctrl Pts',(23.3366347313213,-4.69799730977943,8.91872338222509));
#53987=CARTESIAN_POINT('Ctrl Pts',(22.5855494187791,-5.38681087917914,8.84785629468263));
#53988=CARTESIAN_POINT('Ctrl Pts',(22.2454144271855,-5.69874561378915,8.81576356723475));
#53989=CARTESIAN_POINT('Ctrl Pts',(21.8382660741845,-6.08207973842203,8.77028857443063));
#53990=CARTESIAN_POINT('Ctrl Pts',(21.3802156946739,-6.52138636350872,8.71704071219447));
#53991=CARTESIAN_POINT('Ctrl Pts',(20.76946932905,-7.10714054398311,8.64604210638015));
#53992=CARTESIAN_POINT('Ctrl Pts',(20.1629003032131,-7.69806831767953,8.57558750201974));
#53993=CARTESIAN_POINT('Ctrl Pts',(19.5574857571565,-8.2922929633463,8.53317747320063));
#53994=CARTESIAN_POINT('Ctrl Pts',(18.6418529406584,-9.19100210320499,8.46903627542409));
#53995=CARTESIAN_POINT('Ctrl Pts',(17.7734813303986,-10.1341856434662,8.39329925092376));
#53996=CARTESIAN_POINT('Ctrl Pts',(16.962125308111,-11.0447214443253,8.38345588031826));
#53997=CARTESIAN_POINT('Ctrl Pts',(16.8133360650119,-11.211698614523,8.38165076934145));
#53998=CARTESIAN_POINT('Ctrl Pts',(16.6656205359918,-11.3787950950318,8.38175879297581));
#53999=CARTESIAN_POINT('Ctrl Pts',(16.5183901926363,-11.5466151675562,8.38398696714523));
#54000=CARTESIAN_POINT('Ctrl Pts',(15.726452288761,-12.4493032509656,8.39597210241662));
#54001=CARTESIAN_POINT('Ctrl Pts',(14.9462259720485,-13.4308510041996,8.39966576114259));
#54002=CARTESIAN_POINT('Ctrl Pts',(14.2963150416359,-14.2718135557227,8.45082997390809));
#54003=CARTESIAN_POINT('Ctrl Pts',(13.9908350935056,-14.6670941774161,8.47487887096513));
#54004=CARTESIAN_POINT('Ctrl Pts',(13.7077063567372,-15.0401421211308,8.50738131960351));
#54005=CARTESIAN_POINT('Ctrl Pts',(13.4460198946299,-15.3890269033268,8.54665986878341));
#54006=CARTESIAN_POINT('Ctrl Pts',(12.837329540793,-16.2005430964578,8.63802292136927));
#54007=CARTESIAN_POINT('Ctrl Pts',(12.3530827413148,-16.8928758746813,8.71916608145024));
#54008=CARTESIAN_POINT('Ctrl Pts',(11.9770275692621,-17.438094619976,8.79813803422803));
#54009=CARTESIAN_POINT('Ctrl Pts',(11.6553972431166,-17.9044062037594,8.86568071630212));
#54010=CARTESIAN_POINT('Ctrl Pts',(11.3684205616876,-18.3299004046869,8.93687349930713));
#54011=CARTESIAN_POINT('Ctrl Pts',(11.0710856781329,-18.7780770165651,9.0258659640707));
#54012=CARTESIAN_POINT('Ctrl Pts',(10.8141787015661,-19.165316135464,9.10275833803743));
#54013=CARTESIAN_POINT('Ctrl Pts',(10.5576802661834,-19.557808848585,9.19120852767749));
#54014=CARTESIAN_POINT('Ctrl Pts',(10.2957959918397,-19.9646028342318,9.29767556265455));
#54015=CARTESIAN_POINT('Ctrl Pts',(9.71459276345261,-20.8674060985318,9.53395925933903));
#54016=CARTESIAN_POINT('Ctrl Pts',(9.09527967376161,-21.8590210236913,9.85968483500704));
#54017=CARTESIAN_POINT('Ctrl Pts',(8.43168033652491,-23.0030033264912,10.2883786384855));
#54018=CARTESIAN_POINT('Ctrl Pts',(7.97964340480209,-23.7822721127686,10.5804003761503));
#54019=CARTESIAN_POINT('Ctrl Pts',(7.52291961074489,-24.6086571529433,10.9125713605893));
#54020=CARTESIAN_POINT('Ctrl Pts',(7.10363554125516,-25.4084375301234,11.2437787817976));
#54021=CARTESIAN_POINT('Ctrl Pts',(6.56327799553922,-26.4391644123796,11.670626454462));
#54022=CARTESIAN_POINT('Ctrl Pts',(6.08559840020574,-27.3990249331094,12.1272301632502));
#54023=CARTESIAN_POINT('Ctrl Pts',(5.61708670825588,-28.397040125486,12.6190019907712));
#54024=CARTESIAN_POINT('Ctrl Pts',(5.04102956501762,-29.6241467068311,13.2236585638182));
#54025=CARTESIAN_POINT('Ctrl Pts',(4.50102820502357,-30.867297253229,13.8659822705852));
#54026=CARTESIAN_POINT('Ctrl Pts',(4.,-32.1353158291841,14.4766278329416));
#54027=CARTESIAN_POINT('Ctrl Pts',(3.72183418897115,-32.8393069658979,14.8156520962484));
#54028=CARTESIAN_POINT('Ctrl Pts',(3.45538353518228,-33.5466020895644,15.1562674758126));
#54029=CARTESIAN_POINT('Ctrl Pts',(3.2,-34.2572188230213,15.4984824583453));
#54030=CARTESIAN_POINT('',(24.5,-9.18141366427805,25.390975623741));
#54031=CARTESIAN_POINT('Ctrl Pts',(24.5,-9.18141366427807,25.390975623741));
#54032=CARTESIAN_POINT('Ctrl Pts',(24.5,-8.77450678650653,24.2210276048427));
#54033=CARTESIAN_POINT('Ctrl Pts',(24.5,-8.37535144524489,23.0706175167593));
#54034=CARTESIAN_POINT('Ctrl Pts',(24.5,-6.73049557719857,18.3152928195099));
#54035=CARTESIAN_POINT('Ctrl Pts',(24.5,-4.99261102906233,13.2639411997441));
#54036=CARTESIAN_POINT('Ctrl Pts',(24.5,-3.6160301400213,9.01602984623715));
#54037=CARTESIAN_POINT('',(10.2670750393577,-30.770480162676,14.8182822548653));
#54038=CARTESIAN_POINT('Ctrl Pts',(10.2670750393577,-30.770480162676,14.8182822548653));
#54039=CARTESIAN_POINT('Ctrl Pts',(11.2293198185888,-29.7752240113353,14.8555820456021));
#54040=CARTESIAN_POINT('Ctrl Pts',(12.092802582344,-28.8440362457489,15.1636363299831));
#54041=CARTESIAN_POINT('Ctrl Pts',(14.3080979519049,-26.4010410885782,16.2798551113026));
#54042=CARTESIAN_POINT('Ctrl Pts',(14.8952017874601,-25.7386194595791,16.6851511994675));
#54043=CARTESIAN_POINT('Ctrl Pts',(17.0803363586062,-22.9312839164232,18.4974195815112));
#54044=CARTESIAN_POINT('Ctrl Pts',(17.6922811489506,-22.0817386820725,19.0546305604886));
#54045=CARTESIAN_POINT('Ctrl Pts',(19.0755427322033,-19.9947258593395,20.4139220475843));
#54046=CARTESIAN_POINT('Ctrl Pts',(20.2687424742408,-18.1038001636999,21.6078133727585));
#54047=CARTESIAN_POINT('Ctrl Pts',(22.3267279388309,-14.0665238542576,23.6582159112932));
#54048=CARTESIAN_POINT('Ctrl Pts',(23.4192562717209,-11.8118967310364,24.635842795693));
#54049=CARTESIAN_POINT('Ctrl Pts',(24.5,-9.18141366427807,25.390975623741));
#54050=CARTESIAN_POINT('Ctrl Pts',(6.,-35.548403009865,16.0409177869666));
#54051=CARTESIAN_POINT('Ctrl Pts',(7.51604047332548,-33.6030946132751,15.107667867014));
#54052=CARTESIAN_POINT('Ctrl Pts',(9.08449301626627,-31.993289619074,14.872473123897));
#54053=CARTESIAN_POINT('Ctrl Pts',(9.8624969752411,-31.1881020850933,14.8146152631462));
#54054=CARTESIAN_POINT('Ctrl Pts',(10.0667253012217,-30.97770322442,14.8105160362608));
#54055=CARTESIAN_POINT('Ctrl Pts',(10.2670750393577,-30.770480162676,14.8182822548653));
#54056=CARTESIAN_POINT('Origin',(24.5,-7.65823537717056,3.68801178249925));
#54057=CARTESIAN_POINT('',(24.5,-1.17476144568584,9.64284209699151));
#54058=CARTESIAN_POINT('Ctrl Pts',(24.5,-1.17476144568584,9.64284209699151));
#54059=CARTESIAN_POINT('Ctrl Pts',(24.5,-1.44558163417187,9.6098488038372));
#54060=CARTESIAN_POINT('Ctrl Pts',(24.5,-1.71513676748961,9.56543133792098));
#54061=CARTESIAN_POINT('Ctrl Pts',(24.5,-2.54106347065763,9.39323084353225));
#54062=CARTESIAN_POINT('Ctrl Pts',(24.5,-3.0875901120013,9.22796959145788));
#54063=CARTESIAN_POINT('Ctrl Pts',(24.5,-3.6160301400213,9.01602984623715));
#54064=CARTESIAN_POINT('',(24.5,-4.10202091932642,26.6865776070557));
#54065=CARTESIAN_POINT('Ctrl Pts',(24.5,-1.17476144568584,9.64284209699151));
#54066=CARTESIAN_POINT('Ctrl Pts',(24.5,-1.96806264976098,13.8771085227549));
#54067=CARTESIAN_POINT('Ctrl Pts',(24.5,-2.92680106052676,19.5450505664343));
#54068=CARTESIAN_POINT('Ctrl Pts',(24.5,-4.10202091932642,26.6865776070557));
#54069=CARTESIAN_POINT('Origin',(24.5,0.,0.));
#54070=CARTESIAN_POINT('Ctrl Pts',(24.5,-4.10202064021797,26.6865776499578));
#54071=CARTESIAN_POINT('Ctrl Pts',(24.5,-18.1565214583376,24.5262462204244));
#54072=CARTESIAN_POINT('Ctrl Pts',(24.5,-24.3261594333653,11.7148609561741));
#54073=CARTESIAN_POINT('Ctrl Pts',(24.5,-36.0410203895394,-12.6112984771912));
#54074=CARTESIAN_POINT('Ctrl Pts',(24.5,-11.7148609561741,-24.3261594333653));
#54075=CARTESIAN_POINT('Ctrl Pts',(24.5,12.6112984771912,-36.0410203895394));
#54076=CARTESIAN_POINT('Ctrl Pts',(24.5,24.3261594333653,-11.7148609561741));
#54077=CARTESIAN_POINT('Ctrl Pts',(24.5,36.0410203895394,12.6112984771912));
#54078=CARTESIAN_POINT('Ctrl Pts',(24.5,11.7148609561741,24.3261594333653));
#54079=CARTESIAN_POINT('Ctrl Pts',(24.5,4.17235284052387,27.9584399040123));
#54080=CARTESIAN_POINT('Ctrl Pts',(24.5,-4.10202064021797,26.6865776499578));
#54081=CARTESIAN_POINT('Ctrl Pts',(24.3078118955742,-4.10700177686883,26.7189835059193));
#54082=CARTESIAN_POINT('Ctrl Pts',(24.3078118955742,-18.1785691568795,24.5560287580252));
#54083=CARTESIAN_POINT('Ctrl Pts',(24.3078118955742,-24.355699002996,11.7290864631587));
#54084=CARTESIAN_POINT('Ctrl Pts',(24.3078118955742,-36.0847854661547,-12.6266125398373));
#54085=CARTESIAN_POINT('Ctrl Pts',(24.3078118955742,-11.7290864631587,-24.355699002996));
#54086=CARTESIAN_POINT('Ctrl Pts',(24.3078118955742,12.6266125398373,-36.0847854661547));
#54087=CARTESIAN_POINT('Ctrl Pts',(24.3078118955742,24.355699002996,-11.7290864631587));
#54088=CARTESIAN_POINT('Ctrl Pts',(24.3078118955742,36.0847854661547,12.6266125398373));
#54089=CARTESIAN_POINT('Ctrl Pts',(24.3078118955742,11.7290864631587,24.355699002996));
#54090=CARTESIAN_POINT('Ctrl Pts',(24.3078118955742,4.17741938247407,27.9923901987381));
#54091=CARTESIAN_POINT('Ctrl Pts',(24.3078118955742,-4.10700177686883,26.7189835059193));
#54092=CARTESIAN_POINT('Ctrl Pts',(23.9225830034177,-4.11759678467036,26.7879116082368));
#54093=CARTESIAN_POINT('Ctrl Pts',(23.9225830034177,-18.2254651877316,24.6193769936484));
#54094=CARTESIAN_POINT('Ctrl Pts',(23.9225830034177,-24.4185304393985,11.7593444881934));
#54095=CARTESIAN_POINT('Ctrl Pts',(23.9225830034177,-36.1778749275919,-12.6591859512051));
#54096=CARTESIAN_POINT('Ctrl Pts',(23.9225830034177,-11.7593444881934,-24.4185304393985));
#54097=CARTESIAN_POINT('Ctrl Pts',(23.9225830034177,12.6591859512051,-36.1778749275919));
#54098=CARTESIAN_POINT('Ctrl Pts',(23.9225830034177,24.4185304393985,-11.7593444881934));
#54099=CARTESIAN_POINT('Ctrl Pts',(23.9225830034177,36.1778749275919,12.6591859512051));
#54100=CARTESIAN_POINT('Ctrl Pts',(23.9225830034177,11.7593444881934,24.4185304393985));
#54101=CARTESIAN_POINT('Ctrl Pts',(23.9225830034177,4.18819604957873,28.0646033626596));
#54102=CARTESIAN_POINT('Ctrl Pts',(23.9225830034177,-4.11759678467036,26.7879116082368));
#54103=CARTESIAN_POINT('Ctrl Pts',(23.3421815947946,-4.13538749346637,26.9036528912225));
#54104=CARTESIAN_POINT('Ctrl Pts',(23.3421815947946,-18.3042111069615,24.7257487900476));
#54105=CARTESIAN_POINT('Ctrl Pts',(23.3421815947946,-24.5240344474382,11.8101525406477));
#54106=CARTESIAN_POINT('Ctrl Pts',(23.3421815947946,-36.3341869880859,-12.7138819067904));
#54107=CARTESIAN_POINT('Ctrl Pts',(23.3421815947946,-11.8101525406477,-24.5240344474382));
#54108=CARTESIAN_POINT('Ctrl Pts',(23.3421815947946,12.7138819067904,-36.3341869880859));
#54109=CARTESIAN_POINT('Ctrl Pts',(23.3421815947946,24.5240344474382,-11.8101525406477));
#54110=CARTESIAN_POINT('Ctrl Pts',(23.3421815947946,36.3341869880859,12.7138819067904));
#54111=CARTESIAN_POINT('Ctrl Pts',(23.3421815947946,11.8101525406477,24.5240344474382));
#54112=CARTESIAN_POINT('Ctrl Pts',(23.3421815947946,4.20629179333296,28.1858607882918));
#54113=CARTESIAN_POINT('Ctrl Pts',(23.3421815947946,-4.13538749346637,26.9036528912225));
#54114=CARTESIAN_POINT('Ctrl Pts',(22.5631762070947,-4.16292037730343,27.0827739895517));
#54115=CARTESIAN_POINT('Ctrl Pts',(22.5631762070947,-18.4260782158922,24.8903696799392));
#54116=CARTESIAN_POINT('Ctrl Pts',(22.5631762070947,-24.6873123488983,11.8887830338031));
#54117=CARTESIAN_POINT('Ctrl Pts',(22.5631762070947,-36.5760953827013,-12.7985293150952));
#54118=CARTESIAN_POINT('Ctrl Pts',(22.5631762070947,-11.8887830338031,-24.6873123488983));
#54119=CARTESIAN_POINT('Ctrl Pts',(22.5631762070947,12.7985293150952,-36.5760953827013));
#54120=CARTESIAN_POINT('Ctrl Pts',(22.5631762070947,24.6873123488983,-11.8887830338031));
#54121=CARTESIAN_POINT('Ctrl Pts',(22.5631762070947,36.5760953827013,12.7985293150952));
#54122=CARTESIAN_POINT('Ctrl Pts',(22.5631762070947,11.8887830338031,24.6873123488983));
#54123=CARTESIAN_POINT('Ctrl Pts',(22.5631762070947,4.23429674897826,28.3735186636802));
#54124=CARTESIAN_POINT('Ctrl Pts',(22.5631762070947,-4.16292037730343,27.0827739895517));
#54125=CARTESIAN_POINT('Ctrl Pts',(21.5808622776984,-4.20380096926686,27.3487314742879));
#54126=CARTESIAN_POINT('Ctrl Pts',(21.5808622776984,-18.6070254636793,25.1347973784011));
#54127=CARTESIAN_POINT('Ctrl Pts',(21.5808622776984,-24.929745989549,12.0055329218856));
#54128=CARTESIAN_POINT('Ctrl Pts',(21.5808622776984,-36.9352789114346,-12.9242130676634));
#54129=CARTESIAN_POINT('Ctrl Pts',(21.5808622776984,-12.0055329218856,-24.929745989549));
#54130=CARTESIAN_POINT('Ctrl Pts',(21.5808622776984,12.9242130676634,-36.9352789114346));
#54131=CARTESIAN_POINT('Ctrl Pts',(21.5808622776984,24.929745989549,-12.0055329218856));
#54132=CARTESIAN_POINT('Ctrl Pts',(21.5808622776984,36.9352789114346,12.9242130676634));
#54133=CARTESIAN_POINT('Ctrl Pts',(21.5808622776984,12.0055329218856,24.929745989549));
#54134=CARTESIAN_POINT('Ctrl Pts',(21.5808622776984,4.27587826915116,28.6521514824534));
#54135=CARTESIAN_POINT('Ctrl Pts',(21.5808622776984,-4.20380096926686,27.3487314742879));
#54136=CARTESIAN_POINT('Ctrl Pts',(20.5902243197586,-4.25132104313727,27.6578835367717));
#54137=CARTESIAN_POINT('Ctrl Pts',(20.5902243197586,-18.8173606415355,25.4189229678073));
#54138=CARTESIAN_POINT('Ctrl Pts',(20.5902243197586,-25.2115536630461,12.141244344827));
#54139=CARTESIAN_POINT('Ctrl Pts',(20.5902243197586,-37.3527980078731,-13.0703093182191));
#54140=CARTESIAN_POINT('Ctrl Pts',(20.5902243197586,-12.141244344827,-25.2115536630461));
#54141=CARTESIAN_POINT('Ctrl Pts',(20.5902243197586,13.0703093182191,-37.3527980078731));
#54142=CARTESIAN_POINT('Ctrl Pts',(20.5902243197586,25.2115536630461,-12.141244344827));
#54143=CARTESIAN_POINT('Ctrl Pts',(20.5902243197586,37.3527980078731,13.0703093182191));
#54144=CARTESIAN_POINT('Ctrl Pts',(20.5902243197586,12.141244344827,25.2115536630461));
#54145=CARTESIAN_POINT('Ctrl Pts',(20.5902243197586,4.32421311009545,28.9760375001185));
#54146=CARTESIAN_POINT('Ctrl Pts',(20.5902243197586,-4.25132104313727,27.6578835367717));
#54147=CARTESIAN_POINT('Ctrl Pts',(19.591895069338,-4.30570507106198,28.011690528843));
#54148=CARTESIAN_POINT('Ctrl Pts',(19.591895069338,-19.0580773167089,25.7440885816178));
#54149=CARTESIAN_POINT('Ctrl Pts',(19.591895069338,-25.5340665536333,12.296558367172));
#54150=CARTESIAN_POINT('Ctrl Pts',(19.591895069338,-37.8306249208053,-13.2375081864613));
#54151=CARTESIAN_POINT('Ctrl Pts',(19.591895069338,-12.296558367172,-25.5340665536333));
#54152=CARTESIAN_POINT('Ctrl Pts',(19.591895069338,13.2375081864613,-37.8306249208053));
#54153=CARTESIAN_POINT('Ctrl Pts',(19.591895069338,25.5340665536333,-12.296558367172));
#54154=CARTESIAN_POINT('Ctrl Pts',(19.591895069338,37.8306249208053,13.2375081864613));
#54155=CARTESIAN_POINT('Ctrl Pts',(19.591895069338,12.296558367172,25.5340665536333));
#54156=CARTESIAN_POINT('Ctrl Pts',(19.591895069338,4.37952959270064,29.3467066677876));
#54157=CARTESIAN_POINT('Ctrl Pts',(19.591895069338,-4.30570507106198,28.011690528843));
#54158=CARTESIAN_POINT('Ctrl Pts',(18.5871162949016,-4.36721109149925,28.4118311751982));
#54159=CARTESIAN_POINT('Ctrl Pts',(18.5871162949016,-19.3303176289436,26.1118370484326));
#54160=CARTESIAN_POINT('Ctrl Pts',(18.5871162949016,-25.8988149034099,12.4722119146764));
#54161=CARTESIAN_POINT('Ctrl Pts',(18.5871162949016,-38.3710268180862,-13.4266029887335));
#54162=CARTESIAN_POINT('Ctrl Pts',(18.5871162949016,-12.4722119146764,-25.8988149034099));
#54163=CARTESIAN_POINT('Ctrl Pts',(18.5871162949016,13.4266029887335,-38.3710268180862));
#54164=CARTESIAN_POINT('Ctrl Pts',(18.5871162949016,25.8988149034099,-12.4722119146764));
#54165=CARTESIAN_POINT('Ctrl Pts',(18.5871162949016,38.3710268180862,13.4266029887335));
#54166=CARTESIAN_POINT('Ctrl Pts',(18.5871162949016,12.4722119146764,25.8988149034099));
#54167=CARTESIAN_POINT('Ctrl Pts',(18.5871162949016,4.44209017968666,29.7659177169156));
#54168=CARTESIAN_POINT('Ctrl Pts',(18.5871162949016,-4.36721109149925,28.4118311751982));
#54169=CARTESIAN_POINT('Ctrl Pts',(17.577868433379,-4.43610045989054,28.8600057798811));
#54170=CARTESIAN_POINT('Ctrl Pts',(17.577868433379,-19.6352383997424,26.5237310293085));
#54171=CARTESIAN_POINT('Ctrl Pts',(17.577868433379,-26.3073486251372,12.6689513859872));
#54172=CARTESIAN_POINT('Ctrl Pts',(17.577868433379,-38.9763000111244,-13.63839723915));
#54173=CARTESIAN_POINT('Ctrl Pts',(17.577868433379,-12.6689513859872,-26.3073486251372));
#54174=CARTESIAN_POINT('Ctrl Pts',(17.577868433379,13.63839723915,-38.9763000111244));
#54175=CARTESIAN_POINT('Ctrl Pts',(17.577868433379,26.3073486251372,-12.6689513859872));
#54176=CARTESIAN_POINT('Ctrl Pts',(17.577868433379,38.9763000111244,13.63839723915));
#54177=CARTESIAN_POINT('Ctrl Pts',(17.577868433379,12.6689513859872,26.3073486251372));
#54178=CARTESIAN_POINT('Ctrl Pts',(17.577868433379,4.51216070762872,30.2354519867605));
#54179=CARTESIAN_POINT('Ctrl Pts',(17.577868433379,-4.43610045989054,28.8600057798811));
#54180=CARTESIAN_POINT('Ctrl Pts',(16.5668667015923,-4.51259168970781,29.3576359292874));
#54181=CARTESIAN_POINT('Ctrl Pts',(16.5668667015923,-19.9738068218355,26.9810770304007));
#54182=CARTESIAN_POINT('Ctrl Pts',(16.5668667015923,-26.7609635664043,12.8874008284133));
#54183=CARTESIAN_POINT('Ctrl Pts',(16.5668667015923,-39.6483643948176,-13.873562737991));
#54184=CARTESIAN_POINT('Ctrl Pts',(16.5668667015923,-12.8874008284133,-26.7609635664043));
#54185=CARTESIAN_POINT('Ctrl Pts',(16.5668667015923,13.873562737991,-39.6483643948176));
#54186=CARTESIAN_POINT('Ctrl Pts',(16.5668667015923,26.7609635664043,-12.8874008284133));
#54187=CARTESIAN_POINT('Ctrl Pts',(16.5668667015923,39.6483643948176,13.873562737991));
#54188=CARTESIAN_POINT('Ctrl Pts',(16.5668667015923,12.8874008284133,26.7609635664043));
#54189=CARTESIAN_POINT('Ctrl Pts',(16.5668667015923,4.58996343657508,30.7567988154581));
#54190=CARTESIAN_POINT('Ctrl Pts',(16.5668667015923,-4.51259168970781,29.3576359292874));
#54191=CARTESIAN_POINT('Ctrl Pts',(15.5576189940876,-4.59680623544197,29.9055117717334));
#54192=CARTESIAN_POINT('Ctrl Pts',(15.5576189940876,-20.3465604817598,27.4846012359511));
#54193=CARTESIAN_POINT('Ctrl Pts',(15.5576189940876,-27.2603799871926,13.1279071008807));
#54194=CARTESIAN_POINT('Ctrl Pts',(15.5576189940876,-40.3882870880733,-14.1324728863119));
#54195=CARTESIAN_POINT('Ctrl Pts',(15.5576189940876,-13.1279071008807,-27.2603799871926));
#54196=CARTESIAN_POINT('Ctrl Pts',(15.5576189940876,14.1324728863119,-40.3882870880733));
#54197=CARTESIAN_POINT('Ctrl Pts',(15.5576189940876,27.2603799871926,-13.1279071008807));
#54198=CARTESIAN_POINT('Ctrl Pts',(15.5576189940876,40.3882870880733,14.1324728863119));
#54199=CARTESIAN_POINT('Ctrl Pts',(15.5576189940876,13.1279071008807,27.2603799871926));
#54200=CARTESIAN_POINT('Ctrl Pts',(15.5576189940876,4.67562190344439,31.3307860092005));
#54201=CARTESIAN_POINT('Ctrl Pts',(15.5576189940876,-4.59680623544197,29.9055117717334));
#54202=CARTESIAN_POINT('Ctrl Pts',(14.5544447688713,-4.68871703666209,30.503457259765));
#54203=CARTESIAN_POINT('Ctrl Pts',(14.5544447688713,-20.7533796035957,28.0341418498963));
#54204=CARTESIAN_POINT('Ctrl Pts',(14.5544447688713,-27.805437411382,13.3903929221629));
#54205=CARTESIAN_POINT('Ctrl Pts',(14.5544447688713,-41.1958303335449,-14.4150444892191));
#54206=CARTESIAN_POINT('Ctrl Pts',(14.5544447688713,-13.3903929221629,-27.805437411382));
#54207=CARTESIAN_POINT('Ctrl Pts',(14.5544447688713,14.4150444892191,-41.1958303335449));
#54208=CARTESIAN_POINT('Ctrl Pts',(14.5544447688713,27.805437411382,-13.3903929221629));
#54209=CARTESIAN_POINT('Ctrl Pts',(14.5544447688713,41.1958303335449,14.4150444892191));
#54210=CARTESIAN_POINT('Ctrl Pts',(14.5544447688713,13.3903929221629,27.805437411382));
#54211=CARTESIAN_POINT('Ctrl Pts',(14.5544447688713,4.76910858383447,31.9572291302439));
#54212=CARTESIAN_POINT('Ctrl Pts',(14.5544447688713,-4.68871703666209,30.503457259765));
#54213=CARTESIAN_POINT('Ctrl Pts',(13.5625963827217,-4.78806279521497,31.1497724620392));
#54214=CARTESIAN_POINT('Ctrl Pts',(13.5625963827217,-21.1931076194119,28.6281365537097));
#54215=CARTESIAN_POINT('Ctrl Pts',(13.5625963827217,-28.3945862659469,13.6741120572209));
#54216=CARTESIAN_POINT('Ctrl Pts',(13.5625963827217,-42.0686983231678,-14.720474208726));
#54217=CARTESIAN_POINT('Ctrl Pts',(13.5625963827217,-13.6741120572209,-28.3945862659469));
#54218=CARTESIAN_POINT('Ctrl Pts',(13.5625963827217,14.720474208726,-42.0686983231678));
#54219=CARTESIAN_POINT('Ctrl Pts',(13.5625963827217,28.3945862659469,-13.6741120572209));
#54220=CARTESIAN_POINT('Ctrl Pts',(13.5625963827217,42.0686983231678,14.720474208726));
#54221=CARTESIAN_POINT('Ctrl Pts',(13.5625963827217,13.6741120572209,28.3945862659469));
#54222=CARTESIAN_POINT('Ctrl Pts',(13.5625963827217,4.8701576994406,32.6343472297938));
#54223=CARTESIAN_POINT('Ctrl Pts',(13.5625963827217,-4.78806279521497,31.1497724620392));
#54224=CARTESIAN_POINT('Ctrl Pts',(12.5880795783847,-4.89434668936618,31.8412251978926));
#54225=CARTESIAN_POINT('Ctrl Pts',(12.5880795783847,-21.6635454777474,29.263614818168));
#54226=CARTESIAN_POINT('Ctrl Pts',(12.5880795783847,-29.0248802554437,13.9776456449495));
#54227=CARTESIAN_POINT('Ctrl Pts',(12.5880795783847,-43.0025259003932,-15.0472346104942));
#54228=CARTESIAN_POINT('Ctrl Pts',(12.5880795783847,-13.9776456449495,-29.0248802554437));
#54229=CARTESIAN_POINT('Ctrl Pts',(12.5880795783847,15.0472346104942,-43.0025259003932));
#54230=CARTESIAN_POINT('Ctrl Pts',(12.5880795783847,29.0248802554437,-13.9776456449495));
#54231=CARTESIAN_POINT('Ctrl Pts',(12.5880795783847,43.0025259003932,15.0472346104942));
#54232=CARTESIAN_POINT('Ctrl Pts',(12.5880795783847,13.9776456449495,29.0248802554437));
#54233=CARTESIAN_POINT('Ctrl Pts',(12.5880795783847,4.97826391014952,33.3587540838835));
#54234=CARTESIAN_POINT('Ctrl Pts',(12.5880795783847,-4.89434668936618,31.8412251978926));
#54235=CARTESIAN_POINT('Ctrl Pts',(11.6370973936883,-5.00694477063914,32.5737562362951));
#54236=CARTESIAN_POINT('Ctrl Pts',(11.6370973936883,-22.1619314338677,29.9368460150499));
#54237=CARTESIAN_POINT('Ctrl Pts',(11.6370973936883,-29.6926191863701,14.2992117660733));
#54238=CARTESIAN_POINT('Ctrl Pts',(11.6370973936883,-43.9918309524434,-15.3934074202968));
#54239=CARTESIAN_POINT('Ctrl Pts',(11.6370973936883,-14.2992117660733,-29.6926191863701));
#54240=CARTESIAN_POINT('Ctrl Pts',(11.6370973936883,15.3934074202968,-43.9918309524434));
#54241=CARTESIAN_POINT('Ctrl Pts',(11.6370973936883,29.6926191863701,-14.2992117660733));
#54242=CARTESIAN_POINT('Ctrl Pts',(11.6370973936883,43.9918309524434,15.3934074202968));
#54243=CARTESIAN_POINT('Ctrl Pts',(11.6370973936883,14.2992117660733,29.6926191863701));
#54244=CARTESIAN_POINT('Ctrl Pts',(11.6370973936883,5.09279256942311,34.1261970015792));
#54245=CARTESIAN_POINT('Ctrl Pts',(11.6370973936883,-5.00694477063914,32.5737562362951));
#54246=CARTESIAN_POINT('Ctrl Pts',(10.7155646400367,-5.12517843764354,33.3429507899297));
#54247=CARTESIAN_POINT('Ctrl Pts',(10.7155646400367,-22.6852618362104,30.6437727428344));
#54248=CARTESIAN_POINT('Ctrl Pts',(10.7155646400367,-30.3937787577631,14.6368724193901));
#54249=CARTESIAN_POINT('Ctrl Pts',(10.7155646400367,-45.0306511771533,-15.756906338373));
#54250=CARTESIAN_POINT('Ctrl Pts',(10.7155646400367,-14.6368724193901,-30.3937787577631));
#54251=CARTESIAN_POINT('Ctrl Pts',(10.7155646400367,15.756906338373,-45.0306511771533));
#54252=CARTESIAN_POINT('Ctrl Pts',(10.7155646400367,30.3937787577631,-14.6368724193901));
#54253=CARTESIAN_POINT('Ctrl Pts',(10.7155646400367,45.0306511771533,15.756906338373));
#54254=CARTESIAN_POINT('Ctrl Pts',(10.7155646400367,14.6368724193901,30.3937787577631));
#54255=CARTESIAN_POINT('Ctrl Pts',(10.7155646400367,5.21305344074461,34.9320507901155));
#54256=CARTESIAN_POINT('Ctrl Pts',(10.7155646400367,-5.12517843764354,33.3429507899297));
#54257=CARTESIAN_POINT('Ctrl Pts',(9.82859575068344,-5.24839106585011,34.1445370466763));
#54258=CARTESIAN_POINT('Ctrl Pts',(9.82859575068344,-23.2306303080404,31.3804690010715));
#54259=CARTESIAN_POINT('Ctrl Pts',(9.82859575068344,-31.1244649977519,14.9887523668806));
#54260=CARTESIAN_POINT('Ctrl Pts',(9.82859575068344,-46.1132173646325,-16.1357126308712));
#54261=CARTESIAN_POINT('Ctrl Pts',(9.82859575068344,-14.9887523668806,-31.1244649977519));
#54262=CARTESIAN_POINT('Ctrl Pts',(9.82859575068344,16.1357126308712,-46.1132173646325));
#54263=CARTESIAN_POINT('Ctrl Pts',(9.82859575068344,31.1244649977519,-14.9887523668806));
#54264=CARTESIAN_POINT('Ctrl Pts',(9.82859575068344,46.1132173646325,16.1357126308712));
#54265=CARTESIAN_POINT('Ctrl Pts',(9.82859575068344,14.9887523668806,31.1244649977519));
#54266=CARTESIAN_POINT('Ctrl Pts',(9.82859575068344,5.33837864126793,35.771840046014));
#54267=CARTESIAN_POINT('Ctrl Pts',(9.82859575068344,-5.24839106585011,34.1445370466763));
#54268=CARTESIAN_POINT('Ctrl Pts',(8.97989469943246,-5.37602105757972,34.9748614120298));
#54269=CARTESIAN_POINT('Ctrl Pts',(8.97989469943246,-23.7955510841199,32.1435769609828));
#54270=CARTESIAN_POINT('Ctrl Pts',(8.97989469943246,-31.8813474709538,15.3532477553949));
#54271=CARTESIAN_POINT('Ctrl Pts',(8.97989469943246,-47.2345952263487,-16.5280997155588));
#54272=CARTESIAN_POINT('Ctrl Pts',(8.97989469943246,-15.3532477553949,-31.8813474709538));
#54273=CARTESIAN_POINT('Ctrl Pts',(8.97989469943246,16.5280997155588,-47.2345952263487));
#54274=CARTESIAN_POINT('Ctrl Pts',(8.97989469943246,31.8813474709538,-15.3532477553949));
#54275=CARTESIAN_POINT('Ctrl Pts',(8.97989469943246,47.2345952263487,16.5280997155588));
#54276=CARTESIAN_POINT('Ctrl Pts',(8.97989469943246,15.3532477553949,31.8813474709538));
#54277=CARTESIAN_POINT('Ctrl Pts',(8.97989469943246,5.46819694430327,36.6417370471983));
#54278=CARTESIAN_POINT('Ctrl Pts',(8.97989469943246,-5.37602105757972,34.9748614120298));
#54279=CARTESIAN_POINT('Ctrl Pts',(8.1713316609345,-5.50765762249487,35.8312514010853));
#54280=CARTESIAN_POINT('Ctrl Pts',(8.1713316609345,-24.3782059084644,32.9306404806214));
#54281=CARTESIAN_POINT('Ctrl Pts',(8.1713316609345,-32.6619900727951,15.7291854188016));
#54282=CARTESIAN_POINT('Ctrl Pts',(8.1713316609345,-48.3911754915967,-16.9328046539935));
#54283=CARTESIAN_POINT('Ctrl Pts',(8.1713316609345,-15.7291854188016,-32.6619900727951));
#54284=CARTESIAN_POINT('Ctrl Pts',(8.1713316609345,16.9328046539935,-48.3911754915967));
#54285=CARTESIAN_POINT('Ctrl Pts',(8.1713316609345,32.6619900727951,-15.7291854188016));
#54286=CARTESIAN_POINT('Ctrl Pts',(8.1713316609345,48.3911754915967,16.9328046539935));
#54287=CARTESIAN_POINT('Ctrl Pts',(8.1713316609345,15.7291854188016,32.6619900727951));
#54288=CARTESIAN_POINT('Ctrl Pts',(8.1713316609345,5.60209051620674,37.5389419401399));
#54289=CARTESIAN_POINT('Ctrl Pts',(8.1713316609345,-5.50765762249487,35.8312514010853));
#54290=CARTESIAN_POINT('Ctrl Pts',(7.40358438374929,-5.64301551373697,36.7118512790457));
#54291=CARTESIAN_POINT('Ctrl Pts',(7.40358438374929,-24.9773322104622,33.739954050605));
#54292=CARTESIAN_POINT('Ctrl Pts',(7.40358438374929,-33.4647012075554,16.1157507275363));
#54293=CARTESIAN_POINT('Ctrl Pts',(7.40358438374929,-49.5804519350917,-17.348950480019));
#54294=CARTESIAN_POINT('Ctrl Pts',(7.40358438374929,-16.1157507275363,-33.4647012075554));
#54295=CARTESIAN_POINT('Ctrl Pts',(7.40358438374929,17.348950480019,-49.5804519350917));
#54296=CARTESIAN_POINT('Ctrl Pts',(7.40358438374929,33.4647012075554,-16.1157507275363));
#54297=CARTESIAN_POINT('Ctrl Pts',(7.40358438374929,49.5804519350917,17.348950480019));
#54298=CARTESIAN_POINT('Ctrl Pts',(7.40358438374929,16.1157507275363,33.4647012075554));
#54299=CARTESIAN_POINT('Ctrl Pts',(7.40358438374929,5.73976921934981,38.4615105471143));
#54300=CARTESIAN_POINT('Ctrl Pts',(7.40358438374929,-5.64301551373697,36.7118512790457));
#54301=CARTESIAN_POINT('Ctrl Pts',(6.82198164612729,-5.75413848390819,37.4347856648684));
#54302=CARTESIAN_POINT('Ctrl Pts',(6.82198164612729,-25.4691889731139,34.4043654629813));
#54303=CARTESIAN_POINT('Ctrl Pts',(6.82198164612729,-34.1236923063789,16.4331041147498));
#54304=CARTESIAN_POINT('Ctrl Pts',(6.82198164612729,-50.5567964211288,-17.6905881916291));
#54305=CARTESIAN_POINT('Ctrl Pts',(6.82198164612729,-16.4331041147498,-34.1236923063789));
#54306=CARTESIAN_POINT('Ctrl Pts',(6.82198164612729,17.6905881916291,-50.5567964211288));
#54307=CARTESIAN_POINT('Ctrl Pts',(6.82198164612729,34.1236923063789,-16.4331041147498));
#54308=CARTESIAN_POINT('Ctrl Pts',(6.82198164612729,50.5567964211288,17.6905881916291));
#54309=CARTESIAN_POINT('Ctrl Pts',(6.82198164612729,16.4331041147498,34.1236923063789));
#54310=CARTESIAN_POINT('Ctrl Pts',(6.82198164612729,5.85279747564271,39.2188994429737));
#54311=CARTESIAN_POINT('Ctrl Pts',(6.82198164612729,-5.75413848390819,37.4347856648684));
#54312=CARTESIAN_POINT('Ctrl Pts',(6.40395249919757,-5.83903695291963,37.9871109173118));
#54313=CARTESIAN_POINT('Ctrl Pts',(6.40395249919757,-25.8449698405413,34.9119788899584));
#54314=CARTESIAN_POINT('Ctrl Pts',(6.40395249919757,-34.627164588447,16.6755635870669));
#54315=CARTESIAN_POINT('Ctrl Pts',(6.40395249919757,-51.3027281755139,-17.9516010013801));
#54316=CARTESIAN_POINT('Ctrl Pts',(6.40395249919757,-16.6755635870669,-34.627164588447));
#54317=CARTESIAN_POINT('Ctrl Pts',(6.40395249919757,17.9516010013801,-51.3027281755139));
#54318=CARTESIAN_POINT('Ctrl Pts',(6.40395249919757,34.627164588447,-16.6755635870669));
#54319=CARTESIAN_POINT('Ctrl Pts',(6.40395249919757,51.3027281755139,17.9516010013801));
#54320=CARTESIAN_POINT('Ctrl Pts',(6.40395249919757,16.6755635870669,34.627164588447));
#54321=CARTESIAN_POINT('Ctrl Pts',(6.40395249919757,5.93915159216349,39.7975481022532));
#54322=CARTESIAN_POINT('Ctrl Pts',(6.40395249919757,-5.83903695291963,37.9871109173118));
#54323=CARTESIAN_POINT('Ctrl Pts',(6.13331019225912,-5.89632479122585,38.3598092724512));
#54324=CARTESIAN_POINT('Ctrl Pts',(6.13331019225912,-26.0985394728612,35.2545065735001));
#54325=CARTESIAN_POINT('Ctrl Pts',(6.13331019225912,-34.9668979078181,16.8391705308393));
#54326=CARTESIAN_POINT('Ctrl Pts',(6.13331019225912,-51.8060684386574,-18.1277273769788));
#54327=CARTESIAN_POINT('Ctrl Pts',(6.13331019225912,-16.8391705308393,-34.9668979078181));
#54328=CARTESIAN_POINT('Ctrl Pts',(6.13331019225912,18.1277273769788,-51.8060684386574));
#54329=CARTESIAN_POINT('Ctrl Pts',(6.13331019225912,34.9668979078181,-16.8391705308393));
#54330=CARTESIAN_POINT('Ctrl Pts',(6.13331019225912,51.8060684386574,18.1277273769788));
#54331=CARTESIAN_POINT('Ctrl Pts',(6.13331019225912,16.8391705308393,34.9668979078181));
#54332=CARTESIAN_POINT('Ctrl Pts',(6.13331019225912,5.99742167314282,40.1880089811702));
#54333=CARTESIAN_POINT('Ctrl Pts',(6.13331019225912,-5.89632479122585,38.3598092724512));
#54334=CARTESIAN_POINT('Ctrl Pts',(6.,-5.92514092475929,38.5472788277168));
#54335=CARTESIAN_POINT('Ctrl Pts',(6.,-26.2260865509321,35.4268000961685));
#54336=CARTESIAN_POINT('Ctrl Pts',(6.,-35.1377858481943,16.9214658255848));
#54337=CARTESIAN_POINT('Ctrl Pts',(6.,-52.0592516737791,-18.2163200226096));
#54338=CARTESIAN_POINT('Ctrl Pts',(6.,-16.9214658255848,-35.1377858481943));
#54339=CARTESIAN_POINT('Ctrl Pts',(6.,18.2163200226096,-52.0592516737791));
#54340=CARTESIAN_POINT('Ctrl Pts',(6.,35.1377858481943,-16.9214658255848));
#54341=CARTESIAN_POINT('Ctrl Pts',(6.,52.0592516737791,18.2163200226096));
#54342=CARTESIAN_POINT('Ctrl Pts',(6.,16.9214658255848,35.1377858481943));
#54343=CARTESIAN_POINT('Ctrl Pts',(6.,6.0267318807567,40.3844131946844));
#54344=CARTESIAN_POINT('Ctrl Pts',(6.,-5.92514092475929,38.5472788277168));
#54345=CARTESIAN_POINT('Ctrl Pts',(24.5,-4.10202091932642,26.6865776070557));
#54346=CARTESIAN_POINT('Ctrl Pts',(23.5178991898112,-7.02888984535001,26.4061954211995));
#54347=CARTESIAN_POINT('Ctrl Pts',(22.3947886245986,-9.85513676624463,25.7451296467846));
#54348=CARTESIAN_POINT('Ctrl Pts',(21.1743874927566,-12.5415350592883,24.8143683028972));
#54349=CARTESIAN_POINT('Ctrl Pts',(20.503187179342,-14.0190094152206,24.3024650528661));
#54350=CARTESIAN_POINT('Ctrl Pts',(19.841179296638,-15.459956153512,23.6888889491766));
#54351=CARTESIAN_POINT('Ctrl Pts',(19.1295827650217,-16.8492605460919,23.0263961974636));
#54352=CARTESIAN_POINT('Ctrl Pts',(18.8261415870883,-17.4416919909654,22.7438940041273));
#54353=CARTESIAN_POINT('Ctrl Pts',(18.5104994276256,-18.0296748698289,22.4504043480946));
#54354=CARTESIAN_POINT('Ctrl Pts',(18.2016639423759,-18.5741854933314,22.1732398894808));
#54355=CARTESIAN_POINT('Ctrl Pts',(17.6747132403639,-19.5032570185016,21.700327892593));
#54356=CARTESIAN_POINT('Ctrl Pts',(17.2016343371005,-20.3165166452584,21.2459677585646));
#54357=CARTESIAN_POINT('Ctrl Pts',(16.8729352926472,-20.8613715162025,20.9390355645018));
#54358=CARTESIAN_POINT('Ctrl Pts',(16.6342454025482,-21.2570262996894,20.7161520091495));
#54359=CARTESIAN_POINT('Ctrl Pts',(16.5014949770667,-21.4700011946069,20.5942515068562));
#54360=CARTESIAN_POINT('Ctrl Pts',(16.3424569562979,-21.7223849124751,20.4503534012052));
#54361=CARTESIAN_POINT('Ctrl Pts',(15.993118510103,-22.2767638931664,20.1342708670068));
#54362=CARTESIAN_POINT('Ctrl Pts',(15.6312480487537,-22.8249648575983,19.8204138910798));
#54363=CARTESIAN_POINT('Ctrl Pts',(15.2503296894305,-23.3683243655452,19.5222267532057));
#54364=CARTESIAN_POINT('Ctrl Pts',(14.7484414179076,-24.0842409329261,19.1293430195787));
#54365=CARTESIAN_POINT('Ctrl Pts',(14.2669345517206,-24.7693427603849,18.7403316609859));
#54366=CARTESIAN_POINT('Ctrl Pts',(13.7912435751455,-25.4155597055059,18.3952128404075));
#54367=CARTESIAN_POINT('Ctrl Pts',(13.5533980868579,-25.7386681780664,18.2226534301183));
#54368=CARTESIAN_POINT('Ctrl Pts',(13.3161115657262,-26.0538393629016,18.0600012158979));
#54369=CARTESIAN_POINT('Ctrl Pts',(13.0766514227367,-26.3632568545648,17.9105174192254));
#54370=CARTESIAN_POINT('Ctrl Pts',(12.9188702359555,-26.5671332008995,17.8120219846653));
#54371=CARTESIAN_POINT('Ctrl Pts',(12.7601526360409,-26.768518589267,17.7192419542993));
#54372=CARTESIAN_POINT('Ctrl Pts',(12.5997389313808,-26.9681145831351,17.6332028310594));
#54373=CARTESIAN_POINT('Ctrl Pts',(12.5166971934814,-27.0714399083852,17.5886627567788));
#54374=CARTESIAN_POINT('Ctrl Pts',(12.4397215765388,-27.1663492636317,17.5490685135353));
#54375=CARTESIAN_POINT('Ctrl Pts',(12.3478597934844,-27.2783220449005,17.5045441701774));
#54376=CARTESIAN_POINT('Ctrl Pts',(11.9116121727781,-27.810075923262,17.2930999960328));
#54377=CARTESIAN_POINT('Ctrl Pts',(10.7144663992386,-29.3032420783634,16.6461921152493));
#54378=CARTESIAN_POINT('Ctrl Pts',(9.56604185022482,-30.6013366128143,16.6022989798071));
#54379=CARTESIAN_POINT('Ctrl Pts',(9.07284645450887,-31.1588083667446,16.5834489018267));
#54380=CARTESIAN_POINT('Ctrl Pts',(8.57333454993011,-31.7021782420111,16.6574399322426));
#54381=CARTESIAN_POINT('Ctrl Pts',(8.00348148263448,-32.3497632212541,16.8141041993546));
#54382=CARTESIAN_POINT('Ctrl Pts',(7.63919428966211,-32.7637417147262,16.9142542018388));
#54383=CARTESIAN_POINT('Ctrl Pts',(7.24388644384739,-33.2272501674787,17.0569857758551));
#54384=CARTESIAN_POINT('Ctrl Pts',(6.94254646282505,-33.5948793104207,17.1798573054043));
#54385=CARTESIAN_POINT('Ctrl Pts',(6.91433564865247,-33.6292959762769,17.19136027914));
#54386=CARTESIAN_POINT('Ctrl Pts',(6.88669635040544,-33.6631407630316,17.2027579696588));
#54387=CARTESIAN_POINT('Ctrl Pts',(6.85962514029879,-33.6964076011753,17.2140339107427));
#54388=CARTESIAN_POINT('Ctrl Pts',(6.44000062073739,-34.2120691071963,17.3888196458955));
#54389=CARTESIAN_POINT('Ctrl Pts',(6.15412442492901,-34.5726334242706,17.569202218668));
#54390=CARTESIAN_POINT('Ctrl Pts',(6.,-34.7703877941326,17.6640916167698));
#54391=CARTESIAN_POINT('Ctrl Pts',(2.09999999999999,-8.34942492151724,5.01979576159902));
#54392=CARTESIAN_POINT('Ctrl Pts',(2.73333333333333,-8.34942492151724,5.01979576159902));
#54393=CARTESIAN_POINT('Ctrl Pts',(3.3670066960941,-8.34945762015934,5.01975070676219));
#54394=CARTESIAN_POINT('Ctrl Pts',(4.12581290128969,-8.3494675953969,5.01973710194472));
#54395=CARTESIAN_POINT('Ctrl Pts',(4.38277322768255,-8.35014527570449,5.01863624946971));
#54396=CARTESIAN_POINT('Ctrl Pts',(4.88873771935076,-8.35315509347545,5.01376061458228));
#54397=CARTESIAN_POINT('Ctrl Pts',(5.76578794114311,-8.36010835560182,5.00252538661004));
#54398=CARTESIAN_POINT('Ctrl Pts',(6.49297690404802,-8.36003126626443,5.00271709005476));
#54399=CARTESIAN_POINT('Ctrl Pts',(7.02338209451756,-8.34858381308083,5.02100940896465));
#54400=CARTESIAN_POINT('Ctrl Pts',(7.14976392682211,-8.3458231106267,5.02554405062937));
#54401=CARTESIAN_POINT('Ctrl Pts',(7.39959333012189,-8.3400478083999,5.03523386697765));
#54402=CARTESIAN_POINT('Ctrl Pts',(7.71338818747182,-8.33207879519409,5.04890883922946));
#54403=CARTESIAN_POINT('Ctrl Pts',(8.08764188214564,-8.32084794494089,5.0682031434201));
#54404=CARTESIAN_POINT('Ctrl Pts',(8.58206241785991,-8.30304111738429,5.09831422701953));
#54405=CARTESIAN_POINT('Ctrl Pts',(9.18588787679093,-8.27425997957743,5.14525139206092));
#54406=CARTESIAN_POINT('Ctrl Pts',(9.64255639534934,-8.24198331627265,5.19457168720712));
#54407=CARTESIAN_POINT('Ctrl Pts',(10.3692081392539,-8.17902467196105,5.28739536504009));
#54408=CARTESIAN_POINT('Ctrl Pts',(11.102425634648,-8.09134598482829,5.42279242355537));
#54409=CARTESIAN_POINT('Ctrl Pts',(12.0425787397489,-7.9415154745789,5.64100401523642));
#54410=CARTESIAN_POINT('Ctrl Pts',(12.4996155489097,-7.8577884580503,5.755174313772));
#54411=CARTESIAN_POINT('Ctrl Pts',(13.0011661172537,-7.76088369919287,5.88085533234623));
#54412=CARTESIAN_POINT('Ctrl Pts',(13.5006127767821,-7.65247605468804,6.01885415512814));
#54413=CARTESIAN_POINT('Ctrl Pts',(14.4710726589074,-7.40389754548305,6.32617356312799));
#54414=CARTESIAN_POINT('Ctrl Pts',(15.1518142252861,-7.19020489438465,6.56953458941686));
#54415=CARTESIAN_POINT('Ctrl Pts',(15.8845569213207,-6.9432966915507,6.82188773029062));
#54416=CARTESIAN_POINT('Ctrl Pts',(16.3869773989622,-6.75786173757531,7.00426968060754));
#54417=CARTESIAN_POINT('Ctrl Pts',(17.3639381354626,-6.3463779015774,7.38519896132104));
#54418=CARTESIAN_POINT('Ctrl Pts',(18.0500099547399,-6.00535000373466,7.66464608496521));
#54419=CARTESIAN_POINT('Ctrl Pts',(18.7841565036792,-5.62040929877534,7.94279021781233));
#54420=CARTESIAN_POINT('Ctrl Pts',(19.2876849505228,-5.33554933752951,8.13708078860648));
#54421=CARTESIAN_POINT('Ctrl Pts',(20.2707836182184,-4.71473834446341,8.52038703318919));
#54422=CARTESIAN_POINT('Ctrl Pts',(20.9685349513319,-4.21244438509208,8.77731094000538));
#54423=CARTESIAN_POINT('Ctrl Pts',(22.65695724953,-2.95889425175503,9.31010852249438));
#54424=CARTESIAN_POINT('Ctrl Pts',(23.7241254823866,-2.00510513613211,9.54811629512881));
#54425=CARTESIAN_POINT('Ctrl Pts',(24.6950729185821,-0.969169964574942,
9.66847864460699));
#54426=CARTESIAN_POINT('Ctrl Pts',(2.09999999999999,-10.8626263234642,6.23008976872817));
#54427=CARTESIAN_POINT('Ctrl Pts',(2.73333333333333,-10.8626263234642,6.23008976872817));
#54428=CARTESIAN_POINT('Ctrl Pts',(3.36712916604075,-10.8626687927181,6.23002867096587));
#54429=CARTESIAN_POINT('Ctrl Pts',(4.1260789328716,-10.8626816890499,6.23001031043174));
#54430=CARTESIAN_POINT('Ctrl Pts',(4.38494073854913,-10.8635280023923,6.22857030785887));
#54431=CARTESIAN_POINT('Ctrl Pts',(4.89216306342126,-10.867275319152,6.22221170294779));
#54432=CARTESIAN_POINT('Ctrl Pts',(5.76874066410185,-10.8759106709847,6.20759670771725));
#54433=CARTESIAN_POINT('Ctrl Pts',(6.48939227720775,-10.8757765578405,6.20791193263853));
#54434=CARTESIAN_POINT('Ctrl Pts',(7.01204180322129,-10.8617170555104,6.23144086586232));
#54435=CARTESIAN_POINT('Ctrl Pts',(7.13830270328599,-10.858292565369,6.23733581247022));
#54436=CARTESIAN_POINT('Ctrl Pts',(7.38677643126479,-10.8511579895149,6.24989080196436));
#54437=CARTESIAN_POINT('Ctrl Pts',(7.69896900751756,-10.8413202385665,6.26761040631564));
#54438=CARTESIAN_POINT('Ctrl Pts',(8.07060760210473,-10.8274748483276,6.29258196555194));
#54439=CARTESIAN_POINT('Ctrl Pts',(8.56092958329594,-10.8055382261151,6.33151268282151));
#54440=CARTESIAN_POINT('Ctrl Pts',(9.1581881055872,-10.7701032006638,6.39210343890159));
#54441=CARTESIAN_POINT('Ctrl Pts',(9.60781844770696,-10.7304229027369,6.45557012594851));
#54442=CARTESIAN_POINT('Ctrl Pts',(10.3209483006796,-10.6531647380277,6.57470987900924));
#54443=CARTESIAN_POINT('Ctrl Pts',(11.042581596335,-10.5456407687268,6.74887792887924));
#54444=CARTESIAN_POINT('Ctrl Pts',(11.9743268683783,-10.3604778566151,7.03151955961449));
#54445=CARTESIAN_POINT('Ctrl Pts',(12.4289046542735,-10.2564876869773,7.17994113381094));
#54446=CARTESIAN_POINT('Ctrl Pts',(12.9286907133014,-10.135786957015,7.34363551094295));
#54447=CARTESIAN_POINT('Ctrl Pts',(13.4199991602706,-10.0021283089252,7.52177847665784));
#54448=CARTESIAN_POINT('Ctrl Pts',(14.3833044564643,-9.69353871566837,7.92135052907318));
#54449=CARTESIAN_POINT('Ctrl Pts',(15.0608942658284,-9.42683427492701,8.23929021623871));
#54450=CARTESIAN_POINT('Ctrl Pts',(15.7927655637968,-9.11698148114171,8.57033742089244));
#54451=CARTESIAN_POINT('Ctrl Pts',(16.2911221408769,-8.88573333710061,8.80857545235014));
#54452=CARTESIAN_POINT('Ctrl Pts',(17.2659436260203,-8.36948997402069,9.30918082924326));
#54453=CARTESIAN_POINT('Ctrl Pts',(17.951042142688,-7.93971093348247,9.67818466313474));
#54454=CARTESIAN_POINT('Ctrl Pts',(18.6848541385476,-7.45311339013388,10.0467837622568));
#54455=CARTESIAN_POINT('Ctrl Pts',(19.1879800656874,-7.09344722076858,10.3048160303236));
#54456=CARTESIAN_POINT('Ctrl Pts',(20.1723051379962,-6.30654681482803,10.8163737020384));
#54457=CARTESIAN_POINT('Ctrl Pts',(20.8704406678443,-5.66794248076931,11.1616568826984));
#54458=CARTESIAN_POINT('Ctrl Pts',(22.5587575563567,-4.07186834192525,11.8828606633097));
#54459=CARTESIAN_POINT('Ctrl Pts',(23.6292145427077,-2.85110598151754,12.2186869038546));
#54460=CARTESIAN_POINT('Ctrl Pts',(24.6070641578141,-1.51514224511533,12.4047064442659));
#54461=CARTESIAN_POINT('Ctrl Pts',(2.09999999999999,-15.8890291273581,8.65067778298648));
#54462=CARTESIAN_POINT('Ctrl Pts',(2.73333333333333,-15.8890291273581,8.65067778298648));
#54463=CARTESIAN_POINT('Ctrl Pts',(3.3673825055222,-15.889104504075,8.65057089971265));
#54464=CARTESIAN_POINT('Ctrl Pts',(4.12662168526103,-15.889127309897,8.65053895855418));
#54465=CARTESIAN_POINT('Ctrl Pts',(4.38928798294562,-15.890318506566,8.64840599244989));
#54466=CARTESIAN_POINT('Ctrl Pts',(4.89902245014287,-15.8955560337698,8.63905247688287));
#54467=CARTESIAN_POINT('Ctrl Pts',(5.77467110216829,-15.907556286625,8.61768036781575));
#54468=CARTESIAN_POINT('Ctrl Pts',(6.48222349628015,-15.9072667853389,8.61834812915088));
#54469=CARTESIAN_POINT('Ctrl Pts',(6.98946452110265,-15.8882256758818,8.65185633792884));
#54470=CARTESIAN_POINT('Ctrl Pts',(7.11548589692682,-15.8834783966492,8.66046288514499));
#54471=CARTESIAN_POINT('Ctrl Pts',(7.36126941213412,-15.8736712461814,8.67865495699402));
#54472=CARTESIAN_POINT('Ctrl Pts',(7.67029367856112,-15.8601635892604,8.70433206734693));
#54473=CARTESIAN_POINT('Ctrl Pts',(8.0367725352429,-15.8412062817442,8.74042252484053));
#54474=CARTESIAN_POINT('Ctrl Pts',(8.51906506082345,-15.8112406517118,8.79654161635137));
#54475=CARTESIAN_POINT('Ctrl Pts',(9.10358944465605,-15.7629482177986,8.88355963695649));
#54476=CARTESIAN_POINT('Ctrl Pts',(9.5400123194474,-15.7091485978985,8.97402106211602));
#54477=CARTESIAN_POINT('Ctrl Pts',(10.2287355379469,-15.6048805966226,9.14286649421513));
#54478=CARTESIAN_POINT('Ctrl Pts',(10.9322921746061,-15.4596505450725,9.39125917852511));
#54479=CARTESIAN_POINT('Ctrl Pts',(11.8534554375931,-15.2053258424165,9.80087093771465));
#54480=CARTESIAN_POINT('Ctrl Pts',(12.3052690270545,-15.0613611618861,10.0173156165896));
#54481=CARTESIAN_POINT('Ctrl Pts',(12.8031307179637,-14.8935321735672,10.2567539515269));
#54482=CARTESIAN_POINT('Ctrl Pts',(13.2871710515135,-14.7104718569604,10.5140864129075));
#54483=CARTESIAN_POINT('Ctrl Pts',(14.2485990096974,-14.2816356908812,11.0997389287419));
#54484=CARTESIAN_POINT('Ctrl Pts',(14.9265639642419,-13.9085020645968,11.5682553472289));
#54485=CARTESIAN_POINT('Ctrl Pts',(15.65866299345,-13.4730533863241,12.0571400248602));
#54486=CARTESIAN_POINT('Ctrl Pts',(16.1598143108985,-13.1477831760047,12.4105209936867));
#54487=CARTESIAN_POINT('Ctrl Pts',(17.1407487388018,-12.417186963142,13.156067730112));
#54488=CARTESIAN_POINT('Ctrl Pts',(17.8295851905423,-11.8071773596292,13.7066920314026));
#54489=CARTESIAN_POINT('Ctrl Pts',(18.5645530783256,-11.1166259020156,14.2565922786745));
#54490=CARTESIAN_POINT('Ctrl Pts',(19.0747524351397,-10.6010291281585,14.6469875368371));
#54491=CARTESIAN_POINT('Ctrl Pts',(20.0668395729403,-9.47382018883457,15.4190563401778));
#54492=CARTESIAN_POINT('Ctrl Pts',(20.7687912462459,-8.55849044800405,15.9418324548243));
#54493=CARTESIAN_POINT('Ctrl Pts',(22.4600869487331,-6.27367162967554,17.0380712303253));
#54494=CARTESIAN_POINT('Ctrl Pts',(23.5475381170851,-4.49961958864046,17.5738159147105));
#54495=CARTESIAN_POINT('Ctrl Pts',(24.5367404413918,-2.55107090700389,17.8863800997173));
#54496=CARTESIAN_POINT('Ctrl Pts',(2.09999999999999,-24.6852340341725,12.8867068079385));
#54497=CARTESIAN_POINT('Ctrl Pts',(2.73333333333333,-24.6852340341725,12.8867068079385));
#54498=CARTESIAN_POINT('Ctrl Pts',(3.36791107159354,-24.6853317546275,12.8865652847935));
#54499=CARTESIAN_POINT('Ctrl Pts',(4.12768121430416,-24.6853606115858,12.8865243203323));
#54500=CARTESIAN_POINT('Ctrl Pts',(4.39701762154762,-24.6871752442854,12.8831353414075));
#54501=CARTESIAN_POINT('Ctrl Pts',(4.91113197063761,-24.6950582823475,12.8684563166808));
#54502=CARTESIAN_POINT('Ctrl Pts',(5.7852670703077,-24.7129251351602,12.8352991234043));
#54503=CARTESIAN_POINT('Ctrl Pts',(6.46978616647,-24.7121107535044,12.8370651611017));
#54504=CARTESIAN_POINT('Ctrl Pts',(6.95073559623754,-24.6851250729823,12.8864227095011));
#54505=CARTESIAN_POINT('Ctrl Pts',(7.07635357803357,-24.6780765591886,12.8997472234176));
#54506=CARTESIAN_POINT('Ctrl Pts',(7.31756522858531,-24.6637419516586,12.9274971155078));
#54507=CARTESIAN_POINT('Ctrl Pts',(7.62128632811344,-24.6440033147104,12.9667017603524));
#54508=CARTESIAN_POINT('Ctrl Pts',(7.97917793444992,-24.6164746134198,13.0214934233426));
#54509=CARTESIAN_POINT('Ctrl Pts',(8.44847277450474,-24.573120133392,13.1063538137385));
#54510=CARTESIAN_POINT('Ctrl Pts',(9.01312641813064,-24.5036098535915,13.2370812402565));
#54511=CARTESIAN_POINT('Ctrl Pts',(9.43134912688994,-24.4266874344919,13.3717464360822));
#54512=CARTESIAN_POINT('Ctrl Pts',(10.0907921620889,-24.2778927786545,13.6225041072927));
#54513=CARTESIAN_POINT('Ctrl Pts',(10.7834912876056,-24.0671198126597,14.000653890148));
#54514=CARTESIAN_POINT('Ctrl Pts',(11.7034370264027,-23.6895856203247,14.6371266646603));
#54515=CARTESIAN_POINT('Ctrl Pts',(12.1558473466704,-23.4745906089699,14.9746304906823));
#54516=CARTESIAN_POINT('Ctrl Pts',(12.6542419042604,-23.2234646468753,15.348225695834));
#54517=CARTESIAN_POINT('Ctrl Pts',(13.1437462399789,-22.9481397930833,15.7534255158228));
#54518=CARTESIAN_POINT('Ctrl Pts',(14.1171132883844,-22.2987829221682,16.6787955360184));
#54519=CARTESIAN_POINT('Ctrl Pts',(14.8016574873343,-21.7325476271127,17.4179925894728));
#54520=CARTESIAN_POINT('Ctrl Pts',(15.5357648414539,-21.0744403383711,18.1847988319859));
#54521=CARTESIAN_POINT('Ctrl Pts',(16.0483420510548,-20.573614508204,18.7509903067964));
#54522=CARTESIAN_POINT('Ctrl Pts',(17.0412063199226,-19.4551142828868,19.9339578481721));
#54523=CARTESIAN_POINT('Ctrl Pts',(17.7361485053828,-18.5215259268316,20.8054593492918));
#54524=CARTESIAN_POINT('Ctrl Pts',(18.4726929142883,-17.4699774150895,21.6714660034558));
#54525=CARTESIAN_POINT('Ctrl Pts',(18.9926305583918,-16.670868714932,22.2983785648451));
#54526=CARTESIAN_POINT('Ctrl Pts',(19.9931796161569,-14.9373133436789,23.5255394018631));
#54527=CARTESIAN_POINT('Ctrl Pts',(20.6988341590712,-13.5316346811608,24.355867966199));
#54528=CARTESIAN_POINT('Ctrl Pts',(22.3924759398877,-10.0329126621697,26.0975343019239));
#54529=CARTESIAN_POINT('Ctrl Pts',(23.4934655270119,-7.27758194603014,26.9751716398332));
#54530=CARTESIAN_POINT('Ctrl Pts',(24.4911063137788,-4.25357930705334,27.4974711076497));
#54531=CARTESIAN_POINT('Ctrl Pts',(2.09999999999999,-30.9682375390399,15.9124418257614));
#54532=CARTESIAN_POINT('Ctrl Pts',(2.73333333333333,-30.9682375390399,15.9124418257614));
#54533=CARTESIAN_POINT('Ctrl Pts',(3.36829025256733,-30.9683301024836,15.9123139194918));
#54534=CARTESIAN_POINT('Ctrl Pts',(4.1284374497986,-30.9683565622462,15.9122787049611));
#54535=CARTESIAN_POINT('Ctrl Pts',(4.40254535554455,-30.970634683707,15.9079545360157));
#54536=CARTESIAN_POINT('Ctrl Pts',(4.91974554141507,-30.9804441635442,15.8893934640385));
#54537=CARTESIAN_POINT('Ctrl Pts',(5.79291553961598,-31.0024795572307,15.8478635012422));
#54538=CARTESIAN_POINT('Ctrl Pts',(6.46068624857462,-31.0010953179064,15.8508078920142));
#54539=CARTESIAN_POINT('Ctrl Pts',(6.92365522593866,-30.9690910431221,15.9101265761794));
#54540=CARTESIAN_POINT('Ctrl Pts',(7.04900195729302,-30.9604102911096,15.9267985760767));
#54541=CARTESIAN_POINT('Ctrl Pts',(7.28711491876453,-30.9429667627173,15.9611199296699));
#54542=CARTESIAN_POINT('Ctrl Pts',(7.58730945500939,-30.9189356421462,16.009664909088));
#54543=CARTESIAN_POINT('Ctrl Pts',(7.93961085376542,-30.8855807484087,16.0772177527489));
#54544=CARTESIAN_POINT('Ctrl Pts',(8.40082290028868,-30.8331543630746,16.1816268564623));
#54545=CARTESIAN_POINT('Ctrl Pts',(8.95405999645022,-30.7493484525957,16.3418922694593));
#54546=CARTESIAN_POINT('Ctrl Pts',(9.36434284862748,-30.6565656105899,16.5069296423345));
#54547=CARTESIAN_POINT('Ctrl Pts',(10.0148884847374,-30.4761334632112,16.8160554392504));
#54548=CARTESIAN_POINT('Ctrl Pts',(10.7127408890464,-30.2155593319315,17.2928070606343));
#54549=CARTESIAN_POINT('Ctrl Pts',(11.6387343709689,-29.7461959624163,18.0977624082062));
#54550=CARTESIAN_POINT('Ctrl Pts',(12.0933688355602,-29.4791056966195,18.5237540722142));
#54551=CARTESIAN_POINT('Ctrl Pts',(12.5933202684205,-29.1674178905854,18.9946082520247));
#54552=CARTESIAN_POINT('Ctrl Pts',(13.0908862957948,-28.8211456765741,19.5128785502266));
#54553=CARTESIAN_POINT('Ctrl Pts',(14.0727349416798,-28.0083559361138,20.6876432051089));
#54554=CARTESIAN_POINT('Ctrl Pts',(14.7612267225558,-27.301134448208,21.6223765758924));
#54555=CARTESIAN_POINT('Ctrl Pts',(15.4964710430934,-26.4824736348807,22.5876620437275));
#54556=CARTESIAN_POINT('Ctrl Pts',(16.01484268476,-25.8522730655872,23.3090056830889));
#54557=CARTESIAN_POINT('Ctrl Pts',(17.0124740776252,-24.452781473862,24.804932045947));
#54558=CARTESIAN_POINT('Ctrl Pts',(17.709978366144,-23.2858793778611,25.9050193793247));
#54559=CARTESIAN_POINT('Ctrl Pts',(18.4472345601431,-21.9749509058657,26.9953458912914));
#54560=CARTESIAN_POINT('Ctrl Pts',(18.9707204797144,-20.9713314847816,27.7907154941331));
#54561=CARTESIAN_POINT('Ctrl Pts',(19.9739933044595,-18.8024955852929,29.3401330613107));
#54562=CARTESIAN_POINT('Ctrl Pts',(20.6810262896676,-17.0452285236267,30.3879138141395));
#54563=CARTESIAN_POINT('Ctrl Pts',(22.3757441673503,-12.6765752760488,32.5850201604799));
#54564=CARTESIAN_POINT('Ctrl Pts',(23.4815899075194,-9.21962042180251,33.7021663443025));
#54565=CARTESIAN_POINT('Ctrl Pts',(24.4815088739376,-5.42882719120685,34.3692550812891));
#54566=CARTESIAN_POINT('Ctrl Pts',(2.09999999999999,-34.7380396419603,17.7278828364551));
#54567=CARTESIAN_POINT('Ctrl Pts',(2.73333333333333,-34.7380396419603,17.7278828364551));
#54568=CARTESIAN_POINT('Ctrl Pts',(3.36851999241306,-34.7381248546768,17.7277694819828));
#54569=CARTESIAN_POINT('Ctrl Pts',(4.12889275411719,-34.7381485955713,17.7277395939778));
#54570=CARTESIAN_POINT('Ctrl Pts',(4.40586721403073,-34.740711327236,17.7228406337032));
#54571=CARTESIAN_POINT('Ctrl Pts',(4.92489733234861,-34.7516913871972,17.7019190689149));
#54572=CARTESIAN_POINT('Ctrl Pts',(5.79754727458879,-34.7762173055544,17.655387207618));
#54573=CARTESIAN_POINT('Ctrl Pts',(6.45512262940898,-34.7744373975726,17.6591456413559));
#54574=CARTESIAN_POINT('Ctrl Pts',(6.90770633030733,-34.7396306906666,17.7240081296612));
#54575=CARTESIAN_POINT('Ctrl Pts',(7.03289870960102,-34.7299741346044,17.7426817178056));
#54576=CARTESIAN_POINT('Ctrl Pts',(7.2692358301988,-34.710703785389,17.7808672202825));
#54577=CARTESIAN_POINT('Ctrl Pts',(7.56744238493173,-34.6841437259206,17.8349214307925));
#54578=CARTESIAN_POINT('Ctrl Pts',(7.91665003948323,-34.6473728595804,17.9099709368762));
#54579=CARTESIAN_POINT('Ctrl Pts',(8.37355692634873,-34.5896133218137,18.0258905306332));
#54580=CARTESIAN_POINT('Ctrl Pts',(8.92113358743038,-34.497360835933,18.203630160046));
#54581=CARTESIAN_POINT('Ctrl Pts',(9.32837987631535,-34.3949235995297,18.387182191653));
#54582=CARTESIAN_POINT('Ctrl Pts',(9.97672036625888,-34.1947703440345,18.7327763273445));
#54583=CARTESIAN_POINT('Ctrl Pts',(10.6788811821633,-33.9029132211185,19.2712416755063));
#54584=CARTESIAN_POINT('Ctrl Pts',(11.6082688528039,-33.3775438321155,20.1785876628404));
#54585=CARTESIAN_POINT('Ctrl Pts',(12.064154115784,-33.0788815748098,20.6580339412667));
#54586=CARTESIAN_POINT('Ctrl Pts',(12.5649503363404,-32.7306110340746,21.1874574525754));
#54587=CARTESIAN_POINT('Ctrl Pts',(13.0665664254018,-32.3410506220515,21.7744538722713));
#54588=CARTESIAN_POINT('Ctrl Pts',(14.0523375976892,-31.4297559210954,23.0989321907902));
#54589=CARTESIAN_POINT('Ctrl Pts',(14.7427637262042,-30.6376034884511,24.1509958186388));
#54590=CARTESIAN_POINT('Ctrl Pts',(15.4785695663788,-29.7223267263288,25.2352714327783));
#54591=CARTESIAN_POINT('Ctrl Pts',(15.9996419749169,-29.0143486465837,26.0495423163302));
#54592=CARTESIAN_POINT('Ctrl Pts',(16.9994926423133,-27.4461241825516,27.7327496384012));
#54593=CARTESIAN_POINT('Ctrl Pts',(17.6981566854513,-26.1390088681491,28.9697268515409));
#54594=CARTESIAN_POINT('Ctrl Pts',(18.4357083126267,-24.6721941391514,30.1943963087492));
#54595=CARTESIAN_POINT('Ctrl Pts',(18.9608160431014,-23.5458848553488,31.0904778020446));
#54596=CARTESIAN_POINT('Ctrl Pts',(19.9653367025609,-21.1158182718772,32.8326764201553));
#54597=CARTESIAN_POINT('Ctrl Pts',(20.6729356218039,-19.1474864936212,34.0105320904367));
#54598=CARTESIAN_POINT('Ctrl Pts',(22.3680176960418,-14.2564897842765,36.4800421305849));
#54599=CARTESIAN_POINT('Ctrl Pts',(23.4757593035169,-10.3789662309951,37.7398907431838));
#54600=CARTESIAN_POINT('Ctrl Pts',(24.4767076204831,-6.12845803691562,38.4932334964498));
#54601=CARTESIAN_POINT('',(3.2,-33.4762280926097,17.1202264205697));
#54602=CARTESIAN_POINT('Ctrl Pts',(3.2,-33.4762280926097,17.1202264205697));
#54603=CARTESIAN_POINT('Ctrl Pts',(3.4517402013188,-32.7757491074893,16.7828935203276));
#54604=CARTESIAN_POINT('Ctrl Pts',(3.71840125361074,-32.0670044206292,16.4415800679211));
#54605=CARTESIAN_POINT('Ctrl Pts',(4.,-31.3543250987725,16.098371795166));
#54606=CARTESIAN_POINT('Ctrl Pts',(4.6281648118965,-29.76454503797,15.3327740683972));
#54607=CARTESIAN_POINT('Ctrl Pts',(5.32582967091579,-28.2030205776301,14.5138750276624));
#54608=CARTESIAN_POINT('Ctrl Pts',(6.03866108102417,-26.7368640118942,13.813540492213));
#54609=CARTESIAN_POINT('Ctrl Pts',(6.32798218053302,-26.1417863769365,13.529291573118));
#54610=CARTESIAN_POINT('Ctrl Pts',(6.61604116736837,-25.5687234927156,13.2688968345931));
#54611=CARTESIAN_POINT('Ctrl Pts',(6.89476148100328,-25.0250506156583,13.0435011857835));
#54612=CARTESIAN_POINT('Ctrl Pts',(7.65522892881283,-23.5416799927312,12.4285260820233));
#54613=CARTESIAN_POINT('Ctrl Pts',(8.35226709346248,-22.324236812765,11.9709302842019));
#54614=CARTESIAN_POINT('Ctrl Pts',(8.78926323736241,-21.5755931674142,11.7167440120742));
#54615=CARTESIAN_POINT('Ctrl Pts',(8.9903195773824,-21.231151795529,11.5997961573375));
#54616=CARTESIAN_POINT('Ctrl Pts',(9.18275521977661,-20.9067416215901,11.4960100244497));
#54617=CARTESIAN_POINT('Ctrl Pts',(9.37496045779525,-20.5859767684872,11.4009959127837));
#54618=CARTESIAN_POINT('Ctrl Pts',(9.48075233102288,-20.4094242716606,11.3486991025623));
#54619=CARTESIAN_POINT('Ctrl Pts',(9.58626090804149,-20.2343663629071,11.2992238752517));
#54620=CARTESIAN_POINT('Ctrl Pts',(9.69257910363365,-20.0586675915761,11.2524282472449));
#54621=CARTESIAN_POINT('Ctrl Pts',(10.0319880468435,-19.4977689234922,11.1030384409171));
#54622=CARTESIAN_POINT('Ctrl Pts',(10.3788056741065,-18.9297317699116,10.9818572797184));
#54623=CARTESIAN_POINT('Ctrl Pts',(10.775684908382,-18.293043816953,10.8706700722781));
#54624=CARTESIAN_POINT('Ctrl Pts',(10.8890930404452,-18.1111104094671,10.8388983583255));
#54625=CARTESIAN_POINT('Ctrl Pts',(11.0576203523027,-17.8415364545336,10.7938699917916));
#54626=CARTESIAN_POINT('Ctrl Pts',(11.2725125495735,-17.5031160652737,10.743205792085));
#54627=CARTESIAN_POINT('Ctrl Pts',(11.5968279595283,-16.9923718471319,10.666743356936));
#54628=CARTESIAN_POINT('Ctrl Pts',(12.0255678844699,-16.3252314956296,10.5807340258753));
#54629=CARTESIAN_POINT('Ctrl Pts',(12.532035905153,-15.5782338255957,10.4832582458773));
#54630=CARTESIAN_POINT('Ctrl Pts',(13.0988763177502,-14.7421919627351,10.3741630827162));
#54631=CARTESIAN_POINT('Ctrl Pts',(13.7495416919435,-13.7918088264638,10.3061345330427));
#54632=CARTESIAN_POINT('Ctrl Pts',(14.4398764943048,-12.8279168306252,10.2524861844184));
#54633=CARTESIAN_POINT('Ctrl Pts',(14.7901814039645,-12.3387974969788,10.2252627562297));
#54634=CARTESIAN_POINT('Ctrl Pts',(15.1459546153433,-11.8554473457044,10.1996815666194));
#54635=CARTESIAN_POINT('Ctrl Pts',(15.4570717747561,-11.4475484046093,10.172636394889));
#54636=CARTESIAN_POINT('Ctrl Pts',(15.7998231403801,-10.9981745437756,10.1428412863143));
#54637=CARTESIAN_POINT('Ctrl Pts',(16.0676294489035,-10.6509242977906,10.1275228717851));
#54638=CARTESIAN_POINT('Ctrl Pts',(16.3615307965769,-10.2740380103256,10.1136303748));
#54639=CARTESIAN_POINT('Ctrl Pts',(17.0296616018229,-9.41725616592929,10.0820483311278));
#54640=CARTESIAN_POINT('Ctrl Pts',(17.708469187171,-8.56731901604727,10.0713433202013));
#54641=CARTESIAN_POINT('Ctrl Pts',(18.4207032016838,-7.74709961718816,10.0374944043974));
#54642=CARTESIAN_POINT('Ctrl Pts',(18.829864204215,-7.27590365533518,10.0180490310472));
#54643=CARTESIAN_POINT('Ctrl Pts',(19.2113759272667,-6.83961046405605,10.0084432606969));
#54644=CARTESIAN_POINT('Ctrl Pts',(19.5701113607413,-6.43357233649932,9.99980987752349));
#54645=CARTESIAN_POINT('Ctrl Pts',(20.1215476021908,-5.80942395846933,9.98653892649964));
#54646=CARTESIAN_POINT('Ctrl Pts',(20.6514912601844,-5.2096335262144,9.97986911023992));
#54647=CARTESIAN_POINT('Ctrl Pts',(21.3979544325339,-4.42881997131726,9.93555336802176));
#54648=CARTESIAN_POINT('Ctrl Pts',(21.8107631282077,-3.99701484401668,9.91104589810155));
#54649=CARTESIAN_POINT('Ctrl Pts',(22.3076315955347,-3.48531200858995,9.87811544659317));
#54650=CARTESIAN_POINT('Ctrl Pts',(22.8472772295095,-2.92572478971589,9.83107499415808));
#54651=CARTESIAN_POINT('Ctrl Pts',(23.39531365686,-2.35743671154887,9.78330312337762));
#54652=CARTESIAN_POINT('Ctrl Pts',(23.9608264583112,-1.76507493700295,9.72269270625968));
#54653=CARTESIAN_POINT('Ctrl Pts',(24.5,-1.17476144568584,9.64284209699151));
#54654=CARTESIAN_POINT('Ctrl Pts',(2.79760018324017,-34.323788098568,17.5283403962136));
#54655=CARTESIAN_POINT('Ctrl Pts',(2.93205031708964,-34.0415378530154,17.3923990295756));
#54656=CARTESIAN_POINT('Ctrl Pts',(3.06670609136326,-33.7589461720905,17.256290336237));
#54657=CARTESIAN_POINT('Ctrl Pts',(3.20141516237076,-33.4762861111748,17.1201484566269));
#54658=CARTESIAN_POINT('Origin',(2.9,0.,0.));
#54659=CARTESIAN_POINT('Origin',(3.2,0.,0.));
#54660=CARTESIAN_POINT('Ctrl Pts',(2.1,-3.03642085633519,9.25886571362628));
#54661=CARTESIAN_POINT('Ctrl Pts',(2.73333333333333,-3.03642085633519,9.25886571362628));
#54662=CARTESIAN_POINT('Ctrl Pts',(3.36632482220385,-3.03636324782149,9.25886783371596));
#54663=CARTESIAN_POINT('Ctrl Pts',(4.12418518571929,-3.03634585734704,9.25886838619587));
#54664=CARTESIAN_POINT('Ctrl Pts',(4.3679354222169,-3.03750909441903,9.25849938516288));
#54665=CARTESIAN_POINT('Ctrl Pts',(4.86516885517288,-3.0428301752989,9.25682122204924));
#54666=CARTESIAN_POINT('Ctrl Pts',(5.74559105590866,-3.05539972951126,9.25287204039704));
#54667=CARTESIAN_POINT('Ctrl Pts',(6.51837844974244,-3.05559735374805,9.25281197487748));
#54668=CARTESIAN_POINT('Ctrl Pts',(7.10311570597879,-3.03287937787994,9.25984104765318));
#54669=CARTESIAN_POINT('Ctrl Pts',(7.23027107330381,-3.02779222743327,9.26147721945095));
#54670=CARTESIAN_POINT('Ctrl Pts',(7.4249517464998,-3.01943994533289,9.26424638408617));
#54671=CARTESIAN_POINT('Ctrl Pts',(7.61952199938249,-3.01043015254996,9.2672995518291));
#54672=CARTESIAN_POINT('Ctrl Pts',(8.01076939155846,-2.99081944883794,9.27400592468884));
#54673=CARTESIAN_POINT('Ctrl Pts',(8.60083990938693,-2.95480250579294,9.28632103618811));
#54674=CARTESIAN_POINT('Ctrl Pts',(9.25155102115583,-2.89826302827223,9.30424679722698));
#54675=CARTESIAN_POINT('Ctrl Pts',(9.76267543705633,-2.83990837348766,9.321312567219));
#54676=CARTESIAN_POINT('Ctrl Pts',(10.014174227857,-2.80574940848282,9.33079238677905));
#54677=CARTESIAN_POINT('Ctrl Pts',(10.7177547943786,-2.70119653739831,9.35897042938336));
#54678=CARTESIAN_POINT('Ctrl Pts',(11.8208662239638,-2.46633392199916,9.42626642479173));
#54679=CARTESIAN_POINT('Ctrl Pts',(12.8080235224918,-2.17401434547732,9.49797242406731));
#54680=CARTESIAN_POINT('Ctrl Pts',(13.5604138129135,-1.94092109890682,9.54355781467911));
#54681=CARTESIAN_POINT('Ctrl Pts',(14.1415326282582,-1.74098713062143,9.58078876510701));
#54682=CARTESIAN_POINT('Ctrl Pts',(15.2007206633323,-1.31387162315598,9.6515367181008));
#54683=CARTESIAN_POINT('Ctrl Pts',(15.9284925857039,-0.969988518465284,
9.69257775062039));
#54684=CARTESIAN_POINT('Ctrl Pts',(16.6747535574971,-0.611827371798453,
9.71611760998629));
#54685=CARTESIAN_POINT('Ctrl Pts',(17.2497597626852,-0.315563297197225,
9.72974158816072));
#54686=CARTESIAN_POINT('Ctrl Pts',(18.2984383463456,0.287775723800367,9.73535495662825));
#54687=CARTESIAN_POINT('Ctrl Pts',(19.0236515282951,0.752799571120926,9.7093944714803));
#54688=CARTESIAN_POINT('Ctrl Pts',(19.7681804380506,1.23052258053206,9.65365157938199));
#54689=CARTESIAN_POINT('Ctrl Pts',(20.3331320101339,1.61226392856985,9.598203157932));
#54690=CARTESIAN_POINT('Ctrl Pts',(21.3722761216913,2.37000412517729,9.44736748792574));
#54691=CARTESIAN_POINT('Ctrl Pts',(22.0962297345818,2.93224573984147,9.28523329835205));
#54692=CARTESIAN_POINT('Ctrl Pts',(23.2302247323429,3.79027058202878,8.97091205690245));
#54693=CARTESIAN_POINT('Ctrl Pts',(23.8854423668127,4.30028496502052,8.73255554778861));
#54694=CARTESIAN_POINT('Ctrl Pts',(24.5000000001022,4.7944580651727,8.44852886727892));
#54695=CARTESIAN_POINT('Ctrl Pts',(2.1,-3.9674280119859,13.3378745796554));
#54696=CARTESIAN_POINT('Ctrl Pts',(2.73333333333334,-3.9674280119859,13.3378745796554));
#54697=CARTESIAN_POINT('Ctrl Pts',(3.36613139261334,-3.96736212926572,13.3378808260227));
#54698=CARTESIAN_POINT('Ctrl Pts',(4.12377368580981,-3.96734259158422,13.3378825752465));
#54699=CARTESIAN_POINT('Ctrl Pts',(4.36467137386139,-3.96900709328001,13.3374064013275));
#54700=CARTESIAN_POINT('Ctrl Pts',(4.8600155516962,-3.97665156700167,13.3352304723138));
#54701=CARTESIAN_POINT('Ctrl Pts',(5.74114572251817,-3.99476856002092,13.3300899277835));
#54702=CARTESIAN_POINT('Ctrl Pts',(6.5237150074899,-3.99519388303041,13.3299818397575));
#54703=CARTESIAN_POINT('Ctrl Pts',(7.12009244527277,-3.96202698639281,13.3392674770816));
#54704=CARTESIAN_POINT('Ctrl Pts',(7.24739585324286,-3.95469236122976,13.3414037080991));
#54705=CARTESIAN_POINT('Ctrl Pts',(7.44368077169637,-3.94259427005441,13.3450474937973));
#54706=CARTESIAN_POINT('Ctrl Pts',(7.63959476887961,-3.92955381947168,13.3490688516567));
#54707=CARTESIAN_POINT('Ctrl Pts',(8.03421163923334,-3.90113824280286,13.3579171972697));
#54708=CARTESIAN_POINT('Ctrl Pts',(8.63054470873523,-3.84890354226684,13.3741911829931));
#54709=CARTESIAN_POINT('Ctrl Pts',(9.29110836512143,-3.76667328277033,13.3977994858214));
#54710=CARTESIAN_POINT('Ctrl Pts',(9.81209593588223,-3.68156553543029,13.4201847887225));
#54711=CARTESIAN_POINT('Ctrl Pts',(10.0692696198173,-3.63164870785884,13.4325883482395));
#54712=CARTESIAN_POINT('Ctrl Pts',(10.7901202392243,-3.47870991632635,13.4694216078752));
#54713=CARTESIAN_POINT('Ctrl Pts',(11.91641837421,-3.13571689561405,13.5575476160895));
#54714=CARTESIAN_POINT('Ctrl Pts',(12.9133332403102,-2.71251888458363,13.6487541609417));
#54715=CARTESIAN_POINT('Ctrl Pts',(13.6697365991946,-2.3766290909733,13.7045556427394));
#54716=CARTESIAN_POINT('Ctrl Pts',(14.2631492845408,-2.08523598290125,13.750506108406));
#54717=CARTESIAN_POINT('Ctrl Pts',(15.3329180253697,-1.46723682092391,13.8346922664385));
#54718=CARTESIAN_POINT('Ctrl Pts',(16.0654005693691,-0.972621989855104,
13.8792388488393));
#54719=CARTESIAN_POINT('Ctrl Pts',(16.8131010844738,-0.459790126624247,
13.8977377982197));
#54720=CARTESIAN_POINT('Ctrl Pts',(17.3939180876432,-0.0325415261246532,
13.905223318781));
#54721=CARTESIAN_POINT('Ctrl Pts',(18.4451545927817,0.83183807171203,13.8877537393552));
#54722=CARTESIAN_POINT('Ctrl Pts',(19.1720400984934,1.49522468250933,13.8310899003084));
#54723=CARTESIAN_POINT('Ctrl Pts',(19.9173951349631,2.17510085402637,13.7308930222181));
#54724=CARTESIAN_POINT('Ctrl Pts',(20.4826309364167,2.71876059724247,13.6358544771289));
#54725=CARTESIAN_POINT('Ctrl Pts',(21.5194122431661,3.79340188359948,13.388510786001));
#54726=CARTESIAN_POINT('Ctrl Pts',(22.2433206777627,4.58878559274361,13.1334972537449));
#54727=CARTESIAN_POINT('Ctrl Pts',(23.3780690493382,5.80072380280333,12.6475690238019));
#54728=CARTESIAN_POINT('Ctrl Pts',(24.0312127056184,6.51778005882525,12.2868361640544));
#54729=CARTESIAN_POINT('Ctrl Pts',(24.6419825553303,7.20914878794909,11.8621651263229));
#54730=CARTESIAN_POINT('Ctrl Pts',(2.1,-6.13977804183754,22.8555619337232));
#54731=CARTESIAN_POINT('Ctrl Pts',(2.73333333333333,-6.13977804183754,22.8555619337232));
#54732=CARTESIAN_POINT('Ctrl Pts',(3.365653360318,-6.13958582290045,22.8555736551316));
#54733=CARTESIAN_POINT('Ctrl Pts',(4.12277939961604,-6.13952862263624,22.8555767795658));
#54734=CARTESIAN_POINT('Ctrl Pts',(4.35701675178739,-6.14231565013462,22.854858979794));
#54735=CARTESIAN_POINT('Ctrl Pts',(4.84796106875134,-6.15528607005645,22.8515379397375));
#54736=CARTESIAN_POINT('Ctrl Pts',(5.73069923341384,-6.18633589313978,22.8436124669418));
#54737=CARTESIAN_POINT('Ctrl Pts',(6.53615142020775,-6.18749861931354,22.8433054821354));
#54738=CARTESIAN_POINT('Ctrl Pts',(7.15941690945266,-6.12850524487919,22.858168796905));
#54739=CARTESIAN_POINT('Ctrl Pts',(7.28706050168627,-6.11590359601848,22.861475915022));
#54740=CARTESIAN_POINT('Ctrl Pts',(7.4870444530628,-6.09485029109773,22.8672064973101));
#54741=CARTESIAN_POINT('Ctrl Pts',(7.68604635674693,-6.07220014505125,22.8735294015587));
#54742=CARTESIAN_POINT('Ctrl Pts',(8.08839747562535,-6.02271325537101,22.8874888199869));
#54743=CARTESIAN_POINT('Ctrl Pts',(8.69897241247564,-5.93135368058952,22.9132453728314));
#54744=CARTESIAN_POINT('Ctrl Pts',(9.38147318650496,-5.78652324369514,22.9506361922822));
#54745=CARTESIAN_POINT('Ctrl Pts',(9.92347837816972,-5.63556090051135,22.986091535273));
#54746=CARTESIAN_POINT('Ctrl Pts',(10.1922189143493,-5.54658888375171,23.0057398011073));
#54747=CARTESIAN_POINT('Ctrl Pts',(10.9470029906827,-5.27303275877381,23.064114912156));
#54748=CARTESIAN_POINT('Ctrl Pts',(12.1071873865115,-4.66475748602104,23.2025540475673));
#54749=CARTESIAN_POINT('Ctrl Pts',(13.1093438615391,-3.93318930439982,23.3383945039618));
#54750=CARTESIAN_POINT('Ctrl Pts',(13.8683635369228,-3.35571311089366,23.4172941333814));
#54751=CARTESIAN_POINT('Ctrl Pts',(14.4658066929412,-2.84996101905094,23.4828359475912));
#54752=CARTESIAN_POINT('Ctrl Pts',(15.5292048935208,-1.79474291067229,23.596261658863));
#54753=CARTESIAN_POINT('Ctrl Pts',(16.2561263101303,-0.953642037383936,
23.6478267525734));
#54754=CARTESIAN_POINT('Ctrl Pts',(17.0018250896354,-0.0807357451548354,
23.6536420885738));
#54755=CARTESIAN_POINT('Ctrl Pts',(17.5709881811724,0.63849429415504,23.6465481777418));
#54756=CARTESIAN_POINT('Ctrl Pts',(18.6067936674288,2.09172765883662,23.5771001185496));
#54757=CARTESIAN_POINT('Ctrl Pts',(19.3243419048038,3.20806192731327,23.4509787255064));
#54758=CARTESIAN_POINT('Ctrl Pts',(20.0666595174772,4.35754559455055,23.2485161668225));
#54759=CARTESIAN_POINT('Ctrl Pts',(20.6167887455572,5.25952111571729,23.0664267245431));
#54760=CARTESIAN_POINT('Ctrl Pts',(21.6393774029147,7.05499561655517,22.6043830858133));
#54761=CARTESIAN_POINT('Ctrl Pts',(22.3554860515227,8.38662026867344,22.139813592925));
#54762=CARTESIAN_POINT('Ctrl Pts',(23.4867391132867,10.4237640547879,21.261199459697));
#54763=CARTESIAN_POINT('Ctrl Pts',(24.125337196037,11.6072194078008,20.6279190418669));
#54764=CARTESIAN_POINT('Ctrl Pts',(24.727756995987,12.7519254968117,19.8878182601865));
#54765=CARTESIAN_POINT('Ctrl Pts',(2.1,-8.31212807168918,32.3732492877911));
#54766=CARTESIAN_POINT('Ctrl Pts',(2.73333333333334,-8.31212807168918,32.3732492877911));
#54767=CARTESIAN_POINT('Ctrl Pts',(3.3651165217007,-8.31196521408208,32.3732548809116));
#54768=CARTESIAN_POINT('Ctrl Pts',(4.12171258497796,-8.31191956967934,32.373255625749));
#54769=CARTESIAN_POINT('Ctrl Pts',(4.34927314647352,-8.31575317642587,32.3723152953323));
#54770=CARTESIAN_POINT('Ctrl Pts',(4.83587777455348,-8.33390159830587,32.3678881761052));
#54771=CARTESIAN_POINT('Ctrl Pts',(5.72001511869128,-8.37798521810356,32.3571598115706));
#54772=CARTESIAN_POINT('Ctrl Pts',(6.54876817834788,-8.38086727009316,32.3564666313068));
#54773=CARTESIAN_POINT('Ctrl Pts',(7.19754786253593,-8.29309470443329,32.3775894934029));
#54774=CARTESIAN_POINT('Ctrl Pts',(7.32550632174358,-8.27518440760661,32.3820760814367));
#54775=CARTESIAN_POINT('Ctrl Pts',(7.52896484904414,-8.24473551321405,32.3899925863444));
#54776=CARTESIAN_POINT('Ctrl Pts',(7.73081920990065,-8.21207597448873,32.3987063856483));
#54777=CARTESIAN_POINT('Ctrl Pts',(8.14025197937804,-8.1404418280831,32.4180128546022));
#54778=CARTESIAN_POINT('Ctrl Pts',(8.76332110590288,-8.00782017521505,32.4537361641667));
#54779=CARTESIAN_POINT('Ctrl Pts',(9.46279421342106,-7.79614249898192,32.5057982306959));
#54780=CARTESIAN_POINT('Ctrl Pts',(10.0176607623637,-7.57530053425566,32.5550946973183));
#54781=CARTESIAN_POINT('Ctrl Pts',(10.2919185676042,-7.44544358684942,32.5823081235974));
#54782=CARTESIAN_POINT('Ctrl Pts',(11.0596890924163,-7.04744605634131,32.6628595055625));
#54783=CARTESIAN_POINT('Ctrl Pts',(12.2113652017898,-6.18519408845136,32.8488994631672));
#54784=CARTESIAN_POINT('Ctrl Pts',(13.2034569104159,-5.16113729306093,33.0272278258128));
#54785=CARTESIAN_POINT('Ctrl Pts',(13.9587908471046,-4.34811174973568,33.1287391841076));
#54786=CARTESIAN_POINT('Ctrl Pts',(14.5428233206545,-3.64944819484762,33.2119379485251));
#54787=CARTESIAN_POINT('Ctrl Pts',(15.5915789891506,-2.18333872119813,33.354588850131));
#54788=CARTESIAN_POINT('Ctrl Pts',(16.3123176996232,-1.00843242986031,33.4154605432175));
#54789=CARTESIAN_POINT('Ctrl Pts',(17.0563515829208,0.220802504435864,33.4113265350998));
#54790=CARTESIAN_POINT('Ctrl Pts',(17.6162737851969,1.21359139026907,33.3925683370578));
#54791=CARTESIAN_POINT('Ctrl Pts',(18.645166902744,3.2420318553855,33.2784109512797));
#54792=CARTESIAN_POINT('Ctrl Pts',(19.3594014713778,4.80559392504864,33.0891039142606));
#54793=CARTESIAN_POINT('Ctrl Pts',(20.1008953939689,6.42413294926228,32.7902804240861));
#54794=CARTESIAN_POINT('Ctrl Pts',(20.6466151397584,7.67767483344647,32.5272511447639));
#54795=CARTESIAN_POINT('Ctrl Pts',(21.6663777991218,10.1933701488225,31.8609543508366));
#54796=CARTESIAN_POINT('Ctrl Pts',(22.3810344430405,12.0629280929144,31.194399788557));
#54797=CARTESIAN_POINT('Ctrl Pts',(23.5117469294374,14.9301557887008,29.9342669882141));
#54798=CARTESIAN_POINT('Ctrl Pts',(24.1480627906507,16.5833947234935,29.0351406353916));
#54799=CARTESIAN_POINT('Ctrl Pts',(24.7493903499091,18.1865024531276,27.9850142240257));
#54800=CARTESIAN_POINT('Ctrl Pts',(2.1,-9.55347094589012,37.8119277758299));
#54801=CARTESIAN_POINT('Ctrl Pts',(2.73333333333333,-9.55347094589012,37.8119277758299));
#54802=CARTESIAN_POINT('Ctrl Pts',(3.36479086716999,-9.55332620888327,37.8119309402221));
#54803=CARTESIAN_POINT('Ctrl Pts',(4.12108065676893,-9.55328738573655,37.8119307163399));
#54804=CARTESIAN_POINT('Ctrl Pts',(4.3448181830341,-9.55769178776168,37.8108695150359));
#54805=CARTESIAN_POINT('Ctrl Pts',(4.82897857397213,-9.57873699892895,37.8058249605254));
#54806=CARTESIAN_POINT('Ctrl Pts',(5.7138061276864,-9.63030673302427,37.7934862692131));
#54807=CARTESIAN_POINT('Ctrl Pts',(6.55611484843184,-9.63436371607534,37.7925312363998));
#54808=CARTESIAN_POINT('Ctrl Pts',(7.21874443048418,-9.52930083738139,37.8174231056462));
#54809=CARTESIAN_POINT('Ctrl Pts',(7.34686974636372,-9.50834537407352,37.8225859538797));
#54810=CARTESIAN_POINT('Ctrl Pts',(7.55219545109428,-9.47240667129618,37.8317783930218));
#54811=CARTESIAN_POINT('Ctrl Pts',(7.75555860205759,-9.43392187323299,37.8418815248632));
#54812=CARTESIAN_POINT('Ctrl Pts',(8.16870204156915,-9.34936587598233,37.8643012012295));
#54813=CARTESIAN_POINT('Ctrl Pts',(8.79805949449897,-9.19266019289524,37.905829016536));
#54814=CARTESIAN_POINT('Ctrl Pts',(9.50503273203101,-8.94227483367107,37.9663720914973));
#54815=CARTESIAN_POINT('Ctrl Pts',(10.0644372381433,-8.68184358810197,38.0234930381843));
#54816=CARTESIAN_POINT('Ctrl Pts',(10.3401591124554,-8.52923778582887,38.0548984873651));
#54817=CARTESIAN_POINT('Ctrl Pts',(11.1103063578917,-8.06278464620136,38.1475814285387));
#54818=CARTESIAN_POINT('Ctrl Pts',(12.254581323623,-7.06313343123591,38.3594886709139));
#54819=CARTESIAN_POINT('Ctrl Pts',(13.2428739922751,-5.87394568173444,38.5622360887224));
#54820=CARTESIAN_POINT('Ctrl Pts',(13.9964028454091,-4.92726867958817,38.6768476218439));
#54821=CARTESIAN_POINT('Ctrl Pts',(14.5753784070292,-4.12028262080844,38.7702148495551));
#54822=CARTESIAN_POINT('Ctrl Pts',(15.6192587771561,-2.41889470565338,38.9302475922307));
#54823=CARTESIAN_POINT('Ctrl Pts',(16.3373897865161,-1.05306307057831,38.9969282755714));
#54824=CARTESIAN_POINT('Ctrl Pts',(17.0806184187258,0.379671476043331,38.987618323965));
#54825=CARTESIAN_POINT('Ctrl Pts',(17.6369976627039,1.53007193924879,38.9625497856577));
#54826=CARTESIAN_POINT('Ctrl Pts',(18.6627888667656,3.88910869530589,38.8233284163515));
#54827=CARTESIAN_POINT('Ctrl Pts',(19.3754497970284,5.70863796723174,38.5983466101282));
#54828=CARTESIAN_POINT('Ctrl Pts',(20.1166099111039,7.59519646062446,38.2449529383188));
#54829=CARTESIAN_POINT('Ctrl Pts',(20.6599925696541,9.05087668442584,37.9357680733157));
#54830=CARTESIAN_POINT('Ctrl Pts',(21.6777820692419,11.9791501652495,37.152965907212));
#54831=CARTESIAN_POINT('Ctrl Pts',(22.3917974672498,14.1564098065562,36.3714296771662));
#54832=CARTESIAN_POINT('Ctrl Pts',(23.5225006119247,17.4981794009821,34.8939592200085));
#54833=CARTESIAN_POINT('Ctrl Pts',(24.157514841919,19.4205715247346,33.8431819361365));
#54834=CARTESIAN_POINT('Ctrl Pts',(24.7577717974218,21.2859250779863,32.6159836188887));
#54835=CARTESIAN_POINT('',(24.5,4.79445806514251,8.44852886740476));
#54836=CARTESIAN_POINT('Ctrl Pts',(24.5,4.79445806514251,8.44852886740476));
#54837=CARTESIAN_POINT('Ctrl Pts',(23.8274939346094,4.35568028974841,8.91358816488541));
#54838=CARTESIAN_POINT('Ctrl Pts',(23.3366347313997,4.04378531189072,9.23377527570042));
#54839=CARTESIAN_POINT('Ctrl Pts',(22.5855494187791,3.55891095582593,9.72812650348976));
#54840=CARTESIAN_POINT('Ctrl Pts',(22.2454144274676,3.33933172545618,9.95199741101992));
#54841=CARTESIAN_POINT('Ctrl Pts',(21.8382660749528,3.06477302734464,10.2233469033816));
#54842=CARTESIAN_POINT('Ctrl Pts',(21.3802156956953,2.74923897182448,10.5336111540776));
#54843=CARTESIAN_POINT('Ctrl Pts',(20.7694693297252,2.32851826843566,10.9473053069133));
#54844=CARTESIAN_POINT('Ctrl Pts',(20.1629003035507,1.90499719987852,11.3653835171637));
#54845=CARTESIAN_POINT('Ctrl Pts',(19.5574857571565,1.50134669736388,11.8035248325835));
#54846=CARTESIAN_POINT('Ctrl Pts',(18.641852941928,0.890863106926371,12.4661725480953));
#54847=CARTESIAN_POINT('Ctrl Pts',(17.7734813326701,0.243584198973207,13.1563618703622));
#54848=CARTESIAN_POINT('Ctrl Pts',(16.962125311809,-0.331821443170173,13.8621101827577));
#54849=CARTESIAN_POINT('Ctrl Pts',(16.8133360674514,-0.437341299426043,
13.9915327240442));
#54850=CARTESIAN_POINT('Ctrl Pts',(16.6656205372049,-0.541439795542996,
14.1222413658163));
#54851=CARTESIAN_POINT('Ctrl Pts',(16.5183901926363,-0.644331843442893,
14.2548376268699));
#54852=CARTESIAN_POINT('Ctrl Pts',(15.7264522885918,-1.19777830174949,14.9680601990961));
#54853=CARTESIAN_POINT('Ctrl Pts',(14.9462259717254,-1.80687549737941,15.7377680928373));
#54854=CARTESIAN_POINT('Ctrl Pts',(14.2963150412586,-2.29120527971764,16.427159456152));
#54855=CARTESIAN_POINT('Ctrl Pts',(13.9908350932594,-2.51885653127744,16.7511965325329));
#54856=CARTESIAN_POINT('Ctrl Pts',(13.7077063566188,-2.72603668208911,17.0631221045243));
#54857=CARTESIAN_POINT('Ctrl Pts',(13.4460198946299,-2.912853579393,17.3603809857102));
#54858=CARTESIAN_POINT('Ctrl Pts',(12.8373295399365,-3.34739513961885,18.0518138265595));
#54859=CARTESIAN_POINT('Ctrl Pts',(12.3530827399975,-3.71561728956872,18.6436933223557));
#54860=CARTESIAN_POINT('Ctrl Pts',(11.9770275677491,-3.99381285826312,19.1192007097534));
#54861=CARTESIAN_POINT('Ctrl Pts',(11.6553972423526,-4.2317463794219,19.5258899591599));
#54862=CARTESIAN_POINT('Ctrl Pts',(11.368420561198,-4.44137691516221,19.9029426948744));
#54863=CARTESIAN_POINT('Ctrl Pts',(11.0710856780973,-4.65123335112424,20.3088271733505));
#54864=CARTESIAN_POINT('Ctrl Pts',(10.8141787015422,-4.83255611390069,20.6595245187428));
#54865=CARTESIAN_POINT('Ctrl Pts',(10.5576802661712,-5.00811817493636,21.0215354696975));
#54866=CARTESIAN_POINT('Ctrl Pts',(10.2957959918397,-5.17851079664651,21.4059609250791));
#54867=CARTESIAN_POINT('Ctrl Pts',(9.71459276345219,-5.55666539216075,22.2591214148127));
#54868=CARTESIAN_POINT('Ctrl Pts',(9.09527967376231,-5.92026467566564,23.2374837564195));
#54869=CARTESIAN_POINT('Ctrl Pts',(8.43168033652699,-6.29835966306905,24.399171350721));
#54870=CARTESIAN_POINT('Ctrl Pts',(7.97964340480278,-6.55591401614932,25.1905007964946));
#54871=CARTESIAN_POINT('Ctrl Pts',(7.52291961074439,-6.81145492791075,26.0436998588172));
#54872=CARTESIAN_POINT('Ctrl Pts',(7.10363554125516,-7.05116144768124,26.8754977861791));
#54873=CARTESIAN_POINT('Ctrl Pts',(6.5632779955574,-7.36008619855196,27.9474876833705));
#54874=CARTESIAN_POINT('Ctrl Pts',(6.08559840023997,-7.60156228988461,28.9826246131377));
#54875=CARTESIAN_POINT('Ctrl Pts',(5.61708670830474,-7.83933188747728,30.0695190297804));
#54876=CARTESIAN_POINT('Ctrl Pts',(5.04102956504787,-8.13168078185986,31.4059067943778));
#54877=CARTESIAN_POINT('Ctrl Pts',(4.50102820503747,-8.40458357383467,32.7783233096991));
#54878=CARTESIAN_POINT('Ctrl Pts',(4.,-8.71775829923914,34.1504314334527));
#54879=CARTESIAN_POINT('Ctrl Pts',(3.72183418897114,-8.89162975120532,34.9122120382685));
#54880=CARTESIAN_POINT('Ctrl Pts',(3.45538353518229,-9.06631722055977,35.6775678488616));
#54881=CARTESIAN_POINT('Ctrl Pts',(3.2,-9.24182505978395,36.4465179346992));
#54882=CARTESIAN_POINT('',(24.5,14.1269463268952,23.0093326169409));
#54883=CARTESIAN_POINT('Ctrl Pts',(24.5,14.1269463268952,23.0093326169409));
#54884=CARTESIAN_POINT('Ctrl Pts',(24.5,13.4659464214661,21.9617493509785));
#54885=CARTESIAN_POINT('Ctrl Pts',(24.5,12.8153888814878,20.9324081809094));
#54886=CARTESIAN_POINT('Ctrl Pts',(24.5,10.1230771830749,16.6815116258866));
#54887=CARTESIAN_POINT('Ctrl Pts',(24.5,7.25732475029689,12.1733125527324));
#54888=CARTESIAN_POINT('Ctrl Pts',(24.5,4.79445806514251,8.44852886740475));
#54889=CARTESIAN_POINT('',(10.2670750393577,-7.59968099677391,33.2963779888109));
#54890=CARTESIAN_POINT('Ctrl Pts',(10.2670750393577,-7.59968099677391,33.2963779888109));
#54891=CARTESIAN_POINT('Ctrl Pts',(11.2293198185888,-6.94998678548836,32.5415114357085));
#54892=CARTESIAN_POINT('Ctrl Pts',(12.092802582344,-6.1285541721914,32.0055482292145));
#54893=CARTESIAN_POINT('Ctrl Pts',(14.3080979519049,-3.73267662114747,30.7914887306174));
#54894=CARTESIAN_POINT('Ctrl Pts',(14.8952017874601,-3.00279024948747,30.5262846241022));
#54895=CARTESIAN_POINT('Ctrl Pts',(17.0803363586062,0.164443307829025,29.4613521690468));
#54896=CARTESIAN_POINT('Ctrl Pts',(17.6922811489506,1.12977118340571,29.1445663219268));
#54897=CARTESIAN_POINT('Ctrl Pts',(19.0755427322033,3.49373927319035,28.3603783727572));
#54898=CARTESIAN_POINT('Ctrl Pts',(20.2687424742408,5.60613398516095,27.6263721986722));
#54899=CARTESIAN_POINT('Ctrl Pts',(22.3267279388309,9.72640384774287,25.7483075490095));
#54900=CARTESIAN_POINT('Ctrl Pts',(23.4192562717209,11.8964803423963,24.5951094752949));
#54901=CARTESIAN_POINT('Ctrl Pts',(24.5,14.1269463268952,23.0093326169409));
#54902=CARTESIAN_POINT('Ctrl Pts',(6.,-9.62277221548328,37.7942092772018));
#54903=CARTESIAN_POINT('Ctrl Pts',(7.51604047332548,-9.13953643716897,35.6914341219625));
#54904=CARTESIAN_POINT('Ctrl Pts',(9.08449301626627,-8.31972209498318,34.2861963730775));
#54905=CARTESIAN_POINT('Ctrl Pts',(9.8624969752411,-7.86293097600567,33.6206016235852));
#54906=CARTESIAN_POINT('Ctrl Pts',(10.0667253012217,-7.73495433668603,33.4535493442768));
#54907=CARTESIAN_POINT('Ctrl Pts',(10.2670750393577,-7.59968099677391,33.2963779888109));
#54908=CARTESIAN_POINT('Origin',(24.5,-1.89142793862867,8.2868872535455));
#54909=CARTESIAN_POINT('',(24.5,6.80662575089405,6.93067919103514));
#54910=CARTESIAN_POINT('Ctrl Pts',(24.5,6.80662575089405,6.93067919103514));
#54911=CARTESIAN_POINT('Ctrl Pts',(24.5,6.60260497657294,7.13104816180033));
#54912=CARTESIAN_POINT('Ctrl Pts',(24.5,6.38964036397032,7.322503105027));
#54913=CARTESIAN_POINT('Ctrl Pts',(24.5,5.7372524804206,7.85873653774361));
#54914=CARTESIAN_POINT('Ctrl Pts',(24.5,5.27749333642741,8.17441104304659));
#54915=CARTESIAN_POINT('Ctrl Pts',(24.5,4.79445806514251,8.44852886740476));
#54916=CARTESIAN_POINT('',(24.5,18.3068383223113,19.8458980809827));
#54917=CARTESIAN_POINT('Ctrl Pts',(24.5,6.80662575089405,6.93067919103514));
#54918=CARTESIAN_POINT('Ctrl Pts',(24.5,9.62249333717013,10.1909289822772));
#54919=CARTESIAN_POINT('Ctrl Pts',(24.5,13.4561052459601,14.4744049170257));
#54920=CARTESIAN_POINT('Ctrl Pts',(24.5,18.3068383223113,19.8458980809827));
#54921=CARTESIAN_POINT('Origin',(24.5,0.,0.));
#54922=CARTESIAN_POINT('Ctrl Pts',(24.5,18.3068385298747,19.845897889516));
#54923=CARTESIAN_POINT('Ctrl Pts',(24.5,7.85498547538757,29.4872044845456));
#54924=CARTESIAN_POINT('Ctrl Pts',(24.5,-6.00806521682049,26.3230536289092));
#54925=CARTESIAN_POINT('Ctrl Pts',(24.5,-32.3311188457297,20.3149884120888));
#54926=CARTESIAN_POINT('Ctrl Pts',(24.5,-26.3230536289092,-6.00806521682049));
#54927=CARTESIAN_POINT('Ctrl Pts',(24.5,-20.3149884120888,-32.3311188457297));
#54928=CARTESIAN_POINT('Ctrl Pts',(24.5,6.00806521682049,-26.3230536289092));
#54929=CARTESIAN_POINT('Ctrl Pts',(24.5,32.3311188457297,-20.3149884120888));
#54930=CARTESIAN_POINT('Ctrl Pts',(24.5,26.3230536289092,6.00806521682049));
#54931=CARTESIAN_POINT('Ctrl Pts',(24.5,24.4602079634702,14.1697253493454));
#54932=CARTESIAN_POINT('Ctrl Pts',(24.5,18.3068385298747,19.845897889516));
#54933=CARTESIAN_POINT('Ctrl Pts',(24.3078118955742,18.3290687603783,19.8699970196806));
#54934=CARTESIAN_POINT('Ctrl Pts',(24.3078118955742,7.86452388571633,29.5230111778492));
#54935=CARTESIAN_POINT('Ctrl Pts',(24.3078118955742,-6.01536088802186,26.3550180529563));
#54936=CARTESIAN_POINT('Ctrl Pts',(24.3078118955742,-32.3703789409781,20.3396571649344));
#54937=CARTESIAN_POINT('Ctrl Pts',(24.3078118955742,-26.3550180529563,-6.01536088802186));
#54938=CARTESIAN_POINT('Ctrl Pts',(24.3078118955742,-20.3396571649344,-32.3703789409781));
#54939=CARTESIAN_POINT('Ctrl Pts',(24.3078118955742,6.01536088802186,-26.3550180529563));
#54940=CARTESIAN_POINT('Ctrl Pts',(24.3078118955742,32.3703789409781,-20.3396571649344));
#54941=CARTESIAN_POINT('Ctrl Pts',(24.3078118955742,26.3550180529563,6.01536088802186));
#54942=CARTESIAN_POINT('Ctrl Pts',(24.3078118955742,24.4899103099625,14.1869318298732));
#54943=CARTESIAN_POINT('Ctrl Pts',(24.3078118955742,18.3290687603783,19.8699970196806));
#54944=CARTESIAN_POINT('Ctrl Pts',(23.9225830034177,18.376353041482,19.9212564991933));
#54945=CARTESIAN_POINT('Ctrl Pts',(23.9225830034177,7.88481233370136,29.5991729500489));
#54946=CARTESIAN_POINT('Ctrl Pts',(23.9225830034177,-6.03087897128555,26.4230072180579));
#54947=CARTESIAN_POINT('Ctrl Pts',(23.9225830034177,-32.4538861893435,20.3921282467724));
#54948=CARTESIAN_POINT('Ctrl Pts',(23.9225830034177,-26.4230072180579,-6.03087897128555));
#54949=CARTESIAN_POINT('Ctrl Pts',(23.9225830034177,-20.3921282467724,-32.4538861893435));
#54950=CARTESIAN_POINT('Ctrl Pts',(23.9225830034177,6.03087897128555,-26.4230072180579));
#54951=CARTESIAN_POINT('Ctrl Pts',(23.9225830034177,32.4538861893435,-20.3921282467724));
#54952=CARTESIAN_POINT('Ctrl Pts',(23.9225830034177,26.4230072180579,6.03087897128555));
#54953=CARTESIAN_POINT('Ctrl Pts',(23.9225830034177,24.5530879770028,14.2235304635197));
#54954=CARTESIAN_POINT('Ctrl Pts',(23.9225830034177,18.376353041482,19.9212564991933));
#54955=CARTESIAN_POINT('Ctrl Pts',(23.3421815947946,18.4557508948393,20.007329345021));
#54956=CARTESIAN_POINT('Ctrl Pts',(23.3421815947946,7.91887987539518,29.7270607190791));
#54957=CARTESIAN_POINT('Ctrl Pts',(23.3421815947946,-6.05693630938179,26.5371718756275));
#54958=CARTESIAN_POINT('Ctrl Pts',(23.3421815947946,-32.5941081850093,20.4802355662457));
#54959=CARTESIAN_POINT('Ctrl Pts',(23.3421815947946,-26.5371718756275,-6.05693630938179));
#54960=CARTESIAN_POINT('Ctrl Pts',(23.3421815947946,-20.4802355662457,-32.5941081850093));
#54961=CARTESIAN_POINT('Ctrl Pts',(23.3421815947946,6.05693630938179,-26.5371718756275));
#54962=CARTESIAN_POINT('Ctrl Pts',(23.3421815947946,32.5941081850093,-20.4802355662457));
#54963=CARTESIAN_POINT('Ctrl Pts',(23.3421815947946,26.5371718756275,6.05693630938179));
#54964=CARTESIAN_POINT('Ctrl Pts',(23.3421815947946,24.6591733615329,14.2849854096353));
#54965=CARTESIAN_POINT('Ctrl Pts',(23.3421815947946,18.4557508948393,20.007329345021));
#54966=CARTESIAN_POINT('Ctrl Pts',(22.5631762070947,18.5786269363992,20.140535598514));
#54967=CARTESIAN_POINT('Ctrl Pts',(22.5631762070947,7.97160277018397,29.9249797075388));
#54968=CARTESIAN_POINT('Ctrl Pts',(22.5631762070947,-6.09726262078022,26.7138529899778));
#54969=CARTESIAN_POINT('Ctrl Pts',(22.5631762070947,-32.811115610758,20.6165903691975));
#54970=CARTESIAN_POINT('Ctrl Pts',(22.5631762070947,-26.7138529899778,-6.09726262078022));
#54971=CARTESIAN_POINT('Ctrl Pts',(22.5631762070947,-20.6165903691975,-32.811115610758));
#54972=CARTESIAN_POINT('Ctrl Pts',(22.5631762070947,6.09726262078022,-26.7138529899778));
#54973=CARTESIAN_POINT('Ctrl Pts',(22.5631762070947,32.811115610758,-20.6165903691975));
#54974=CARTESIAN_POINT('Ctrl Pts',(22.5631762070947,26.7138529899778,6.09726262078022));
#54975=CARTESIAN_POINT('Ctrl Pts',(22.5631762070947,24.823351000691,14.3800930251898));
#54976=CARTESIAN_POINT('Ctrl Pts',(22.5631762070947,18.5786269363992,20.140535598514));
#54977=CARTESIAN_POINT('Ctrl Pts',(21.5808622776984,18.7610722387808,20.3383191117939));
#54978=CARTESIAN_POINT('Ctrl Pts',(21.5808622776984,8.049885276359,30.2188481398075));
#54979=CARTESIAN_POINT('Ctrl Pts',(21.5808622776984,-6.15713878527593,26.9761876072355));
#54980=CARTESIAN_POINT('Ctrl Pts',(21.5808622776984,-33.1333263925114,20.8190488219595));
#54981=CARTESIAN_POINT('Ctrl Pts',(21.5808622776984,-26.9761876072355,-6.15713878527593));
#54982=CARTESIAN_POINT('Ctrl Pts',(21.5808622776984,-20.8190488219595,-33.1333263925114));
#54983=CARTESIAN_POINT('Ctrl Pts',(21.5808622776984,6.15713878527593,-26.9761876072355));
#54984=CARTESIAN_POINT('Ctrl Pts',(21.5808622776984,33.1333263925114,-20.8190488219595));
#54985=CARTESIAN_POINT('Ctrl Pts',(21.5808622776984,26.9761876072355,6.15713878527593));
#54986=CARTESIAN_POINT('Ctrl Pts',(21.5808622776984,25.0671205642303,14.521308004598));
#54987=CARTESIAN_POINT('Ctrl Pts',(21.5808622776984,18.7610722387808,20.3383191117939));
#54988=CARTESIAN_POINT('Ctrl Pts',(20.5902243197586,18.9731487726588,20.5682249597772));
#54989=CARTESIAN_POINT('Ctrl Pts',(20.5902243197586,8.14088176876611,30.5604442111678));
#54990=CARTESIAN_POINT('Ctrl Pts',(20.5902243197586,-6.22673953280078,27.2811284065763));
#54991=CARTESIAN_POINT('Ctrl Pts',(20.5902243197586,-33.5078679393771,21.0543888737755));
#54992=CARTESIAN_POINT('Ctrl Pts',(20.5902243197586,-27.2811284065763,-6.22673953280078));
#54993=CARTESIAN_POINT('Ctrl Pts',(20.5902243197586,-21.0543888737755,-33.5078679393771));
#54994=CARTESIAN_POINT('Ctrl Pts',(20.5902243197586,6.22673953280078,-27.2811284065763));
#54995=CARTESIAN_POINT('Ctrl Pts',(20.5902243197586,33.5078679393771,-21.0543888737755));
#54996=CARTESIAN_POINT('Ctrl Pts',(20.5902243197586,27.2811284065763,6.22673953280078));
#54997=CARTESIAN_POINT('Ctrl Pts',(20.5902243197586,25.3504811299752,14.6854579332265));
#54998=CARTESIAN_POINT('Ctrl Pts',(20.5902243197586,18.9731487726588,20.5682249597772));
#54999=CARTESIAN_POINT('Ctrl Pts',(19.591895069338,19.2158583309824,20.831339156335));
#55000=CARTESIAN_POINT('Ctrl Pts',(19.591895069338,8.24502209055126,30.9513815302994));
#55001=CARTESIAN_POINT('Ctrl Pts',(19.591895069338,-6.30639363871178,27.6301158469569));
#55002=CARTESIAN_POINT('Ctrl Pts',(19.591895069338,-33.9365094856687,21.3237222082451));
#55003=CARTESIAN_POINT('Ctrl Pts',(19.591895069338,-27.6301158469569,-6.30639363871178));
#55004=CARTESIAN_POINT('Ctrl Pts',(19.591895069338,-21.3237222082451,-33.9365094856687));
#55005=CARTESIAN_POINT('Ctrl Pts',(19.591895069338,6.30639363871178,-27.6301158469569));
#55006=CARTESIAN_POINT('Ctrl Pts',(19.591895069338,33.9365094856687,-21.3237222082451));
#55007=CARTESIAN_POINT('Ctrl Pts',(19.591895069338,27.6301158469569,6.30639363871178));
#55008=CARTESIAN_POINT('Ctrl Pts',(19.591895069338,25.6747712176182,14.8733182115315));
#55009=CARTESIAN_POINT('Ctrl Pts',(19.591895069338,19.2158583309824,20.831339156335));
#55010=CARTESIAN_POINT('Ctrl Pts',(18.5871162949016,19.4903525092225,21.1289101117858));
#55011=CARTESIAN_POINT('Ctrl Pts',(18.5871162949016,8.36280036120327,31.3935149959097));
#55012=CARTESIAN_POINT('Ctrl Pts',(18.5871162949016,-6.3964790415962,28.0248057855197));
#55013=CARTESIAN_POINT('Ctrl Pts',(18.5871162949016,-34.4212848271159,21.6283267439235));
#55014=CARTESIAN_POINT('Ctrl Pts',(18.5871162949016,-28.0248057855197,-6.3964790415962));
#55015=CARTESIAN_POINT('Ctrl Pts',(18.5871162949016,-21.6283267439235,-34.4212848271159));
#55016=CARTESIAN_POINT('Ctrl Pts',(18.5871162949016,6.3964790415962,-28.0248057855197));
#55017=CARTESIAN_POINT('Ctrl Pts',(18.5871162949016,34.4212848271159,-21.6283267439235));
#55018=CARTESIAN_POINT('Ctrl Pts',(18.5871162949016,28.0248057855197,6.3964790415962));
#55019=CARTESIAN_POINT('Ctrl Pts',(18.5871162949016,26.041529501609,15.085780189022));
#55020=CARTESIAN_POINT('Ctrl Pts',(18.5871162949016,19.4903525092225,21.1289101117858));
#55021=CARTESIAN_POINT('Ctrl Pts',(17.577868433379,19.7977977061578,21.4622022842733));
#55022=CARTESIAN_POINT('Ctrl Pts',(17.577868433379,8.49471705192315,31.8887233507017));
#55023=CARTESIAN_POINT('Ctrl Pts',(17.577868433379,-6.49737853829363,28.4668753648014));
#55024=CARTESIAN_POINT('Ctrl Pts',(17.577868433379,-34.964253903095,21.9694968265077));
#55025=CARTESIAN_POINT('Ctrl Pts',(17.577868433379,-28.4668753648014,-6.49737853829363));
#55026=CARTESIAN_POINT('Ctrl Pts',(17.577868433379,-21.9694968265077,-34.964253903095));
#55027=CARTESIAN_POINT('Ctrl Pts',(17.577868433379,6.49737853829363,-28.4668753648014));
#55028=CARTESIAN_POINT('Ctrl Pts',(17.577868433379,34.964253903095,-21.9694968265077));
#55029=CARTESIAN_POINT('Ctrl Pts',(17.577868433379,28.4668753648014,6.49737853829363));
#55030=CARTESIAN_POINT('Ctrl Pts',(17.577868433379,26.4523144354541,15.3237466731552));
#55031=CARTESIAN_POINT('Ctrl Pts',(17.577868433379,19.7977977061578,21.4622022842733));
#55032=CARTESIAN_POINT('Ctrl Pts',(16.5668667015923,20.1391691218662,21.8322728591294));
#55033=CARTESIAN_POINT('Ctrl Pts',(16.5668667015923,8.64119059555145,32.4385773696654));
#55034=CARTESIAN_POINT('Ctrl Pts',(16.5668667015923,-6.60941217672811,28.9577268063763));
#55035=CARTESIAN_POINT('Ctrl Pts',(16.5668667015923,-35.5671389831044,22.3483146296482));
#55036=CARTESIAN_POINT('Ctrl Pts',(16.5668667015923,-28.9577268063763,-6.60941217672811));
#55037=CARTESIAN_POINT('Ctrl Pts',(16.5668667015923,-22.3483146296482,-35.5671389831044));
#55038=CARTESIAN_POINT('Ctrl Pts',(16.5668667015923,6.60941217672811,-28.9577268063763));
#55039=CARTESIAN_POINT('Ctrl Pts',(16.5668667015923,35.5671389831044,-22.3483146296482));
#55040=CARTESIAN_POINT('Ctrl Pts',(16.5668667015923,28.9577268063763,6.60941217672811));
#55041=CARTESIAN_POINT('Ctrl Pts',(16.5668667015923,26.9084290074696,15.5879724811674));
#55042=CARTESIAN_POINT('Ctrl Pts',(16.5668667015923,20.1391691218662,21.8322728591294));
#55043=CARTESIAN_POINT('Ctrl Pts',(15.5576189940876,20.5150087935408,22.239709442716));
#55044=CARTESIAN_POINT('Ctrl Pts',(15.5576189940876,8.80245356606713,33.0439501233491));
#55045=CARTESIAN_POINT('Ctrl Pts',(15.5576189940876,-6.7327578464244,29.4981394951766));
#55046=CARTESIAN_POINT('Ctrl Pts',(15.5576189940876,-36.230897341601,22.7653816487522));
#55047=CARTESIAN_POINT('Ctrl Pts',(15.5576189940876,-29.4981394951766,-6.7327578464244));
#55048=CARTESIAN_POINT('Ctrl Pts',(15.5576189940876,-22.7653816487522,-36.230897341601));
#55049=CARTESIAN_POINT('Ctrl Pts',(15.5576189940876,6.7327578464244,-29.4981394951766));
#55050=CARTESIAN_POINT('Ctrl Pts',(15.5576189940876,36.230897341601,-22.7653816487522));
#55051=CARTESIAN_POINT('Ctrl Pts',(15.5576189940876,29.4981394951766,6.7327578464244));
#55052=CARTESIAN_POINT('Ctrl Pts',(15.5576189940876,27.4105974466067,15.8788771567249));
#55053=CARTESIAN_POINT('Ctrl Pts',(15.5576189940876,20.5150087935408,22.239709442716));
#55054=CARTESIAN_POINT('Ctrl Pts',(14.5544447688713,20.9251959536421,22.6843811145439));
#55055=CARTESIAN_POINT('Ctrl Pts',(14.5544447688713,8.97845414527848,33.7046470889725));
#55056=CARTESIAN_POINT('Ctrl Pts',(14.5544447688713,-6.86737591305397,30.0879397818628));
#55057=CARTESIAN_POINT('Ctrl Pts',(14.5544447688713,-36.9553156949167,23.2205638688088));
#55058=CARTESIAN_POINT('Ctrl Pts',(14.5544447688713,-30.0879397818628,-6.86737591305397));
#55059=CARTESIAN_POINT('Ctrl Pts',(14.5544447688713,-23.2205638688088,-36.9553156949167));
#55060=CARTESIAN_POINT('Ctrl Pts',(14.5544447688713,6.86737591305397,-30.0879397818628));
#55061=CARTESIAN_POINT('Ctrl Pts',(14.5544447688713,36.9553156949167,-23.2205638688088));
#55062=CARTESIAN_POINT('Ctrl Pts',(14.5544447688713,30.0879397818628,6.86737591305397));
#55063=CARTESIAN_POINT('Ctrl Pts',(14.5544447688713,27.9586583924468,16.1963672242196));
#55064=CARTESIAN_POINT('Ctrl Pts',(14.5544447688713,20.9251959536421,22.6843811145439));
#55065=CARTESIAN_POINT('Ctrl Pts',(13.5625963827217,21.3685644590621,23.1650236936344));
#55066=CARTESIAN_POINT('Ctrl Pts',(13.5625963827217,9.16869197168609,34.4187899356465));
#55067=CARTESIAN_POINT('Ctrl Pts',(13.5625963827217,-7.012883663685,30.7254508915224));
#55068=CARTESIAN_POINT('Ctrl Pts',(13.5625963827217,-37.7383345552074,23.7125672278374));
#55069=CARTESIAN_POINT('Ctrl Pts',(13.5625963827217,-30.7254508915224,-7.012883663685));
#55070=CARTESIAN_POINT('Ctrl Pts',(13.5625963827217,-23.7125672278374,-37.7383345552074));
#55071=CARTESIAN_POINT('Ctrl Pts',(13.5625963827217,7.012883663685,-30.7254508915224));
#55072=CARTESIAN_POINT('Ctrl Pts',(13.5625963827217,37.7383345552074,-23.7125672278374));
#55073=CARTESIAN_POINT('Ctrl Pts',(13.5625963827217,30.7254508915224,7.012883663685));
#55074=CARTESIAN_POINT('Ctrl Pts',(13.5625963827217,28.5510537330912,16.5395400740865));
#55075=CARTESIAN_POINT('Ctrl Pts',(13.5625963827217,21.3685644590621,23.1650236936344));
#55076=CARTESIAN_POINT('Ctrl Pts',(12.5880795783847,21.8428970524859,23.679233517433));
#55077=CARTESIAN_POINT('Ctrl Pts',(12.5880795783847,9.37221567818334,35.1828072810307));
#55078=CARTESIAN_POINT('Ctrl Pts',(12.5880795783847,-7.16855342343642,31.4074846721918));
#55079=CARTESIAN_POINT('Ctrl Pts',(12.5880795783847,-38.5760380956282,24.2389312487553));
#55080=CARTESIAN_POINT('Ctrl Pts',(12.5880795783847,-31.4074846721918,-7.16855342343642));
#55081=CARTESIAN_POINT('Ctrl Pts',(12.5880795783847,-24.2389312487553,-38.5760380956282));
#55082=CARTESIAN_POINT('Ctrl Pts',(12.5880795783847,7.16855342343642,-31.4074846721918));
#55083=CARTESIAN_POINT('Ctrl Pts',(12.5880795783847,38.5760380956282,-24.2389312487553));
#55084=CARTESIAN_POINT('Ctrl Pts',(12.5880795783847,31.4074846721918,7.16855342343642));
#55085=CARTESIAN_POINT('Ctrl Pts',(12.5880795783847,29.1848209376287,16.9066795210254));
#55086=CARTESIAN_POINT('Ctrl Pts',(12.5880795783847,21.8428970524859,23.679233517433));
#55087=CARTESIAN_POINT('Ctrl Pts',(11.6370973936883,22.3454091248114,24.2239918742266));
#55088=CARTESIAN_POINT('Ctrl Pts',(11.6370973936883,9.58783046185459,35.9922138974944));
#55089=CARTESIAN_POINT('Ctrl Pts',(11.6370973936883,-7.33347131998334,32.1300371876035));
#55090=CARTESIAN_POINT('Ctrl Pts',(11.6370973936883,-39.4635085075868,24.7965658676202));
#55091=CARTESIAN_POINT('Ctrl Pts',(11.6370973936883,-32.1300371876035,-7.33347131998334));
#55092=CARTESIAN_POINT('Ctrl Pts',(11.6370973936883,-24.7965658676202,-39.4635085075868));
#55093=CARTESIAN_POINT('Ctrl Pts',(11.6370973936883,7.33347131998334,-32.1300371876035));
#55094=CARTESIAN_POINT('Ctrl Pts',(11.6370973936883,39.4635085075868,-24.7965658676202));
#55095=CARTESIAN_POINT('Ctrl Pts',(11.6370973936883,32.1300371876035,7.33347131998334));
#55096=CARTESIAN_POINT('Ctrl Pts',(11.6370973936883,29.856239422758,17.2956302422525));
#55097=CARTESIAN_POINT('Ctrl Pts',(11.6370973936883,22.3454091248114,24.2239918742266));
#55098=CARTESIAN_POINT('Ctrl Pts',(10.7155646400367,22.8730721573722,24.7960156372148));
#55099=CARTESIAN_POINT('Ctrl Pts',(10.7155646400367,9.81423686457129,36.8421316872136));
#55100=CARTESIAN_POINT('Ctrl Pts',(10.7155646400367,-7.5066434330687,32.8887537885844));
#55101=CARTESIAN_POINT('Ctrl Pts',(10.7155646400367,-40.3953972216531,25.3821103555157));
#55102=CARTESIAN_POINT('Ctrl Pts',(10.7155646400367,-32.8887537885844,-7.5066434330687));
#55103=CARTESIAN_POINT('Ctrl Pts',(10.7155646400367,-25.3821103555157,-40.3953972216531));
#55104=CARTESIAN_POINT('Ctrl Pts',(10.7155646400367,7.5066434330687,-32.8887537885844));
#55105=CARTESIAN_POINT('Ctrl Pts',(10.7155646400367,40.3953972216531,-25.3821103555157));
#55106=CARTESIAN_POINT('Ctrl Pts',(10.7155646400367,32.8887537885844,7.5066434330687));
#55107=CARTESIAN_POINT('Ctrl Pts',(10.7155646400367,30.5612627117334,17.7040481258859));
#55108=CARTESIAN_POINT('Ctrl Pts',(10.7155646400367,22.8730721573722,24.7960156372148));
#55109=CARTESIAN_POINT('Ctrl Pts',(9.82859575068344,23.4229557116635,25.392128005376));
#55110=CARTESIAN_POINT('Ctrl Pts',(9.82859575068344,10.0501775118362,37.7278405321141));
#55111=CARTESIAN_POINT('Ctrl Pts',(9.82859575068344,-7.68710803106292,33.6794208535527));
#55112=CARTESIAN_POINT('Ctrl Pts',(9.82859575068344,-41.3665288846156,25.9923128224897));
#55113=CARTESIAN_POINT('Ctrl Pts',(9.82859575068344,-33.6794208535527,-7.68710803106292));
#55114=CARTESIAN_POINT('Ctrl Pts',(9.82859575068344,-25.9923128224897,-41.3665288846156));
#55115=CARTESIAN_POINT('Ctrl Pts',(9.82859575068344,7.68710803106292,-33.6794208535527));
#55116=CARTESIAN_POINT('Ctrl Pts',(9.82859575068344,41.3665288846156,-25.9923128224897));
#55117=CARTESIAN_POINT('Ctrl Pts',(9.82859575068344,33.6794208535527,7.68710803106292));
#55118=CARTESIAN_POINT('Ctrl Pts',(9.82859575068344,31.2959753750754,18.1296649753334));
#55119=CARTESIAN_POINT('Ctrl Pts',(9.82859575068344,23.4229557116635,25.392128005376));
#55120=CARTESIAN_POINT('Ctrl Pts',(8.97989469943246,23.9925534429024,26.00961192505));
#55121=CARTESIAN_POINT('Ctrl Pts',(8.97989469943246,10.2945769966732,38.6453034106753));
#55122=CARTESIAN_POINT('Ctrl Pts',(8.97989469943246,-7.87404256435504,34.4984345571934));
#55123=CARTESIAN_POINT('Ctrl Pts',(8.97989469943246,-42.3724771215484,26.6243919928384));
#55124=CARTESIAN_POINT('Ctrl Pts',(8.97989469943246,-34.4984345571934,-7.87404256435504));
#55125=CARTESIAN_POINT('Ctrl Pts',(8.97989469943246,-26.6243919928384,-42.3724771215484));
#55126=CARTESIAN_POINT('Ctrl Pts',(8.97989469943246,7.87404256435504,-34.4984345571934));
#55127=CARTESIAN_POINT('Ctrl Pts',(8.97989469943246,42.3724771215484,-26.6243919928384));
#55128=CARTESIAN_POINT('Ctrl Pts',(8.97989469943246,34.4984345571934,7.87404256435504));
#55129=CARTESIAN_POINT('Ctrl Pts',(8.97989469943246,32.057028625143,18.5705408479257));
#55130=CARTESIAN_POINT('Ctrl Pts',(8.97989469943246,23.9925534429024,26.00961192505));
#55131=CARTESIAN_POINT('Ctrl Pts',(8.1713316609345,24.5800320418402,26.6464799603347));
#55132=CARTESIAN_POINT('Ctrl Pts',(8.1713316609345,10.5466486940461,39.5915673736694));
#55133=CARTESIAN_POINT('Ctrl Pts',(8.1713316609345,-8.06684536480278,35.3431588191374));
#55134=CARTESIAN_POINT('Ctrl Pts',(8.1713316609345,-43.4100041839401,27.2763134543346));
#55135=CARTESIAN_POINT('Ctrl Pts',(8.1713316609345,-35.3431588191374,-8.06684536480278));
#55136=CARTESIAN_POINT('Ctrl Pts',(8.1713316609345,-27.2763134543346,-43.4100041839401));
#55137=CARTESIAN_POINT('Ctrl Pts',(8.1713316609345,8.06684536480278,-35.3431588191374));
#55138=CARTESIAN_POINT('Ctrl Pts',(8.1713316609345,43.4100041839401,-27.2763134543346));
#55139=CARTESIAN_POINT('Ctrl Pts',(8.1713316609345,35.3431588191374,8.06684536480278));
#55140=CARTESIAN_POINT('Ctrl Pts',(8.1713316609345,32.8419729332853,19.0252567390383));
#55141=CARTESIAN_POINT('Ctrl Pts',(8.1713316609345,24.5800320418402,26.6464799603347));
#55142=CARTESIAN_POINT('Ctrl Pts',(7.40358438374929,25.1841184850965,27.3013520645346));
#55143=CARTESIAN_POINT('Ctrl Pts',(7.40358438374929,10.8058463829268,40.5645819359366));
#55144=CARTESIAN_POINT('Ctrl Pts',(7.40358438374929,-8.26509864276547,36.2117631833691));
#55145=CARTESIAN_POINT('Ctrl Pts',(7.40358438374929,-44.4768618261345,27.9466645406036));
#55146=CARTESIAN_POINT('Ctrl Pts',(7.40358438374929,-36.2117631833691,-8.26509864276547));
#55147=CARTESIAN_POINT('Ctrl Pts',(7.40358438374929,-27.9466645406036,-44.4768618261345));
#55148=CARTESIAN_POINT('Ctrl Pts',(7.40358438374929,8.26509864276547,-36.2117631833691));
#55149=CARTESIAN_POINT('Ctrl Pts',(7.40358438374929,44.4768618261345,-27.9466645406036));
#55150=CARTESIAN_POINT('Ctrl Pts',(7.40358438374929,36.2117631833691,8.26509864276547));
#55151=CARTESIAN_POINT('Ctrl Pts',(7.40358438374929,33.6491073822974,19.4928273124192));
#55152=CARTESIAN_POINT('Ctrl Pts',(7.40358438374929,25.1841184850965,27.3013520645346));
#55153=CARTESIAN_POINT('Ctrl Pts',(6.82198164612729,25.6800473090374,27.8389737180133));
#55154=CARTESIAN_POINT('Ctrl Pts',(6.82198164612729,11.0186364669452,41.3633847776977));
#55155=CARTESIAN_POINT('Ctrl Pts',(6.82198164612729,-8.42785600320625,36.9248497716085));
#55156=CARTESIAN_POINT('Ctrl Pts',(6.82198164612729,-45.3527057748147,28.4969937684022));
#55157=CARTESIAN_POINT('Ctrl Pts',(6.82198164612729,-36.9248497716085,-8.42785600320625));
#55158=CARTESIAN_POINT('Ctrl Pts',(6.82198164612729,-28.4969937684022,-45.3527057748147));
#55159=CARTESIAN_POINT('Ctrl Pts',(6.82198164612729,8.42785600320625,-36.9248497716085));
#55160=CARTESIAN_POINT('Ctrl Pts',(6.82198164612729,45.3527057748147,-28.4969937684022));
#55161=CARTESIAN_POINT('Ctrl Pts',(6.82198164612729,36.9248497716085,8.42785600320625));
#55162=CARTESIAN_POINT('Ctrl Pts',(6.82198164612729,34.3117298306725,19.8766825158504));
#55163=CARTESIAN_POINT('Ctrl Pts',(6.82198164612729,25.6800473090374,27.8389737180133));
#55164=CARTESIAN_POINT('Ctrl Pts',(6.40395249919757,26.0589392503377,28.2497191761072));
#55165=CARTESIAN_POINT('Ctrl Pts',(6.40395249919757,11.1812090865047,41.9736738853683));
#55166=CARTESIAN_POINT('Ctrl Pts',(6.40395249919757,-8.55220338791415,37.4696512606331));
#55167=CARTESIAN_POINT('Ctrl Pts',(6.40395249919757,-46.0218546485472,28.9174478727189));
#55168=CARTESIAN_POINT('Ctrl Pts',(6.40395249919757,-37.4696512606331,-8.55220338791415));
#55169=CARTESIAN_POINT('Ctrl Pts',(6.40395249919757,-28.9174478727189,-46.0218546485472));
#55170=CARTESIAN_POINT('Ctrl Pts',(6.40395249919757,8.55220338791415,-37.4696512606331));
#55171=CARTESIAN_POINT('Ctrl Pts',(6.40395249919757,46.0218546485472,-28.9174478727189));
#55172=CARTESIAN_POINT('Ctrl Pts',(6.40395249919757,37.4696512606331,8.55220338791415));
#55173=CARTESIAN_POINT('Ctrl Pts',(6.40395249919757,34.8179764807844,20.1699496868337));
#55174=CARTESIAN_POINT('Ctrl Pts',(6.40395249919757,26.0589392503377,28.2497191761072));
#55175=CARTESIAN_POINT('Ctrl Pts',(6.13331019225912,26.3146081748953,28.5268822352565));
#55176=CARTESIAN_POINT('Ctrl Pts',(6.13331019225912,11.2909099333019,42.3854851244564));
#55177=CARTESIAN_POINT('Ctrl Pts',(6.13331019225912,-8.63611058850204,37.8372727263161));
#55178=CARTESIAN_POINT('Ctrl Pts',(6.13331019225912,-46.4733833148181,29.201162137814));
#55179=CARTESIAN_POINT('Ctrl Pts',(6.13331019225912,-37.8372727263161,-8.63611058850204));
#55180=CARTESIAN_POINT('Ctrl Pts',(6.13331019225912,-29.201162137814,-46.4733833148181));
#55181=CARTESIAN_POINT('Ctrl Pts',(6.13331019225912,8.63611058850204,-37.8372727263161));
#55182=CARTESIAN_POINT('Ctrl Pts',(6.13331019225912,46.4733833148181,-29.201162137814));
#55183=CARTESIAN_POINT('Ctrl Pts',(6.13331019225912,37.8372727263161,8.63611058850204));
#55184=CARTESIAN_POINT('Ctrl Pts',(6.13331019225912,35.1595818898379,20.3678406790677));
#55185=CARTESIAN_POINT('Ctrl Pts',(6.13331019225912,26.3146081748953,28.5268822352565));
#55186=CARTESIAN_POINT('Ctrl Pts',(6.,26.4432112098191,28.666296951523));
#55187=CARTESIAN_POINT('Ctrl Pts',(6.,11.3460901311154,42.5926286998992));
#55188=CARTESIAN_POINT('Ctrl Pts',(6.,-8.67831642429626,38.0221885750911));
#55189=CARTESIAN_POINT('Ctrl Pts',(6.,-46.7005049993874,29.3438721507949));
#55190=CARTESIAN_POINT('Ctrl Pts',(6.,-38.0221885750911,-8.67831642429626));
#55191=CARTESIAN_POINT('Ctrl Pts',(6.,-29.3438721507949,-46.7005049993874));
#55192=CARTESIAN_POINT('Ctrl Pts',(6.,8.67831642429626,-38.0221885750911));
#55193=CARTESIAN_POINT('Ctrl Pts',(6.,46.7005049993874,-29.3438721507949));
#55194=CARTESIAN_POINT('Ctrl Pts',(6.,38.0221885750911,8.67831642429626));
#55195=CARTESIAN_POINT('Ctrl Pts',(6.,35.3314115027902,20.4673810601656));
#55196=CARTESIAN_POINT('Ctrl Pts',(6.,26.4432112098191,28.666296951523));
#55197=CARTESIAN_POINT('Ctrl Pts',(24.5,18.3068383223113,19.8458980809827));
#55198=CARTESIAN_POINT('Ctrl Pts',(23.5178991898112,16.2627537755328,21.9594009189012));
#55199=CARTESIAN_POINT('Ctrl Pts',(22.3947886245986,13.9837756084006,23.7568819701794));
#55200=CARTESIAN_POINT('Ctrl Pts',(21.1743874927566,11.5811351476418,25.2768725242511));
#55201=CARTESIAN_POINT('Ctrl Pts',(20.503187179342,10.2597228773583,26.1128420343255));
#55202=CARTESIAN_POINT('Ctrl Pts',(19.8411792966381,8.88159416625748,26.8568611155666));
#55203=CARTESIAN_POINT('Ctrl Pts',(19.1295827650218,7.49741935561041,27.5300055539183));
#55204=CARTESIAN_POINT('Ctrl Pts',(18.8261415870883,6.90717528281466,27.8170498721766));
#55205=CARTESIAN_POINT('Ctrl Pts',(18.5104994276256,6.31111450131055,28.0937655905368));
#55206=CARTESIAN_POINT('Ctrl Pts',(18.2016639423759,5.75492178098747,28.3466719251461));
#55207=CARTESIAN_POINT('Ctrl Pts',(17.6747132403632,4.80591767224158,28.778193485753));
#55208=CARTESIAN_POINT('Ctrl Pts',(17.2016343370993,3.9436255315325,29.1307365554341));
#55209=CARTESIAN_POINT('Ctrl Pts',(16.8729352926459,3.36394482370453,29.365352154054));
#55210=CARTESIAN_POINT('Ctrl Pts',(16.6342454025476,2.94300072064618,29.5357218962085));
#55211=CARTESIAN_POINT('Ctrl Pts',(16.5014949770664,2.71490739519207,29.6262286540088));
#55212=CARTESIAN_POINT('Ctrl Pts',(16.3424569562978,2.44504465168102,29.7338311889201));
#55213=CARTESIAN_POINT('Ctrl Pts',(15.993118510103,1.85227173456061,29.9701878926247));
#55214=CARTESIAN_POINT('Ctrl Pts',(15.6312480487537,1.26509075909629,30.2031020416042));
#55215=CARTESIAN_POINT('Ctrl Pts',(15.2503296894305,0.693179555091501,30.4420009717055));
#55216=CARTESIAN_POINT('Ctrl Pts',(14.7484414179076,-0.0603559955513863,
30.7567680816717));
#55217=CARTESIAN_POINT('Ctrl Pts',(14.2669345517206,-0.791651325392304,
31.0498576441856));
#55218=CARTESIAN_POINT('Ctrl Pts',(13.7912435751455,-1.46438575958394,31.3399123313253));
#55219=CARTESIAN_POINT('Ctrl Pts',(13.5533980868579,-1.80075297667976,31.4849396748952));
#55220=CARTESIAN_POINT('Ctrl Pts',(13.3161115657262,-2.1244256180349,31.6299384327499));
#55221=CARTESIAN_POINT('Ctrl Pts',(13.0766514227367,-2.43421540696108,31.7786491461901));
#55222=CARTESIAN_POINT('Ctrl Pts',(12.9188702359555,-2.63833706135937,31.8766351933073));
#55223=CARTESIAN_POINT('Ctrl Pts',(12.7601526360409,-2.83643714593442,31.9762372272926));
#55224=CARTESIAN_POINT('Ctrl Pts',(12.5997389313808,-3.02815130787591,32.0786431431723));
#55225=CARTESIAN_POINT('Ctrl Pts',(12.5166971934814,-3.12739642674706,32.1316558533011));
#55226=CARTESIAN_POINT('Ctrl Pts',(12.4397215765388,-3.21752746773653,32.1811723683389));
#55227=CARTESIAN_POINT('Ctrl Pts',(12.3478597934844,-3.32215188831681,32.2409557398963));
#55228=CARTESIAN_POINT('Ctrl Pts',(11.9116121727781,-3.8190087207047,32.5248643766822));
#55229=CARTESIAN_POINT('Ctrl Pts',(10.7144663992386,-5.25575553834431,33.2889282188856));
#55230=CARTESIAN_POINT('Ctrl Pts',(9.56604185022482,-6.09942127757595,34.2764524708192));
#55231=CARTESIAN_POINT('Ctrl Pts',(9.07284645450781,-6.46173681538865,34.7005486072444));
#55232=CARTESIAN_POINT('Ctrl Pts',(8.57333454992787,-6.74267387425559,35.171504935247));
#55233=CARTESIAN_POINT('Ctrl Pts',(8.00348148263079,-7.02395144844514,35.7754858324545));
#55234=CARTESIAN_POINT('Ctrl Pts',(7.63919428965979,-7.20376239240166,36.1615897569194));
#55235=CARTESIAN_POINT('Ctrl Pts',(7.24388644384695,-7.38116314765918,36.6129669384717));
#55236=CARTESIAN_POINT('Ctrl Pts',(6.94254646282575,-7.51431133904849,36.9770001219077));
#55237=CARTESIAN_POINT('Ctrl Pts',(6.91433564865292,-7.52677639221536,37.0110801416112));
#55238=CARTESIAN_POINT('Ctrl Pts',(6.88669635040566,-7.53896719832808,37.0446474052169));
#55239=CARTESIAN_POINT('Ctrl Pts',(6.85962514029878,-7.55089284691699,37.0776869008724));
#55240=CARTESIAN_POINT('Ctrl Pts',(6.44000062073739,-7.73574954670347,37.5898244239546));
#55241=CARTESIAN_POINT('Ctrl Pts',(6.15412442492902,-7.81952894703128,37.9841916530545));
#55242=CARTESIAN_POINT('Ctrl Pts',(6.,-7.86863926112478,38.1979648172293));
#55243=CARTESIAN_POINT('Ctrl Pts',(2.1,-1.28114692797347,9.65763472891602));
#55244=CARTESIAN_POINT('Ctrl Pts',(2.73333333333333,-1.28114692797347,9.65763472891602));
#55245=CARTESIAN_POINT('Ctrl Pts',(3.36701669548158,-1.28120274047516,9.65763272452521));
#55246=CARTESIAN_POINT('Ctrl Pts',(4.12582575310106,-1.28121960670544,9.65763220679461));
#55247=CARTESIAN_POINT('Ctrl Pts',(4.38278636589858,-1.28250284215921,9.65747570633452));
#55248=CARTESIAN_POINT('Ctrl Pts',(4.88875443651799,-1.28819124993779,9.65678908665978));
#55249=CARTESIAN_POINT('Ctrl Pts',(5.76580325925563,-1.30131080478345,9.65522040881189));
#55250=CARTESIAN_POINT('Ctrl Pts',(6.49302708244736,-1.30111147249391,9.65528059069283));
#55251=CARTESIAN_POINT('Ctrl Pts',(7.02340672589377,-1.27967384267621,9.6577356709489));
#55252=CARTESIAN_POINT('Ctrl Pts',(7.14986679476879,-1.2744035847383,9.65840531711269));
#55253=CARTESIAN_POINT('Ctrl Pts',(7.33705121725519,-1.26602996195062,9.65954820770469));
#55254=CARTESIAN_POINT('Ctrl Pts',(7.52532549516812,-1.25695505359351,9.66085108878951));
#55255=CARTESIAN_POINT('Ctrl Pts',(7.90080343897497,-1.23734054050575,9.66372617426799));
#55256=CARTESIAN_POINT('Ctrl Pts',(8.46124590624133,-1.20179139860997,9.66897349947471));
#55257=CARTESIAN_POINT('Ctrl Pts',(9.0650192250414,-1.14716675316572,9.67573613473312));
#55258=CARTESIAN_POINT('Ctrl Pts',(9.52839384147276,-1.09219084928558,9.68122767953111));
#55259=CARTESIAN_POINT('Ctrl Pts',(9.75198702930936,-1.06064937497063,9.68391236927288));
#55260=CARTESIAN_POINT('Ctrl Pts',(10.3692921392863,-0.965652648141829,
9.69126404805778));
#55261=CARTESIAN_POINT('Ctrl Pts',(11.3477764514917,-0.751349332513189,
9.71242942002159));
#55262=CARTESIAN_POINT('Ctrl Pts',(12.273624621788,-0.471227384196326,9.73058177218512));
#55263=CARTESIAN_POINT('Ctrl Pts',(13.0004910640178,-0.241262883353551,
9.73434036989634));
#55264=CARTESIAN_POINT('Ctrl Pts',(13.5002210053635,-0.0656770837232706,
9.73563225387362));
#55265=CARTESIAN_POINT('Ctrl Pts',(14.4706186721272,0.32956163981752,9.73289534983573));
#55266=CARTESIAN_POINT('Ctrl Pts',(15.1515630987551,0.653141644356525,9.71756271653061));
#55267=CARTESIAN_POINT('Ctrl Pts',(15.8843828864863,1.00441577560146,9.68186404942655));
#55268=CARTESIAN_POINT('Ctrl Pts',(16.3868682969429,1.26265129573327,9.65060020522716));
#55269=CARTESIAN_POINT('Ctrl Pts',(17.3638401545857,1.81703406288438,9.5663953411847));
#55270=CARTESIAN_POINT('Ctrl Pts',(18.0499667751367,2.24816630064726,9.47400212950933));
#55271=CARTESIAN_POINT('Ctrl Pts',(18.7841437937616,2.70564998147611,9.34646266782294));
#55272=CARTESIAN_POINT('Ctrl Pts',(19.2876952035555,3.03517152447214,9.24488767133294));
#55273=CARTESIAN_POINT('Ctrl Pts',(20.2707977577484,3.7219238542422,8.99850535487191));
#55274=CARTESIAN_POINT('Ctrl Pts',(20.9685540112183,4.235972155578,8.76598582891085));
#55275=CARTESIAN_POINT('Ctrl Pts',(22.6570377008399,5.43415064582254,8.1180933488664));
#55276=CARTESIAN_POINT('Ctrl Pts',(23.7241254823866,6.21485531376477,7.52080745806043));
#55277=CARTESIAN_POINT('Ctrl Pts',(24.6950729185821,6.9548534027433,6.78592542456852));
#55278=CARTESIAN_POINT('Ctrl Pts',(2.1,-2.21221115744603,13.7368936516971));
#55279=CARTESIAN_POINT('Ctrl Pts',(2.73333333333333,-2.21221115744603,13.7368936516971));
#55280=CARTESIAN_POINT('Ctrl Pts',(3.36721312611028,-2.212274819488,13.7368878045733));
#55281=CARTESIAN_POINT('Ctrl Pts',(4.12624134471083,-2.21229370557991,13.7368861759272));
#55282=CARTESIAN_POINT('Ctrl Pts',(4.3860549636034,-2.21413081411987,13.7366102290359));
#55283=CARTESIAN_POINT('Ctrl Pts',(4.89391292370119,-2.22224402939692,13.7354015386744));
#55284=CARTESIAN_POINT('Ctrl Pts',(5.77025435885904,-2.24089536952233,13.7326445504079));
#55285=CARTESIAN_POINT('Ctrl Pts',(6.48769850774887,-2.24046786125482,13.7327531026294));
#55286=CARTESIAN_POINT('Ctrl Pts',(7.00643829240506,-2.21043597265355,13.7370420202613));
#55287=CARTESIAN_POINT('Ctrl Pts',(7.13275034169493,-2.20294627186771,13.7382060585672));
#55288=CARTESIAN_POINT('Ctrl Pts',(7.31833052215287,-2.19110496486678,13.7401615208733));
#55289=CARTESIAN_POINT('Ctrl Pts',(7.50526106344739,-2.17826120362336,13.7423748920571));
#55290=CARTESIAN_POINT('Ctrl Pts',(7.87736941114561,-2.15053462971115,13.7472402835191));
#55291=CARTESIAN_POINT('Ctrl Pts',(8.43154979519769,-2.10033857529429,13.7561031931122));
#55292=CARTESIAN_POINT('Ctrl Pts',(9.02547054687868,-2.02346233065752,13.7678309754653));
#55293=CARTESIAN_POINT('Ctrl Pts',(9.47898143432341,-1.94636277550259,13.7777315018726));
#55294=CARTESIAN_POINT('Ctrl Pts',(9.69689934795854,-1.90224417438758,13.7827387521995));
#55295=CARTESIAN_POINT('Ctrl Pts',(10.2969337278913,-1.76957263587484,13.7967587059728));
#55296=CARTESIAN_POINT('Ctrl Pts',(11.2522303770065,-1.4696861906153,13.8352459397839));
#55297=CARTESIAN_POINT('Ctrl Pts',(12.1683201134608,-1.07356159461314,13.8726526533793));
#55298=CARTESIAN_POINT('Ctrl Pts',(12.8911734653119,-0.746687011509429,
13.8874770909768));
#55299=CARTESIAN_POINT('Ctrl Pts',(13.3786074158793,-0.500607932547462,
13.8966643733047));
#55300=CARTESIAN_POINT('Ctrl Pts',(14.3384206267996,0.0584081193865376,
13.9098212945186));
#55301=CARTESIAN_POINT('Ctrl Pts',(15.0146615424652,0.519121115919698,13.9020742478091));
#55302=CARTESIAN_POINT('Ctrl Pts',(15.746048046055,1.02169095472785,13.86617557386));
#55303=CARTESIAN_POINT('Ctrl Pts',(16.242728877042,1.38808517145924,13.8334463689218));
#55304=CARTESIAN_POINT('Ctrl Pts',(17.2171396935533,2.1807240013221,13.7384313437697));
#55305=CARTESIAN_POINT('Ctrl Pts',(17.901644760173,2.79999400820501,13.6257148243664));
#55306=CARTESIAN_POINT('Ctrl Pts',(18.635036129223,3.45866556557441,13.4635963097359));
#55307=CARTESIAN_POINT('Ctrl Pts',(19.138368982942,3.93302752738387,13.3339158646569));
#55308=CARTESIAN_POINT('Ctrl Pts',(20.1238246490668,4.92585190997813,13.0127240131391));
#55309=CARTESIAN_POINT('Ctrl Pts',(20.8219879064555,5.67099230989098,12.7030107212261));
#55310=CARTESIAN_POINT('Ctrl Pts',(22.5097170303094,7.41023638571154,11.829789792395));
#55311=CARTESIAN_POINT('Ctrl Pts',(23.5814142719248,8.55489393715888,11.0112481940202));
#55312=CARTESIAN_POINT('Ctrl Pts',(24.5630597774301,9.65314473468797,9.98522809376511));
#55313=CARTESIAN_POINT('Ctrl Pts',(2.1,-4.38469435954868,23.2551644715195));
#55314=CARTESIAN_POINT('Ctrl Pts',(2.73333333333333,-4.38469435954868,23.2551644715195));
#55315=CARTESIAN_POINT('Ctrl Pts',(3.36769471511647,-4.38488057129456,23.2551532064746));
#55316=CARTESIAN_POINT('Ctrl Pts',(4.1272406751542,-4.38493601711281,23.2551502171888));
#55317=CARTESIAN_POINT('Ctrl Pts',(4.39371542805278,-4.38811237897684,23.2545870692032));
#55318=CARTESIAN_POINT('Ctrl Pts',(4.90597407671282,-4.40197836606138,23.2521437544136));
#55319=CARTESIAN_POINT('Ctrl Pts',(5.7807080208241,-4.43354775064731,23.2466189723673));
#55320=CARTESIAN_POINT('Ctrl Pts',(6.47526981917573,-4.43237909948388,23.2469264289471));
#55321=CARTESIAN_POINT('Ctrl Pts',(6.96712055433637,-4.38373884372307,23.2551815947408));
#55322=CARTESIAN_POINT('Ctrl Pts',(7.09309241227956,-4.37109334355141,23.2574951210814));
#55323=CARTESIAN_POINT('Ctrl Pts',(7.27497337036715,-4.351375704304,23.2613005282899));
#55324=CARTESIAN_POINT('Ctrl Pts',(7.45881576444989,-4.32994273678029,23.2655958831574));
#55325=CARTESIAN_POINT('Ctrl Pts',(7.82318936765134,-4.28381461113148,23.274992130574));
#55326=CARTESIAN_POINT('Ctrl Pts',(8.36312569624925,-4.20072544276082,23.2920454909141));
#55327=CARTESIAN_POINT('Ctrl Pts',(8.93510635605503,-4.07458377982203,23.3148346780207));
#55328=CARTESIAN_POINT('Ctrl Pts',(9.36759672724957,-3.94929372225073,23.3343645701841));
#55329=CARTESIAN_POINT('Ctrl Pts',(9.57394607457417,-3.87811577159792,23.3443682182037));
#55330=CARTESIAN_POINT('Ctrl Pts',(10.1400380810636,-3.66525566654609,23.3725990353288));
#55331=CARTESIAN_POINT('Ctrl Pts',(11.0614325554581,-3.17865730581794,23.4497905636272));
#55332=CARTESIAN_POINT('Ctrl Pts',(11.9722693017586,-2.51485712541299,23.532986674016));
#55333=CARTESIAN_POINT('Ctrl Pts',(12.6924963782862,-1.96359415406124,23.5743666485978));
#55334=CARTESIAN_POINT('Ctrl Pts',(13.175889377178,-1.55399509894084,23.6027261013292));
#55335=CARTESIAN_POINT('Ctrl Pts',(14.1420689046042,-0.604663058554355,
23.6550841747934));
#55336=CARTESIAN_POINT('Ctrl Pts',(14.8238605574682,0.181234839702475,23.6661844031786));
#55337=CARTESIAN_POINT('Ctrl Pts',(15.5572436616688,1.03764444286935,23.6307306769521));
#55338=CARTESIAN_POINT('Ctrl Pts',(16.0655714023431,1.67005225479606,23.594824522056));
#55339=CARTESIAN_POINT('Ctrl Pts',(17.0554148112706,3.03886141709287,23.4727037999293));
#55340=CARTESIAN_POINT('Ctrl Pts',(17.7492194074361,4.10701720329462,23.31031570719));
#55341=CARTESIAN_POINT('Ctrl Pts',(18.4856236416724,5.23721796897442,23.0659994842294));
#55342=CARTESIAN_POINT('Ctrl Pts',(19.0039934118869,6.06901762023052,22.8653268989984));
#55343=CARTESIAN_POINT('Ctrl Pts',(20.0037041464425,7.79468578904712,22.3590924212079));
#55344=CARTESIAN_POINT('Ctrl Pts',(20.70921584779,9.08661075029831,21.861654374002));
#55345=CARTESIAN_POINT('Ctrl Pts',(22.4031172629537,12.0907653827351,20.4503412208277));
#55346=CARTESIAN_POINT('Ctrl Pts',(23.5045174575955,14.1205525667797,19.0832753645027));
#55347=CARTESIAN_POINT('Ctrl Pts',(24.5018789378046,16.0600964495426,17.350084418661));
#55348=CARTESIAN_POINT('Ctrl Pts',(2.1,-6.55717756165133,32.7734352913419));
#55349=CARTESIAN_POINT('Ctrl Pts',(2.73333333333333,-6.55717756165133,32.7734352913419));
#55350=CARTESIAN_POINT('Ctrl Pts',(3.36823422033876,-6.55733365835752,32.7734302460344));
#55351=CARTESIAN_POINT('Ctrl Pts',(4.12831140060925,-6.55737729440761,32.7734296688118));
#55352=CARTESIAN_POINT('Ctrl Pts',(4.40146367837934,-6.56196909742548,32.7725602253241));
#55353=CARTESIAN_POINT('Ctrl Pts',(4.91806272527724,-6.58173623082086,32.76884327078));
#55354=CARTESIAN_POINT('Ctrl Pts',(5.79139783182175,-6.62612337659199,32.7605686737685));
#55355=CARTESIAN_POINT('Ctrl Pts',(6.46265872030445,-6.62323378721398,32.761262568013));
#55356=CARTESIAN_POINT('Ctrl Pts',(6.9289941766225,-6.55893905781572,32.772802106805));
#55357=CARTESIAN_POINT('Ctrl Pts',(7.05465117146563,-6.54117940276051,32.7762565405843));
#55358=CARTESIAN_POINT('Ctrl Pts',(7.23305738134067,-6.51402594214224,32.7818127633436));
#55359=CARTESIAN_POINT('Ctrl Pts',(7.41404715164792,-6.48440358817651,32.7881007548297));
#55360=CARTESIAN_POINT('Ctrl Pts',(7.77133867510313,-6.4209500807349,32.8017918588461));
#55361=CARTESIAN_POINT('Ctrl Pts',(8.29877981539897,-6.30710599255026,32.8265515875734));
#55362=CARTESIAN_POINT('Ctrl Pts',(8.85378665049961,-6.13594718228628,32.8595134623599));
#55363=CARTESIAN_POINT('Ctrl Pts',(9.2734143759592,-5.96649254262646,32.8879015674141));
#55364=CARTESIAN_POINT('Ctrl Pts',(9.47424581976662,-5.87008555018478,32.9025811140304));
#55365=CARTESIAN_POINT('Ctrl Pts',(10.0273490535427,-5.58086225664978,32.9443886029256));
#55366=CARTESIAN_POINT('Ctrl Pts',(10.95724978738,-4.89624833181571,33.0629975685759));
#55367=CARTESIAN_POINT('Ctrl Pts',(11.8781516205332,-3.94888311770831,33.1941309591058));
#55368=CARTESIAN_POINT('Ctrl Pts',(12.602064400414,-3.16718879965623,33.2625544037443));
#55369=CARTESIAN_POINT('Ctrl Pts',(13.0988694696214,-2.57261376786209,33.3120220678116));
#55370=CARTESIAN_POINT('Ctrl Pts',(14.0796924707411,-1.2066313810241,33.4035962308661));
#55371=CARTESIAN_POINT('Ctrl Pts',(14.7676661666682,-0.0828568772261278,
33.4312577852876));
#55372=CARTESIAN_POINT('Ctrl Pts',(15.5027143066566,1.13114584822823,33.3935159926964));
#55373=CARTESIAN_POINT('Ctrl Pts',(16.0202838183814,2.0480009213489,33.3515195947089));
#55374=CARTESIAN_POINT('Ctrl Pts',(17.0170397773181,4.00663252246451,33.1950226426635));
#55375=CARTESIAN_POINT('Ctrl Pts',(17.7141529625547,5.52939972439683,32.9767008794832));
#55376=CARTESIAN_POINT('Ctrl Pts',(18.4513779804965,7.13168519855837,32.6442892324621));
#55377=CARTESIAN_POINT('Ctrl Pts',(18.9741471075058,8.32767525987012,32.3665292176382));
#55378=CARTESIAN_POINT('Ctrl Pts',(19.976694090316,10.7868079909045,31.6647961243488));
#55379=CARTESIAN_POINT('Ctrl Pts',(20.6835910141171,12.6238140087707,30.9721601751623));
#55380=CARTESIAN_POINT('Ctrl Pts',(22.3784981023364,16.8857640647611,29.0059479969508));
#55381=CARTESIAN_POINT('Ctrl Pts',(23.4839952293235,19.7901269247353,27.0797142961554));
#55382=CARTESIAN_POINT('Ctrl Pts',(24.4831092917558,22.5567994415466,24.6338907495562));
#55383=CARTESIAN_POINT('Ctrl Pts',(2.1,-7.79859653428142,38.2124471883833));
#55384=CARTESIAN_POINT('Ctrl Pts',(2.73333333333333,-7.79859653428142,38.2124471883833));
#55385=CARTESIAN_POINT('Ctrl Pts',(3.36856062451574,-7.79873444591204,38.2124447399906));
#55386=CARTESIAN_POINT('Ctrl Pts',(4.12894455864879,-7.79877122896585,38.2124451854717));
#55387=CARTESIAN_POINT('Ctrl Pts',(4.40592023303614,-7.8041991375916,38.2113944348269));
#55388=CARTESIAN_POINT('Ctrl Pts',(4.92496378260879,-7.82740050255151,38.206935096053));
#55389=CARTESIAN_POINT('Ctrl Pts',(5.79760871146345,-7.87907393959177,38.1970978805761));
#55390=CARTESIAN_POINT('Ctrl Pts',(6.45531298767032,-7.87500898787854,38.1980539230733));
#55391=CARTESIAN_POINT('Ctrl Pts',(6.9077976809273,-7.80261420329609,38.2112781567269));
#55392=CARTESIAN_POINT('Ctrl Pts',(7.0332878180794,-7.78194383532455,38.215382261872));
#55393=CARTESIAN_POINT('Ctrl Pts',(7.20982673716659,-7.75066227156594,38.2219121181203));
#55394=CARTESIAN_POINT('Ctrl Pts',(7.389307620971,-7.7164659210836,38.2293156575816));
#55395=CARTESIAN_POINT('Ctrl Pts',(7.74288824317936,-7.64337852998469,38.245403215072));
#55396=CARTESIAN_POINT('Ctrl Pts',(8.26404052600409,-7.51246641850933,38.274457453936));
#55397=CARTESIAN_POINT('Ctrl Pts',(8.81154663884202,-7.31609326494859,38.3131349275136));
#55398=CARTESIAN_POINT('Ctrl Pts',(9.22663616903524,-7.12105996837216,38.3466696593823));
#55399=CARTESIAN_POINT('Ctrl Pts',(9.42600345931065,-7.00962245615174,38.3641521150841));
#55400=CARTESIAN_POINT('Ctrl Pts',(9.97673035450293,-6.67410993020777,38.4142586338593));
#55401=CARTESIAN_POINT('Ctrl Pts',(10.9140328205435,-5.86861558602685,38.5578683438277));
#55402=CARTESIAN_POINT('Ctrl Pts',(11.8387370187856,-4.75720739105203,38.7162552762356));
#55403=CARTESIAN_POINT('Ctrl Pts',(12.5644578213362,-3.84288974266347,38.7999538670138));
#55404=CARTESIAN_POINT('Ctrl Pts',(13.066322703487,-3.14070085828515,38.8614056110336));
#55405=CARTESIAN_POINT('Ctrl Pts',(14.0520220952575,-1.53711560165909,38.9747074705805));
#55406=CARTESIAN_POINT('Ctrl Pts',(14.7426079813353,-0.220446917943601,
39.0113449605053));
#55407=CARTESIAN_POINT('Ctrl Pts',(15.4784644022037,1.19801237275349,38.9717886737579));
#55408=CARTESIAN_POINT('Ctrl Pts',(15.9995803483975,2.27611610107773,38.925960287591));
#55409=CARTESIAN_POINT('Ctrl Pts',(16.9994385686868,4.56988282057309,38.7493359633624));
#55410=CARTESIAN_POINT('Ctrl Pts',(17.6981355886256,6.35201308463761,38.4986340630539));
#55411=CARTESIAN_POINT('Ctrl Pts',(18.4357025434826,8.22406759263825,38.1153991106372));
#55412=CARTESIAN_POINT('Ctrl Pts',(18.9608213396521,9.62691357240197,37.7935110674948));
#55413=CARTESIAN_POINT('Ctrl Pts',(19.9653436397241,12.5041437675931,36.97985111824));
#55414=CARTESIAN_POINT('Ctrl Pts',(20.6729453639354,14.6522661765941,36.1753281013235));
#55415=CARTESIAN_POINT('Ctrl Pts',(22.3680401919045,19.6325296413544,33.8910883575064));
#55416=CARTESIAN_POINT('Ctrl Pts',(23.4757593035169,23.0350551290633,31.6450395565025));
#55417=CARTESIAN_POINT('Ctrl Pts',(24.4767076204831,26.2741907223813,28.7915599578483));
#55418=CARTESIAN_POINT('',(3.2,-7.48695481785667,36.8470556158206));
#55419=CARTESIAN_POINT('Ctrl Pts',(3.2,-7.48695481785667,36.8470556158206));
#55420=CARTESIAN_POINT('Ctrl Pts',(3.45174020136192,-7.31395079566958,36.089075469184));
#55421=CARTESIAN_POINT('Ctrl Pts',(3.71840125365622,-7.13890531377323,35.3221511031575));
#55422=CARTESIAN_POINT('Ctrl Pts',(4.,-6.96288805731186,34.5509691145741));
#55423=CARTESIAN_POINT('Ctrl Pts',(4.62816480834395,-6.57024481011749,32.8306866476012));
#55424=CARTESIAN_POINT('Ctrl Pts',(5.32582966279889,-6.23689128633005,31.0992624735586));
#55425=CARTESIAN_POINT('Ctrl Pts',(6.03866106850362,-5.87030121037977,29.5163236792264));
#55426=CARTESIAN_POINT('Ctrl Pts',(6.32798217235993,-5.72151112539207,28.8738469369729));
#55427=CARTESIAN_POINT('Ctrl Pts',(6.61604116347502,-5.5677970636221,28.26345485931));
#55428=CARTESIAN_POINT('Ctrl Pts',(6.89476148100328,-5.40504398120696,27.6978623915459));
#55429=CARTESIAN_POINT('Ctrl Pts',(7.65522893079838,-4.96098442132935,26.1546858287526));
#55430=CARTESIAN_POINT('Ctrl Pts',(8.35226709607949,-4.55968381483506,24.9175441087371));
#55431=CARTESIAN_POINT('Ctrl Pts',(8.78926323826716,-4.29164296772241,24.1737483921843));
#55432=CARTESIAN_POINT('Ctrl Pts',(8.99031957410375,-4.16832080221034,23.8315374961511));
#55433=CARTESIAN_POINT('Ctrl Pts',(9.18275521560808,-4.04719763389059,23.5131938148023));
#55434=CARTESIAN_POINT('Ctrl Pts',(9.37496045132061,-3.92148904458358,23.203169428056));
#55435=CARTESIAN_POINT('Ctrl Pts',(9.48075232667821,-3.8522976546506,23.0325285963487));
#55436=CARTESIAN_POINT('Ctrl Pts',(9.58626090583131,-3.78183212273648,22.8648155089132));
#55437=CARTESIAN_POINT('Ctrl Pts',(9.69257910363365,-3.70887202431335,22.6982720777597));
#55438=CARTESIAN_POINT('Ctrl Pts',(10.0319880462582,-3.47595507903542,22.1666008207471));
#55439=CARTESIAN_POINT('Ctrl Pts',(10.3788056733388,-3.21653295379331,21.6469362728903));
#55440=CARTESIAN_POINT('Ctrl Pts',(10.7756849077178,-2.90649416731403,21.0798294966464));
#55441=CARTESIAN_POINT('Ctrl Pts',(10.8890930398495,-2.81790066929938,20.917778891218));
#55442=CARTESIAN_POINT('Ctrl Pts',(11.0576203517596,-2.68502865207462,20.6789427589835));
#55443=CARTESIAN_POINT('Ctrl Pts',(11.2725125491579,-2.51363785689445,20.3827664323304));
#55444=CARTESIAN_POINT('Ctrl Pts',(11.5968279592171,-2.25497478446942,19.9357769744012));
#55445=CARTESIAN_POINT('Ctrl Pts',(12.0255678842989,-1.90626438158956,19.3605597033925));
#55446=CARTESIAN_POINT('Ctrl Pts',(12.532035905153,-1.51672858576023,18.715758252655));
#55447=CARTESIAN_POINT('Ctrl Pts',(13.0988763178897,-1.08075904337671,17.9940946817688));
#55448=CARTESIAN_POINT('Ctrl Pts',(13.7495416923942,-0.541391711628421,
17.2086401181151));
#55449=CARTESIAN_POINT('Ctrl Pts',(14.4398764947203,0.0176411498964413,
16.421589811873));
#55450=CARTESIAN_POINT('Ctrl Pts',(14.7901814044069,0.301317933115872,16.0222073882751));
#55451=CARTESIAN_POINT('Ctrl Pts',(15.1459546156529,0.582681643644018,15.6283594122733));
#55452=CARTESIAN_POINT('Ctrl Pts',(15.4570717747561,0.815857706666163,15.2925887900305));
#55453=CARTESIAN_POINT('Ctrl Pts',(15.7998231395665,1.0727429716009,14.922677212769));
#55454=CARTESIAN_POINT('Ctrl Pts',(16.0676294472855,1.27727353930151,14.6416351637504));
#55455=CARTESIAN_POINT('Ctrl Pts',(16.3615307941354,1.50139670385469,14.3383117695221));
#55456=CARTESIAN_POINT('Ctrl Pts',(17.0296616001641,2.01089961082543,13.6487616669271));
#55457=CARTESIAN_POINT('Ctrl Pts',(17.7084691863034,2.53245724211085,12.9775795790632));
#55458=CARTESIAN_POINT('Ctrl Pts',(18.4207032016838,3.01739152515405,12.3152017758896));
#55459=CARTESIAN_POINT('Ctrl Pts',(18.8298642041348,3.29597439691827,11.9346819465985));
#55460=CARTESIAN_POINT('Ctrl Pts',(19.2113759271843,3.56048865862558,11.5875850942181));
#55461=CARTESIAN_POINT('Ctrl Pts',(19.5701113606338,3.80689943954097,11.2647488766695));
#55462=CARTESIAN_POINT('Ctrl Pts',(20.1215476021662,4.18567394083428,10.768495722294));
#55463=CARTESIAN_POINT('Ctrl Pts',(20.6514912602097,4.55442248629506,10.2954021170133));
#55464=CARTESIAN_POINT('Ctrl Pts',(21.3979544325339,5.00660433247608,9.65730708454375));
#55465=CARTESIAN_POINT('Ctrl Pts',(21.8107631282391,5.25666971421805,9.30442808413761));
#55466=CARTESIAN_POINT('Ctrl Pts',(22.3076315955878,5.54996514997988,8.88383089702849));
#55467=CARTESIAN_POINT('Ctrl Pts',(22.8472772295773,5.86208436754307,8.41699874974435));
#55468=CARTESIAN_POINT('Ctrl Pts',(23.3953136569067,6.17905663623287,7.94290796489216));
#55469=CARTESIAN_POINT('Ctrl Pts',(23.9608264583334,6.50100102939092,7.44199090360229));
#55470=CARTESIAN_POINT('Ctrl Pts',(24.5,6.80662575089405,6.93067919103514));
#55471=CARTESIAN_POINT('Ctrl Pts',(2.7976125197915,-7.69632218254969,37.764160171016));
#55472=CARTESIAN_POINT('Ctrl Pts',(2.93206640474696,-7.62662479454036,37.4587302040282));
#55473=CARTESIAN_POINT('Ctrl Pts',(3.06672620115017,-7.55684524328147,37.1529290248933));
#55474=CARTESIAN_POINT('Ctrl Pts',(3.20143890385924,-7.48704899610989,36.8470537203075));
#55475=CARTESIAN_POINT('Origin',(2.9,0.,0.));
#55476=CARTESIAN_POINT('Origin',(3.2,0.,0.));
#55477=CARTESIAN_POINT('Ctrl Pts',(2.09999999999999,5.34569526878069,8.14677776873086));
#55478=CARTESIAN_POINT('Ctrl Pts',(2.73333333333333,5.34569526878069,8.14677776873086));
#55479=CARTESIAN_POINT('Ctrl Pts',(3.36630034669941,5.34572932827768,8.14673820499258));
#55480=CARTESIAN_POINT('Ctrl Pts',(4.12415222295647,5.34573957275389,8.1467261713621));
#55481=CARTESIAN_POINT('Ctrl Pts',(4.36790021147292,5.34472553942211,8.14740587797417));
#55482=CARTESIAN_POINT('Ctrl Pts',(4.86512966195106,5.34009529004106,8.15052042278991));
#55483=CARTESIAN_POINT('Ctrl Pts',(5.74554670028596,5.32916987892461,8.15788640243843));
#55484=CARTESIAN_POINT('Ctrl Pts',(6.51831318247728,5.32899607663781,8.15800776496995));
#55485=CARTESIAN_POINT('Ctrl Pts',(7.10304257246599,5.34865471993144,8.1446302741035));
#55486=CARTESIAN_POINT('Ctrl Pts',(7.23019774633306,5.35310568763719,8.14167315323862));
#55487=CARTESIAN_POINT('Ctrl Pts',(7.42487767291169,5.36047814040294,8.13686977999796));
#55488=CARTESIAN_POINT('Ctrl Pts',(7.61944738538559,5.36848260168234,8.13172941156603));
#55489=CARTESIAN_POINT('Ctrl Pts',(8.01069407403727,5.38595279816171,8.120578662717));
#55490=CARTESIAN_POINT('Ctrl Pts',(8.60076076555801,5.41803622104533,8.10009941893901));
#55491=CARTESIAN_POINT('Ctrl Pts',(9.2514693452681,5.46730206741326,8.06707288500877));
#55492=CARTESIAN_POINT('Ctrl Pts',(9.76259388701861,5.51702797098133,8.03209010716476));
#55493=CARTESIAN_POINT('Ctrl Pts',(10.0140925250858,5.54573721585672,8.01129437931371));
#55494=CARTESIAN_POINT('Ctrl Pts',(10.7176766675203,5.63295501491629,7.94712173936429));
#55495=CARTESIAN_POINT('Ctrl Pts',(11.8207864606551,5.83200083591163,7.80546186007917));
#55496=CARTESIAN_POINT('Ctrl Pts',(12.8079685189794,6.07032563529004,7.62162237801202));
#55497=CARTESIAN_POINT('Ctrl Pts',(13.5603848523328,6.25130155066986,7.46780194988823));
#55498=CARTESIAN_POINT('Ctrl Pts',(14.1415274513423,6.40507133769525,7.3346969582253));
#55499=CARTESIAN_POINT('Ctrl Pts',(15.2007173823881,6.72668652876932,7.04487589906985));
#55500=CARTESIAN_POINT('Ctrl Pts',(15.9285144230346,6.97318784291672,6.80160018473738));
#55501=CARTESIAN_POINT('Ctrl Pts',(16.6747983655381,7.21490870896561,6.53624796834907));
#55502=CARTESIAN_POINT('Ctrl Pts',(17.2498259297328,7.41028452077371,6.31310610738743));
#55503=CARTESIAN_POINT('Ctrl Pts',(18.298502385672,7.7908485469562,5.84489796690035));
#55504=CARTESIAN_POINT('Ctrl Pts',(19.0237218101043,8.06049256566364,5.46513485251275));
#55505=CARTESIAN_POINT('Ctrl Pts',(19.7682624700467,8.31477089119449,5.0568703055287));
#55506=CARTESIAN_POINT('Ctrl Pts',(20.3332247834019,8.50943535027493,4.72383204545389));
#55507=CARTESIAN_POINT('Ctrl Pts',(21.3723657664017,8.86395000435395,4.03736317745124));
#55508=CARTESIAN_POINT('Ctrl Pts',(22.0962933246612,9.08773286473061,3.49670452915844));
#55509=CARTESIAN_POINT('Ctrl Pts',(23.230285826829,9.37695244520676,2.62988617519763));
#55510=CARTESIAN_POINT('Ctrl Pts',(23.8854423668127,9.50857067043872,2.08256115897413));
#55511=CARTESIAN_POINT('Ctrl Pts',(24.5000000001022,9.59462155805315,1.51911333273275));
#55512=CARTESIAN_POINT('Ctrl Pts',(2.09999999999999,7.95431935050272,11.4178889030821));
#55513=CARTESIAN_POINT('Ctrl Pts',(2.73333333333333,7.95431935050272,11.4178889030821));
#55514=CARTESIAN_POINT('Ctrl Pts',(3.36609905747045,7.95436068480874,11.4178460511122));
#55515=CARTESIAN_POINT('Ctrl Pts',(4.12372996076631,7.95437287171506,11.4178332681552));
#55516=CARTESIAN_POINT('Ctrl Pts',(4.36462463573312,7.95296242822486,11.4188381049305));
#55517=CARTESIAN_POINT('Ctrl Pts',(4.8599634841508,7.94649420404603,11.4234589089508));
#55518=CARTESIAN_POINT('Ctrl Pts',(5.7410868750954,7.93117831228565,11.4344193928147));
#55519=CARTESIAN_POINT('Ctrl Pts',(6.5236282796852,7.93082369663374,11.4346895818339));
#55520=CARTESIAN_POINT('Ctrl Pts',(7.11999518656519,7.95876090338528,11.4145500209094));
#55521=CARTESIAN_POINT('Ctrl Pts',(7.24729832679298,7.96500410071765,11.4101475403836));
#55522=CARTESIAN_POINT('Ctrl Pts',(7.44358223949712,7.97539578806132,11.4029609179064));
#55523=CARTESIAN_POINT('Ctrl Pts',(7.63949549354406,7.98667025085612,11.3952729249967));
#55524=CARTESIAN_POINT('Ctrl Pts',(8.03411141548379,8.01130481419146,11.3785737699017));
#55525=CARTESIAN_POINT('Ctrl Pts',(8.63043907126314,8.0565947486948,11.3478833478014));
#55526=CARTESIAN_POINT('Ctrl Pts',(9.29099904315616,8.12632114559454,11.2983139694396));
#55527=CARTESIAN_POINT('Ctrl Pts',(9.81198649015675,8.19688630646801,11.2457313990878));
#55528=CARTESIAN_POINT('Ctrl Pts',(10.0691598295132,8.23770627585821,11.2144385788119));
#55529=CARTESIAN_POINT('Ctrl Pts',(10.7900135369803,8.36185925360191,11.1178323753134));
#55530=CARTESIAN_POINT('Ctrl Pts',(11.9163064264562,8.64460860281135,10.9046196798766));
#55531=CARTESIAN_POINT('Ctrl Pts',(12.9132493179395,8.97978135610216,10.630613017264));
#55532=CARTESIAN_POINT('Ctrl Pts',(13.6696831671135,9.23283835425736,10.4027912554835));
#55533=CARTESIAN_POINT('Ctrl Pts',(14.2631240428071,9.45044991189978,10.2036164976331));
#55534=CARTESIAN_POINT('Ctrl Pts',(15.3328942858921,9.90158336336293,9.77293765230881));
#55535=CARTESIAN_POINT('Ctrl Pts',(16.0654073723091,10.2448029848828,9.41400445161443));
#55536=CARTESIAN_POINT('Ctrl Pts',(16.8131365772258,10.57901850791,9.02458364992901));
#55537=CARTESIAN_POINT('Ctrl Pts',(17.3939813143476,10.851263252928,8.69520722532973));
#55538=CARTESIAN_POINT('Ctrl Pts',(18.4452193504662,11.3765346858633,8.00852150865001));
#55539=CARTESIAN_POINT('Ctrl Pts',(19.1721170343286,11.7458521349479,7.45453132983995));
#55540=CARTESIAN_POINT('Ctrl Pts',(19.9174877328955,12.091418353064,6.86049809607568));
#55541=CARTESIAN_POINT('Ctrl Pts',(20.4827387246483,12.356087585852,6.37617988890529));
#55542=CARTESIAN_POINT('Ctrl Pts',(21.5195226714883,12.8327353582581,5.38177661181528));
#55543=CARTESIAN_POINT('Ctrl Pts',(22.2433987526262,13.1292643057035,4.60093146432436));
#55544=CARTESIAN_POINT('Ctrl Pts',(23.3781286077009,13.5049778910929,3.35041159552442));
#55545=CARTESIAN_POINT('Ctrl Pts',(24.0312127056184,13.6700047304202,2.56491139960509));
#55546=CARTESIAN_POINT('Ctrl Pts',(24.6419825553303,13.7690448953621,1.75959950001178));
#55547=CARTESIAN_POINT('Ctrl Pts',(2.09999999999999,14.0411088745208,19.0504815499016));
#55548=CARTESIAN_POINT('Ctrl Pts',(2.73333333333332,14.0411088745208,19.0504815499016));
#55549=CARTESIAN_POINT('Ctrl Pts',(3.36561005673443,14.0412263191859,19.0503511340209));
#55550=CARTESIAN_POINT('Ctrl Pts',(4.12272018987638,14.0412610463446,19.0503120245693));
#55551=CARTESIAN_POINT('Ctrl Pts',(4.35695331957966,14.0389612776608,19.0520444329267));
#55552=CARTESIAN_POINT('Ctrl Pts',(4.84789055187918,14.0282760040565,19.0601164814598));
#55553=CARTESIAN_POINT('Ctrl Pts',(5.73061998203781,14.0027176670903,19.0794536983509));
#55554=CARTESIAN_POINT('Ctrl Pts',(6.53603781131808,14.0017409829267,19.0801839394591));
#55555=CARTESIAN_POINT('Ctrl Pts',(7.15929021859793,14.0501390439893,19.0433328078394));
#55556=CARTESIAN_POINT('Ctrl Pts',(7.28693348498685,14.0605815697539,19.0355424902978));
#55557=CARTESIAN_POINT('Ctrl Pts',(7.48691623290952,14.078188038547,19.0226557527357));
#55558=CARTESIAN_POINT('Ctrl Pts',(7.68591744492013,14.0972533274485,19.0088897738562));
#55559=CARTESIAN_POINT('Ctrl Pts',(8.08826748913676,14.1390214221172,18.9789033544198));
#55560=CARTESIAN_POINT('Ctrl Pts',(8.69883992347527,14.2161182599971,18.923537563707));
#55561=CARTESIAN_POINT('Ctrl Pts',(9.38134013805784,14.3356504197161,18.8336195827372));
#55562=CARTESIAN_POINT('Ctrl Pts',(9.9233475627503,14.4574943433302,18.7376985909731));
#55563=CARTESIAN_POINT('Ctrl Pts',(10.1920889325272,14.5283291258725,18.680388177824));
#55564=CARTESIAN_POINT('Ctrl Pts',(10.9468888975129,14.7445321558586,18.5029076794783));
#55565=CARTESIAN_POINT('Ctrl Pts',(12.1070929839769,15.2320217055213,18.1136587205138));
#55566=CARTESIAN_POINT('Ctrl Pts',(13.1092959939513,15.7943764572631,17.6263674112012));
#55567=CARTESIAN_POINT('Ctrl Pts',(13.8683665989331,16.2161387424221,17.2240481534117));
#55568=CARTESIAN_POINT('Ctrl Pts',(14.465851216866,16.5827359029316,16.869477355448));
#55569=CARTESIAN_POINT('Ctrl Pts',(15.5292553024092,17.3293369894269,16.1151915443042));
#55570=CARTESIAN_POINT('Ctrl Pts',(16.2562016623198,17.8940957313968,15.4897104678438));
#55571=CARTESIAN_POINT('Ctrl Pts',(17.0019161442256,18.4429114016061,14.8108419597527));
#55572=CARTESIAN_POINT('Ctrl Pts',(17.5710904839668,18.8858158377931,14.2440758142749));
#55573=CARTESIAN_POINT('Ctrl Pts',(18.6068900718781,19.7375953416174,13.0645912504827));
#55574=CARTESIAN_POINT('Ctrl Pts',(19.324409219312,20.3350114167168,12.1131549555414));
#55575=CARTESIAN_POINT('Ctrl Pts',(20.0667073169345,20.8934110750517,11.088202506253));
#55576=CARTESIAN_POINT('Ctrl Pts',(20.6168193612055,21.3134200285188,10.2694650930084));
#55577=CARTESIAN_POINT('Ctrl Pts',(21.6393963370735,22.0716356556127,8.57762941163691));
#55578=CARTESIAN_POINT('Ctrl Pts',(22.3554514423905,22.5386470334874,7.24689507937901));
#55579=CARTESIAN_POINT('Ctrl Pts',(23.4866625010404,23.1218327822785,5.10639065291024));
#55580=CARTESIAN_POINT('Ctrl Pts',(24.1251846279709,23.3645442655133,3.78635366314737));
#55581=CARTESIAN_POINT('Ctrl Pts',(24.7276044279209,23.4996227468203,2.42994111486043));
#55582=CARTESIAN_POINT('Ctrl Pts',(2.09999999999999,20.1278983985389,26.6830741967211));
#55583=CARTESIAN_POINT('Ctrl Pts',(2.73333333333333,20.1278983985389,26.6830741967211));
#55584=CARTESIAN_POINT('Ctrl Pts',(3.3650650513931,20.1279907180548,26.6829648227731));
#55585=CARTESIAN_POINT('Ctrl Pts',(4.12164146402536,20.1280157003356,26.6829338985605));
#55586=CARTESIAN_POINT('Ctrl Pts',(4.34919679890247,20.1248892574282,26.6853459614754));
#55587=CARTESIAN_POINT('Ctrl Pts',(4.83579295504009,20.1101102777032,26.696777172012));
#55588=CARTESIAN_POINT('Ctrl Pts',(5.71992017424441,20.0742335862458,26.7245575404596));
#55589=CARTESIAN_POINT('Ctrl Pts',(6.54863427370623,20.0718789324825,26.7263949062999));
#55590=CARTESIAN_POINT('Ctrl Pts',(7.19739899140384,20.1431128638101,26.6709474908365));
#55591=CARTESIAN_POINT('Ctrl Pts',(7.32535704253212,20.1577873874664,26.6597421276243));
#55592=CARTESIAN_POINT('Ctrl Pts',(7.52881418015135,20.182960786228,26.6408726601145));
#55593=CARTESIAN_POINT('Ctrl Pts',(7.73066774801736,20.2101360022771,26.6207718311195));
#55594=CARTESIAN_POINT('Ctrl Pts',(8.14009928573882,20.2698930414322,26.5768039510723));
#55595=CARTESIAN_POINT('Ctrl Pts',(8.76316584740861,20.3805079701614,26.4953932538648));
#55596=CARTESIAN_POINT('Ctrl Pts',(9.46263854560405,20.5531886673258,26.3623600509603));
#55597=CARTESIAN_POINT('Ctrl Pts',(10.017507545926,20.7294232739755,26.2204349152997));
#55598=CARTESIAN_POINT('Ctrl Pts',(10.2917662953052,20.8316640419599,26.1358762893613));
#55599=CARTESIAN_POINT('Ctrl Pts',(11.0595542080066,21.1427939329773,25.8749304546139));
#55600=CARTESIAN_POINT('Ctrl Pts',(12.2112543073819,21.8258513926037,25.3167945268977));
#55601=CARTESIAN_POINT('Ctrl Pts',(13.2033940527264,22.6037886818375,24.6273187356927));
#55602=CARTESIAN_POINT('Ctrl Pts',(13.9587789479009,23.1900942266241,24.054937732768));
#55603=CARTESIAN_POINT('Ctrl Pts',(14.5428532084221,23.690775770569,23.5605522478501));
#55604=CARTESIAN_POINT('Ctrl Pts',(15.5916178900821,24.7164130754297,22.5032405024335));
#55605=CARTESIAN_POINT('Ctrl Pts',(16.3123893656982,25.4965693245089,21.6225906204811));
#55606=CARTESIAN_POINT('Ctrl Pts',(17.0564424910833,26.2597700017511,20.6589372504844));
#55607=CARTESIAN_POINT('Ctrl Pts',(17.616379707499,26.8641130888823,19.8710282227327));
#55608=CARTESIAN_POINT('Ctrl Pts',(18.6452710323621,28.039573237267,18.2139535665106));
#55609=CARTESIAN_POINT('Ctrl Pts',(19.3594959561944,28.8664279612339,16.8734755791401));
#55610=CARTESIAN_POINT('Ctrl Pts',(20.1009829497248,29.6419385160434,15.4217292188935));
#55611=CARTESIAN_POINT('Ctrl Pts',(20.6466969351181,30.2178627789357,14.2776672115503));
#55612=CARTESIAN_POINT('Ctrl Pts',(21.6664536129056,31.2654377485049,11.8953905111638));
#55613=CARTESIAN_POINT('Ctrl Pts',(22.3810862465992,31.9099310212778,10.0181473413673));
#55614=CARTESIAN_POINT('Ctrl Pts',(23.5117833300425,32.7123864767864,6.99078754096831));
#55615=CARTESIAN_POINT('Ctrl Pts',(24.1480627906507,33.0401645369321,5.13769400067936));
#55616=CARTESIAN_POINT('Ctrl Pts',(24.7493903499091,33.2186639686628,3.22959079971438));
#55617=CARTESIAN_POINT('Ctrl Pts',(2.09999999999999,23.6060638408349,31.0445557091894));
#55618=CARTESIAN_POINT('Ctrl Pts',(2.73333333333333,23.6060638408349,31.0445557091894));
#55619=CARTESIAN_POINT('Ctrl Pts',(3.36473746642767,23.6061425297296,31.0444589629108));
#55620=CARTESIAN_POINT('Ctrl Pts',(4.12100628902188,23.6061623402403,31.0444327844504));
#55621=CARTESIAN_POINT('Ctrl Pts',(4.34473822453751,23.6025854765119,31.0472157503264));
#55622=CARTESIAN_POINT('Ctrl Pts',(4.82888984385421,23.5855175045883,31.0605268452774));
#55623=CARTESIAN_POINT('Ctrl Pts',(5.71370711452889,23.5437141746986,31.0931560738764));
#55624=CARTESIAN_POINT('Ctrl Pts',(6.55597759920728,23.5404210020823,31.0957493072636));
#55625=CARTESIAN_POINT('Ctrl Pts',(7.21859239432847,23.6253815004145,31.0291339441544));
#55626=CARTESIAN_POINT('Ctrl Pts',(7.34671727862973,23.642483368885,31.0159694149875));
#55627=CARTESIAN_POINT('Ctrl Pts',(7.55204160508675,23.6720771362965,30.9936033840678));
#55628=CARTESIAN_POINT('Ctrl Pts',(7.75540399562257,23.703970579718,30.9698143809751));
#55629=CARTESIAN_POINT('Ctrl Pts',(8.1685462302919,23.7742182410811,30.9176848413218));
#55630=CARTESIAN_POINT('Ctrl Pts',(8.79790183526862,23.9043880616322,30.821062716188));
#55631=CARTESIAN_POINT('Ctrl Pts',(9.50487531095145,24.1078339771774,30.6630536225869));
#55632=CARTESIAN_POINT('Ctrl Pts',(10.0642822980701,24.3148700594436,30.4950542324297));
#55633=CARTESIAN_POINT('Ctrl Pts',(10.3400051840509,24.4345722367156,30.3953232126618));
#55634=CARTESIAN_POINT('Ctrl Pts',(11.1101689715184,24.7978712127453,30.0884174263745));
#55635=CARTESIAN_POINT('Ctrl Pts',(12.2544685115539,25.5868263762922,29.438979342731));
#55636=CARTESIAN_POINT('Ctrl Pts',(13.2428015568077,26.4868133212994,28.635622249399));
#55637=CARTESIAN_POINT('Ctrl Pts',(13.9963745203349,27.1666930320859,27.9669135540566));
#55638=CARTESIAN_POINT('Ctrl Pts',(14.5753856172388,27.7428627327012,27.3941772128234));
#55639=CARTESIAN_POINT('Ctrl Pts',(15.6192725488263,28.9287825114552,26.1637553334563));
#55640=CARTESIAN_POINT('Ctrl Pts',(16.3374308310286,29.8325152502563,25.1374605936698));
#55641=CARTESIAN_POINT('Ctrl Pts',(17.0806756556551,30.718544717149,24.0114822717043));
#55642=CARTESIAN_POINT('Ctrl Pts',(17.6370679821595,31.416219386984,23.0964177419519));
#55643=CARTESIAN_POINT('Ctrl Pts',(18.6628584031467,32.7782054424402,21.1652477398233));
#55644=CARTESIAN_POINT('Ctrl Pts',(19.3755147763723,33.7367580996321,19.6024095311255));
#55645=CARTESIAN_POINT('Ctrl Pts',(20.1166717274658,34.6367097434079,17.9070970149883));
#55646=CARTESIAN_POINT('Ctrl Pts',(20.6600520901303,35.3025782886813,16.5762223315018));
#55647=CARTESIAN_POINT('Ctrl Pts',(21.677838645414,36.5163042963535,13.7987400828508));
#55648=CARTESIAN_POINT('Ctrl Pts',(22.3918362246611,37.2627527205715,11.6092337566466));
#55649=CARTESIAN_POINT('Ctrl Pts',(23.5225266677048,38.1911612590058,8.07535257523923));
#55650=CARTESIAN_POINT('Ctrl Pts',(24.157514841919,38.568193396505,5.91726457407121));
#55651=CARTESIAN_POINT('Ctrl Pts',(24.7577717974218,38.7717600341623,3.69372680454323));
#55652=CARTESIAN_POINT('',(24.5,9.59462155813272,1.51911333283482));
#55653=CARTESIAN_POINT('Ctrl Pts',(24.5,9.59462155813272,1.51911333283482));
#55654=CARTESIAN_POINT('Ctrl Pts',(23.827493934627,9.68464608987473,2.15212334066745));
#55655=CARTESIAN_POINT('Ctrl Pts',(23.3366347313572,9.74051511545228,2.59560605191541));
#55656=CARTESIAN_POINT('Ctrl Pts',(22.5855494187791,9.82470025254072,3.28291903755242));
#55657=CARTESIAN_POINT('Ctrl Pts',(22.2454144273139,9.86282416523817,3.59417422067011));
#55658=CARTESIAN_POINT('Ctrl Pts',(21.8382660745341,9.90378919285794,3.97801649612276));
#55659=CARTESIAN_POINT('Ctrl Pts',(21.3802156951389,9.94963128619511,4.41815755084702));
#55660=CARTESIAN_POINT('Ctrl Pts',(20.7694693293574,10.0107553309835,5.0050243272898));
#55661=CARTESIAN_POINT('Ctrl Pts',(20.1629003033668,10.0735609707631,5.59681393246532));
#55662=CARTESIAN_POINT('Ctrl Pts',(19.5574857571565,10.1644416730676,6.18557724500365));
#55663=CARTESIAN_POINT('Ctrl Pts',(18.6418529412372,10.3018902261041,7.07602662905619));
#55664=CARTESIAN_POINT('Ctrl Pts',(17.7734813314344,10.4379301691332,8.01241566165726));
#55665=CARTESIAN_POINT('Ctrl Pts',(16.962125309797,10.6309468689446,8.90231278422673));
#55666=CARTESIAN_POINT('Ctrl Pts',(16.8133360661241,10.6663429318508,9.06550516375273));
#55667=CARTESIAN_POINT('Ctrl Pts',(16.6656205365448,10.7036307121431,9.22838814972182));
#55668=CARTESIAN_POINT('Ctrl Pts',(16.5183901926363,10.7431465007573,9.39150480786586));
#55669=CARTESIAN_POINT('Ctrl Pts',(15.7264522886848,10.9556981390766,10.2688936729658));
#55670=CARTESIAN_POINT('Ctrl Pts',(14.946225971903,11.1777141128626,11.2250100584366));
#55671=CARTESIAN_POINT('Ctrl Pts',(14.296315041466,11.4147273043975,12.0335028146403));
#55672=CARTESIAN_POINT('Ctrl Pts',(13.9908350933947,11.5261314584923,12.4135215427682));
#55673=CARTESIAN_POINT('Ctrl Pts',(13.7077063566838,11.640829979709,12.7699839203788));
#55674=CARTESIAN_POINT('Ctrl Pts',(13.4460198946299,11.7567579012083,13.1013811331617));
#55675=CARTESIAN_POINT('Ctrl Pts',(12.8373295403739,12.0264096327183,13.8722207297729));
#55676=CARTESIAN_POINT('Ctrl Pts',(12.3530827406682,12.2595769009129,14.5291392283553));
#55677=CARTESIAN_POINT('Ctrl Pts',(11.9770275685189,12.457891446445,15.0431152888451));
#55678=CARTESIAN_POINT('Ctrl Pts',(11.6553972427396,12.6275047814291,15.4827058064633));
#55679=CARTESIAN_POINT('Ctrl Pts',(11.368420561445,12.7915939796411,15.8816900946671));
#55680=CARTESIAN_POINT('Ctrl Pts',(11.0710856781132,12.9780838956265,16.2988272964875));
#55681=CARTESIAN_POINT('Ctrl Pts',(10.8141787015525,13.1392172276392,16.659247359313));
#55682=CARTESIAN_POINT('Ctrl Pts',(10.5576802661763,13.3127876314479,17.0222174418464));
#55683=CARTESIAN_POINT('Ctrl Pts',(10.2957959918397,13.5071054931829,17.3951211088922));
#55684=CARTESIAN_POINT('Ctrl Pts',(9.71459276345088,13.9383576898262,18.2227111416047));
#55685=CARTESIAN_POINT('Ctrl Pts',(9.09527967376,14.4765717245283,19.1169834509677));
#55686=CARTESIAN_POINT('Ctrl Pts',(8.43168033652509,15.1490772897656,20.1368903834754));
#55687=CARTESIAN_POINT('Ctrl Pts',(7.97964340480164,15.6071810509049,20.8316403245095));
#55688=CARTESIAN_POINT('Ctrl Pts',(7.52291961074447,16.1149117861986,21.5633911686948));
#55689=CARTESIAN_POINT('Ctrl Pts',(7.10363554125516,16.615783022346,22.2694187973217));
#55690=CARTESIAN_POINT('Ctrl Pts',(6.56327799554258,17.2612870411659,23.1793206618854));
#55691=CARTESIAN_POINT('Ctrl Pts',(6.08559840021217,17.920031801205,24.0135115916133));
#55692=CARTESIAN_POINT('Ctrl Pts',(5.61708670826502,18.6215531549853,24.8770749330837));
#55693=CARTESIAN_POINT('Ctrl Pts',(5.04102956502363,19.4841066278815,25.9388666451068));
#55694=CARTESIAN_POINT('Ctrl Pts',(4.50102820502663,20.3869529589021,27.0079183407073));
#55695=CARTESIAN_POINT('Ctrl Pts',(4.,21.2644490398942,28.1082636227258));
#55696=CARTESIAN_POINT('Ctrl Pts',(3.72183418897234,21.7516260223353,28.7191642361292));
#55697=CARTESIAN_POINT('Ctrl Pts',(3.45538353518276,22.241089434693,29.3329319419627));
#55698=CARTESIAN_POINT('Ctrl Pts',(3.2,22.7328514723457,29.9495820327475));
#55699=CARTESIAN_POINT('',(24.5,26.7974275967278,3.30119284473541));
#55700=CARTESIAN_POINT('Ctrl Pts',(24.5,26.7974275967278,3.30119284473543));
#55701=CARTESIAN_POINT('Ctrl Pts',(24.5,25.566267318827,3.1648258977828));
#55702=CARTESIAN_POINT('Ctrl Pts',(24.5,24.3558799941678,3.03166854152344));
#55703=CARTESIAN_POINT('Ctrl Pts',(24.5,19.3537663513507,2.48621193714647));
#55704=CARTESIAN_POINT('Ctrl Pts',(24.5,14.0423469702365,1.915931263191));
#55705=CARTESIAN_POINT('Ctrl Pts',(24.5,9.59462155813271,1.51911333283482));
#55706=CARTESIAN_POINT('',(10.2670750393577,21.2938329649397,26.7016219748491));
#55707=CARTESIAN_POINT('Ctrl Pts',(10.2670750393577,21.2938329649397,26.7016219748491));
#55708=CARTESIAN_POINT('Ctrl Pts',(11.2293198185888,21.1087322437254,25.7230189888652));
#55709=CARTESIAN_POINT('Ctrl Pts',(12.092802582344,21.2018541927487,24.7466295176431));
#55710=CARTESIAN_POINT('Ctrl Pts',(14.3080979519049,21.7464694747342,22.1165033038735));
#55711=CARTESIAN_POINT('Ctrl Pts',(14.8952017874601,21.9942012642266,21.3805031040621));
#55712=CARTESIAN_POINT('Ctrl Pts',(17.0803363586062,23.1363413672538,18.2402856712274));
#55713=CARTESIAN_POINT('Ctrl Pts',(17.6922811489506,23.4905403046472,17.2880492021451));
#55714=CARTESIAN_POINT('Ctrl Pts',(19.0755427322033,24.3513474737146,14.9508913369539));
#55715=CARTESIAN_POINT('Ctrl Pts',(20.2687424742408,25.0945348989029,12.841709283693));
#55716=CARTESIAN_POINT('Ctrl Pts',(22.3267279388309,26.1951510699121,8.4493984325661));
#55717=CARTESIAN_POINT('Ctrl Pts',(23.4192562717209,26.6465650740303,6.03375707119804));
#55718=CARTESIAN_POINT('Ctrl Pts',(24.5,26.7974275967278,3.30119284473544));
#55719=CARTESIAN_POINT('Ctrl Pts',(6.,23.5490023259382,31.0876903203335));
#55720=CARTESIAN_POINT('Ctrl Pts',(7.51604047332546,22.2062790886928,29.3988225104988));
#55721=CARTESIAN_POINT('Ctrl Pts',(9.08449301626627,21.6187658580324,27.8817144423825));
#55722=CARTESIAN_POINT('Ctrl Pts',(9.8624969752411,21.383187532576,27.1095892261748));
#55723=CARTESIAN_POINT('Ctrl Pts',(10.0667253012217,21.3323729308866,26.9053776680083));
#55724=CARTESIAN_POINT('Ctrl Pts',(10.2670750393577,21.2938329649397,26.7016219748491));
#55725=CARTESIAN_POINT('Origin',(24.5,5.29966331579924,6.64556760097825));
#55726=CARTESIAN_POINT('',(24.5,9.71413754081038,0.));
#55727=CARTESIAN_POINT('Ctrl Pts',(24.5,9.71413754081038,-6.93889390390723E-17));
#55728=CARTESIAN_POINT('Ctrl Pts',(24.5,9.71413754081038,0.274177179878995));
#55729=CARTESIAN_POINT('Ctrl Pts',(24.5,9.70252976905084,0.548413945873121));
#55730=CARTESIAN_POINT('Ctrl Pts',(24.5,9.65945653318739,1.05563169561816));
#55731=CARTESIAN_POINT('Ctrl Pts',(24.5,9.63118849993238,1.28815889347686));
#55732=CARTESIAN_POINT('Ctrl Pts',(24.5,9.59462155813272,1.51911333283482));
#55733=CARTESIAN_POINT('',(24.5,9.66248492718882,-1.00042650586162));
#55734=CARTESIAN_POINT('Ctrl Pts',(24.5,9.66248492718882,-1.00042650586162));
#55735=CARTESIAN_POINT('Ctrl Pts',(24.5,9.69691073862103,-0.667929433741795));
#55736=CARTESIAN_POINT('Ctrl Pts',(24.5,9.71413754081038,-0.334008932195348));
#55737=CARTESIAN_POINT('Ctrl Pts',(24.5,9.71413754081038,1.38777878078145E-16));
#55738=CARTESIAN_POINT('',(24.5,26.9302749158019,-1.93914748261464));
#55739=CARTESIAN_POINT('Ctrl Pts',(24.5,9.66248492718882,-1.00042650586161));
#55740=CARTESIAN_POINT('Ctrl Pts',(24.5,13.9671155781194,-1.16922793892204));
#55741=CARTESIAN_POINT('Ctrl Pts',(24.5,19.7062898477147,-1.49576285895545));
#55742=CARTESIAN_POINT('Ctrl Pts',(24.5,26.9302749158019,-1.93914748261464));
#55743=CARTESIAN_POINT('Origin',(24.5,0.,0.));
#55744=CARTESIAN_POINT('Ctrl Pts',(24.5,26.9302748955208,-1.93914776427185));
#55745=CARTESIAN_POINT('Ctrl Pts',(24.5,27.9515281336428,12.2436963424502));
#55746=CARTESIAN_POINT('Ctrl Pts',(24.5,16.8342246501858,21.1094500266368));
#55747=CARTESIAN_POINT('Ctrl Pts',(24.5,-4.275225376451,37.9436746768226));
#55748=CARTESIAN_POINT('Ctrl Pts',(24.5,-21.1094500266368,16.8342246501858));
#55749=CARTESIAN_POINT('Ctrl Pts',(24.5,-37.9436746768226,-4.275225376451));
#55750=CARTESIAN_POINT('Ctrl Pts',(24.5,-16.8342246501858,-21.1094500266368));
#55751=CARTESIAN_POINT('Ctrl Pts',(24.5,4.275225376451,-37.9436746768226));
#55752=CARTESIAN_POINT('Ctrl Pts',(24.5,21.1094500266368,-16.8342246501858));
#55753=CARTESIAN_POINT('Ctrl Pts',(24.5,26.329027592611,-10.2890814031001));
#55754=CARTESIAN_POINT('Ctrl Pts',(24.5,26.9302748955208,-1.93914776427185));
#55755=CARTESIAN_POINT('Ctrl Pts',(24.3078118955742,26.9629766761956,-1.94150249645076));
#55756=CARTESIAN_POINT('Ctrl Pts',(24.3078118955742,27.9854700353166,12.2585640210755));
#55757=CARTESIAN_POINT('Ctrl Pts',(24.3078118955742,16.854666666633,21.1350835044834));
#55758=CARTESIAN_POINT('Ctrl Pts',(24.3078118955742,-4.28041683785042,37.9897501711163));
#55759=CARTESIAN_POINT('Ctrl Pts',(24.3078118955742,-21.1350835044834,16.854666666633));
#55760=CARTESIAN_POINT('Ctrl Pts',(24.3078118955742,-37.9897501711163,-4.28041683785042));
#55761=CARTESIAN_POINT('Ctrl Pts',(24.3078118955742,-16.854666666633,-21.1350835044834));
#55762=CARTESIAN_POINT('Ctrl Pts',(24.3078118955742,4.28041683785042,-37.9897501711163));
#55763=CARTESIAN_POINT('Ctrl Pts',(24.3078118955742,21.1350835044834,-16.854666666633));
#55764=CARTESIAN_POINT('Ctrl Pts',(24.3078118955742,26.3609992709193,-10.3015755675561));
#55765=CARTESIAN_POINT('Ctrl Pts',(24.3078118955742,26.9629766761956,-1.94150249645076));
#55766=CARTESIAN_POINT('Ctrl Pts',(23.9225830034177,27.0325342181099,-1.94651107331878));
#55767=CARTESIAN_POINT('Ctrl Pts',(23.9225830034177,28.0576653469971,12.2901879619685));
#55768=CARTESIAN_POINT('Ctrl Pts',(23.9225830034177,16.8981473697169,21.1896065816043));
#55769=CARTESIAN_POINT('Ctrl Pts',(23.9225830034177,-4.29145921188742,38.0877539513211));
#55770=CARTESIAN_POINT('Ctrl Pts',(23.9225830034177,-21.1896065816043,16.8981473697169));
#55771=CARTESIAN_POINT('Ctrl Pts',(23.9225830034177,-38.0877539513211,-4.29145921188742));
#55772=CARTESIAN_POINT('Ctrl Pts',(23.9225830034177,-16.8981473697169,-21.1896065816043));
#55773=CARTESIAN_POINT('Ctrl Pts',(23.9225830034177,4.29145921188742,-38.0877539513211));
#55774=CARTESIAN_POINT('Ctrl Pts',(23.9225830034177,21.1896065816043,-16.8981473697169));
#55775=CARTESIAN_POINT('Ctrl Pts',(23.9225830034177,26.4290038660243,-10.3281509817965));
#55776=CARTESIAN_POINT('Ctrl Pts',(23.9225830034177,27.0325342181099,-1.94651107331878));
#55777=CARTESIAN_POINT('Ctrl Pts',(23.3421815947946,27.1493324306214,-1.95492127312333));
#55778=CARTESIAN_POINT('Ctrl Pts',(23.3421815947946,28.178892795868,12.3432896051147));
#55779=CARTESIAN_POINT('Ctrl Pts',(23.3421815947946,16.9711584086233,21.2811595286045));
#55780=CARTESIAN_POINT('Ctrl Pts',(23.3421815947946,-4.31000111998121,38.2523179372279));
#55781=CARTESIAN_POINT('Ctrl Pts',(23.3421815947946,-21.2811595286045,16.9711584086233));
#55782=CARTESIAN_POINT('Ctrl Pts',(23.3421815947946,-38.2523179372279,-4.31000111998121));
#55783=CARTESIAN_POINT('Ctrl Pts',(23.3421815947946,-16.9711584086233,-21.2811595286045));
#55784=CARTESIAN_POINT('Ctrl Pts',(23.3421815947946,4.31000111998121,-38.2523179372279));
#55785=CARTESIAN_POINT('Ctrl Pts',(23.3421815947946,21.2811595286045,-16.9711584086233));
#55786=CARTESIAN_POINT('Ctrl Pts',(23.3421815947946,26.5431944330316,-10.372775343075));
#55787=CARTESIAN_POINT('Ctrl Pts',(23.3421815947946,27.1493324306214,-1.95492127312333));
#55788=CARTESIAN_POINT('Ctrl Pts',(22.5631762070947,27.3300892320692,-1.96793689025922));
#55789=CARTESIAN_POINT('Ctrl Pts',(22.5631762070947,28.3665042792493,12.4254696570208));
#55790=CARTESIAN_POINT('Ctrl Pts',(22.5631762070947,17.0841502222764,21.4228467814061));
#55791=CARTESIAN_POINT('Ctrl Pts',(22.5631762070947,-4.33869655912967,38.5069970036825));
#55792=CARTESIAN_POINT('Ctrl Pts',(22.5631762070947,-21.4228467814061,17.0841502222764));
#55793=CARTESIAN_POINT('Ctrl Pts',(22.5631762070947,-38.5069970036825,-4.33869655912967));
#55794=CARTESIAN_POINT('Ctrl Pts',(22.5631762070947,-17.0841502222764,-21.4228467814061));
#55795=CARTESIAN_POINT('Ctrl Pts',(22.5631762070947,4.33869655912967,-38.5069970036825));
#55796=CARTESIAN_POINT('Ctrl Pts',(22.5631762070947,21.4228467814061,-17.0841502222764));
#55797=CARTESIAN_POINT('Ctrl Pts',(22.5631762070947,26.7199156448029,-10.4418359617087));
#55798=CARTESIAN_POINT('Ctrl Pts',(22.5631762070947,27.3300892320692,-1.96793689025922));
#55799=CARTESIAN_POINT('Ctrl Pts',(21.5808622776984,27.5984753948965,-1.98726236798372));
#55800=CARTESIAN_POINT('Ctrl Pts',(21.5808622776984,28.6450682155646,12.5474898997744));
#55801=CARTESIAN_POINT('Ctrl Pts',(21.5808622776984,17.2519195070522,21.633222810393));
#55802=CARTESIAN_POINT('Ctrl Pts',(21.5808622776984,-4.38130330334076,38.8851423174452));
#55803=CARTESIAN_POINT('Ctrl Pts',(21.5808622776984,-21.633222810393,17.2519195070522));
#55804=CARTESIAN_POINT('Ctrl Pts',(21.5808622776984,-38.8851423174452,-4.38130330334076));
#55805=CARTESIAN_POINT('Ctrl Pts',(21.5808622776984,-17.2519195070522,-21.633222810393));
#55806=CARTESIAN_POINT('Ctrl Pts',(21.5808622776984,4.38130330334076,-38.8851423174452));
#55807=CARTESIAN_POINT('Ctrl Pts',(21.5808622776984,21.633222810393,-17.2519195070522));
#55808=CARTESIAN_POINT('Ctrl Pts',(21.5808622776984,26.9823097983707,-10.5443765814205));
#55809=CARTESIAN_POINT('Ctrl Pts',(21.5808622776984,27.5984753948965,-1.98726236798372));
#55810=CARTESIAN_POINT('Ctrl Pts',(20.5902243197586,27.9104505809399,-2.00972652725693));
#55811=CARTESIAN_POINT('Ctrl Pts',(20.5902243197586,28.9688741634622,12.6893276440645));
#55812=CARTESIAN_POINT('Ctrl Pts',(20.5902243197586,17.4469364679823,21.8777663445708));
#55813=CARTESIAN_POINT('Ctrl Pts',(20.5902243197586,-4.43082987658852,39.3247028125531));
#55814=CARTESIAN_POINT('Ctrl Pts',(20.5902243197586,-21.8777663445708,17.4469364679823));
#55815=CARTESIAN_POINT('Ctrl Pts',(20.5902243197586,-39.3247028125531,-4.43082987658852));
#55816=CARTESIAN_POINT('Ctrl Pts',(20.5902243197586,-17.4469364679823,-21.8777663445708));
#55817=CARTESIAN_POINT('Ctrl Pts',(20.5902243197586,4.43082987658852,-39.3247028125531));
#55818=CARTESIAN_POINT('Ctrl Pts',(20.5902243197586,21.8777663445708,-17.4469364679823));
#55819=CARTESIAN_POINT('Ctrl Pts',(20.5902243197586,27.2873198034082,-10.6635709861342));
#55820=CARTESIAN_POINT('Ctrl Pts',(20.5902243197586,27.9104505809399,-2.00972652725693));
#55821=CARTESIAN_POINT('Ctrl Pts',(19.591895069338,28.2674884777214,-2.03543548277225));
#55822=CARTESIAN_POINT('Ctrl Pts',(19.591895069338,29.3394516958262,12.8516528935431));
#55823=CARTESIAN_POINT('Ctrl Pts',(19.591895069338,17.6701223131461,22.157632542334));
#55824=CARTESIAN_POINT('Ctrl Pts',(19.591895069338,-4.48751022918786,39.8277548554801));
#55825=CARTESIAN_POINT('Ctrl Pts',(19.591895069338,-22.157632542334,17.6701223131461));
#55826=CARTESIAN_POINT('Ctrl Pts',(19.591895069338,-39.8277548554801,-4.48751022918786));
#55827=CARTESIAN_POINT('Ctrl Pts',(19.591895069338,-17.6701223131461,-22.157632542334));
#55828=CARTESIAN_POINT('Ctrl Pts',(19.591895069338,4.48751022918786,-39.8277548554801));
#55829=CARTESIAN_POINT('Ctrl Pts',(19.591895069338,22.157632542334,-17.6701223131461));
#55830=CARTESIAN_POINT('Ctrl Pts',(19.591895069338,27.6363864457815,-10.7999822184082));
#55831=CARTESIAN_POINT('Ctrl Pts',(19.591895069338,28.2674884777214,-2.03543548277225));
#55832=CARTESIAN_POINT('Ctrl Pts',(18.5871162949016,28.6712831397633,-2.06451121702157));
#55833=CARTESIAN_POINT('Ctrl Pts',(18.5871162949016,29.7585591093251,13.0352358404652));
#55834=CARTESIAN_POINT('Ctrl Pts',(18.5871162949016,17.9225360029332,22.47414929801));
#55835=CARTESIAN_POINT('Ctrl Pts',(18.5871162949016,-4.55161329507687,40.3966853009432));
#55836=CARTESIAN_POINT('Ctrl Pts',(18.5871162949016,-22.47414929801,17.9225360029332));
#55837=CARTESIAN_POINT('Ctrl Pts',(18.5871162949016,-40.3966853009432,-4.55161329507687));
#55838=CARTESIAN_POINT('Ctrl Pts',(18.5871162949016,-17.9225360029332,-22.47414929801));
#55839=CARTESIAN_POINT('Ctrl Pts',(18.5871162949016,4.55161329507687,-40.3966853009432));
#55840=CARTESIAN_POINT('Ctrl Pts',(18.5871162949016,22.47414929801,-17.9225360029332));
#55841=CARTESIAN_POINT('Ctrl Pts',(18.5871162949016,28.0311659584264,-10.9542575150402));
#55842=CARTESIAN_POINT('Ctrl Pts',(18.5871162949016,28.6712831397633,-2.06451121702157));
#55843=CARTESIAN_POINT('Ctrl Pts',(17.577868433379,29.1235503979937,-2.09707728053386));
#55844=CARTESIAN_POINT('Ctrl Pts',(17.577868433379,30.2279773028415,13.2408565776054));
#55845=CARTESIAN_POINT('Ctrl Pts',(17.577868433379,18.2052501102534,22.8286615754873));
#55846=CARTESIAN_POINT('Ctrl Pts',(17.577868433379,-4.62341146523393,41.0339116857407));
#55847=CARTESIAN_POINT('Ctrl Pts',(17.577868433379,-22.8286615754873,18.2052501102534));
#55848=CARTESIAN_POINT('Ctrl Pts',(17.577868433379,-41.0339116857407,-4.62341146523393));
#55849=CARTESIAN_POINT('Ctrl Pts',(17.577868433379,-18.2052501102534,-22.8286615754873));
#55850=CARTESIAN_POINT('Ctrl Pts',(17.577868433379,4.62341146523393,-41.0339116857407));
#55851=CARTESIAN_POINT('Ctrl Pts',(17.577868433379,22.8286615754873,-18.2052501102534));
#55852=CARTESIAN_POINT('Ctrl Pts',(17.577868433379,28.4733358645036,-11.1270524328026));
#55853=CARTESIAN_POINT('Ctrl Pts',(17.577868433379,29.1235503979937,-2.09707728053386));
#55854=CARTESIAN_POINT('Ctrl Pts',(16.5668667015923,29.6257248204915,-2.1332369711586));
#55855=CARTESIAN_POINT('Ctrl Pts',(16.5668667015923,30.7491952463233,13.4691673231831));
#55856=CARTESIAN_POINT('Ctrl Pts',(16.5668667015923,18.5191613894625,23.2222938691605));
#55857=CARTESIAN_POINT('Ctrl Pts',(16.5668667015923,-4.703132479698,41.7414552586229));
#55858=CARTESIAN_POINT('Ctrl Pts',(16.5668667015923,-23.2222938691605,18.5191613894625));
#55859=CARTESIAN_POINT('Ctrl Pts',(16.5668667015923,-41.7414552586229,-4.703132479698));
#55860=CARTESIAN_POINT('Ctrl Pts',(16.5668667015923,-18.5191613894625,-23.2222938691605));
#55861=CARTESIAN_POINT('Ctrl Pts',(16.5668667015923,4.703132479698,-41.7414552586229));
#55862=CARTESIAN_POINT('Ctrl Pts',(16.5668667015923,23.2222938691605,-18.5191613894625));
#55863=CARTESIAN_POINT('Ctrl Pts',(16.5668667015923,28.964298703819,-11.3189150681333));
#55864=CARTESIAN_POINT('Ctrl Pts',(16.5668667015923,29.6257248204915,-2.1332369711586));
#55865=CARTESIAN_POINT('Ctrl Pts',(15.5576189940876,30.1786037710718,-2.17304770406385));
#55866=CARTESIAN_POINT('Ctrl Pts',(15.5576189940876,31.3230405413156,13.7205305941226));
#55867=CARTESIAN_POINT('Ctrl Pts',(15.5576189940876,18.8647682759327,23.6556711972172));
#55868=CARTESIAN_POINT('Ctrl Pts',(15.5576189940876,-4.79090292128452,42.5204394731498));
#55869=CARTESIAN_POINT('Ctrl Pts',(15.5576189940876,-23.6556711972172,18.8647682759327));
#55870=CARTESIAN_POINT('Ctrl Pts',(15.5576189940876,-42.5204394731498,-4.79090292128452));
#55871=CARTESIAN_POINT('Ctrl Pts',(15.5576189940876,-18.8647682759327,-23.6556711972172));
#55872=CARTESIAN_POINT('Ctrl Pts',(15.5576189940876,4.79090292128452,-42.5204394731498));
#55873=CARTESIAN_POINT('Ctrl Pts',(15.5576189940876,23.6556711972172,-18.8647682759327));
#55874=CARTESIAN_POINT('Ctrl Pts',(15.5576189940876,29.5048340381843,-11.5301500648294));
#55875=CARTESIAN_POINT('Ctrl Pts',(15.5576189940876,30.1786037710718,-2.17304770406385));
#55876=CARTESIAN_POINT('Ctrl Pts',(14.5544447688713,30.7820095946451,-2.2164966869751));
#55877=CARTESIAN_POINT('Ctrl Pts',(14.5544447688713,31.9493287956705,13.9948656205477));
#55878=CARTESIAN_POINT('Ctrl Pts',(14.5544447688713,19.2419597167431,24.1286543036994));
#55879=CARTESIAN_POINT('Ctrl Pts',(14.5544447688713,-4.88669458695623,43.3706140204425));
#55880=CARTESIAN_POINT('Ctrl Pts',(14.5544447688713,-24.1286543036994,19.2419597167431));
#55881=CARTESIAN_POINT('Ctrl Pts',(14.5544447688713,-43.3706140204425,-4.88669458695623));
#55882=CARTESIAN_POINT('Ctrl Pts',(14.5544447688713,-19.2419597167431,-24.1286543036994));
#55883=CARTESIAN_POINT('Ctrl Pts',(14.5544447688713,4.88669458695623,-43.3706140204425));
#55884=CARTESIAN_POINT('Ctrl Pts',(14.5544447688713,24.1286543036994,-19.2419597167431));
#55885=CARTESIAN_POINT('Ctrl Pts',(14.5544447688713,30.0947681788509,-11.760689547324));
#55886=CARTESIAN_POINT('Ctrl Pts',(14.5544447688713,30.7820095946451,-2.2164966869751));
#55887=CARTESIAN_POINT('Ctrl Pts',(13.5625963827217,31.4342268363874,-2.26346039644524));
#55888=CARTESIAN_POINT('Ctrl Pts',(13.5625963827217,32.6262795008725,14.2913924806776));
#55889=CARTESIAN_POINT('Ctrl Pts',(13.5625963827217,19.6496633740883,24.6398985195302));
#55890=CARTESIAN_POINT('Ctrl Pts',(13.5625963827217,-4.99023514544193,44.2895618936185));
#55891=CARTESIAN_POINT('Ctrl Pts',(13.5625963827217,-24.6398985195302,19.6496633740883));
#55892=CARTESIAN_POINT('Ctrl Pts',(13.5625963827217,-44.2895618936185,-4.99023514544193));
#55893=CARTESIAN_POINT('Ctrl Pts',(13.5625963827217,-19.6496633740883,-24.6398985195302));
#55894=CARTESIAN_POINT('Ctrl Pts',(13.5625963827217,4.99023514544193,-44.2895618936185));
#55895=CARTESIAN_POINT('Ctrl Pts',(13.5625963827217,24.6398985195302,-19.6496633740883));
#55896=CARTESIAN_POINT('Ctrl Pts',(13.5625963827217,30.7324239703655,-12.0098781025402));
#55897=CARTESIAN_POINT('Ctrl Pts',(13.5625963827217,31.4342268363874,-2.26346039644524));
#55898=CARTESIAN_POINT('Ctrl Pts',(12.5880795783847,32.1319937999165,-2.31370396999061));
#55899=CARTESIAN_POINT('Ctrl Pts',(12.5880795783847,33.3505072700831,14.6086282627996));
#55900=CARTESIAN_POINT('Ctrl Pts',(12.5880795783847,20.0858403482595,25.1868471453426));
#55901=CARTESIAN_POINT('Ctrl Pts',(12.5880795783847,-5.10100679708313,45.2726874936021));
#55902=CARTESIAN_POINT('Ctrl Pts',(12.5880795783847,-25.1868471453426,20.0858403482595));
#55903=CARTESIAN_POINT('Ctrl Pts',(12.5880795783847,-45.2726874936021,-5.10100679708313));
#55904=CARTESIAN_POINT('Ctrl Pts',(12.5880795783847,-20.0858403482595,-25.1868471453426));
#55905=CARTESIAN_POINT('Ctrl Pts',(12.5880795783847,5.10100679708313,-45.2726874936021));
#55906=CARTESIAN_POINT('Ctrl Pts',(12.5880795783847,25.1868471453426,-20.0858403482595));
#55907=CARTESIAN_POINT('Ctrl Pts',(12.5880795783847,31.4146125372199,-12.276469554577));
#55908=CARTESIAN_POINT('Ctrl Pts',(12.5880795783847,32.1319937999165,-2.31370396999061));
#55909=CARTESIAN_POINT('Ctrl Pts',(11.6370973936883,32.8712141860011,-2.36693244851678));
#55910=CARTESIAN_POINT('Ctrl Pts',(11.6370973936883,34.1177604637013,14.9447106077621));
#55911=CARTESIAN_POINT('Ctrl Pts',(11.6370973936883,20.5479300259039,25.766289273552));
#55912=CARTESIAN_POINT('Ctrl Pts',(11.6370973936883,-5.21835924764815,46.3142192994559));
#55913=CARTESIAN_POINT('Ctrl Pts',(11.6370973936883,-25.766289273552,20.5479300259039));
#55914=CARTESIAN_POINT('Ctrl Pts',(11.6370973936883,-46.3142192994559,-5.21835924764815));
#55915=CARTESIAN_POINT('Ctrl Pts',(11.6370973936883,-20.5479300259039,-25.766289273552));
#55916=CARTESIAN_POINT('Ctrl Pts',(11.6370973936883,5.21835924764815,-46.3142192994559));
#55917=CARTESIAN_POINT('Ctrl Pts',(11.6370973936883,25.766289273552,-20.5479300259039));
#55918=CARTESIAN_POINT('Ctrl Pts',(11.6370973936883,32.1373290344614,-12.5588988560514));
#55919=CARTESIAN_POINT('Ctrl Pts',(11.6370973936883,32.8712141860011,-2.36693244851678));
#55920=CARTESIAN_POINT('Ctrl Pts',(10.7155646400367,33.6474328922446,-2.42282503686346));
#55921=CARTESIAN_POINT('Ctrl Pts',(10.7155646400367,34.9234150323828,15.297614028594));
#55922=CARTESIAN_POINT('Ctrl Pts',(10.7155646400367,21.0331475043468,26.3747327466602));
#55923=CARTESIAN_POINT('Ctrl Pts',(10.7155646400367,-5.34158524231336,47.4078802510069));
#55924=CARTESIAN_POINT('Ctrl Pts',(10.7155646400367,-26.3747327466602,21.0331475043468));
#55925=CARTESIAN_POINT('Ctrl Pts',(10.7155646400367,-47.4078802510069,-5.34158524231336));
#55926=CARTESIAN_POINT('Ctrl Pts',(10.7155646400367,-21.0331475043468,-26.3747327466602));
#55927=CARTESIAN_POINT('Ctrl Pts',(10.7155646400367,5.34158524231336,-47.4078802510069));
#55928=CARTESIAN_POINT('Ctrl Pts',(10.7155646400367,26.3747327466602,-21.0331475043468));
#55929=CARTESIAN_POINT('Ctrl Pts',(10.7155646400367,32.8962178246381,-12.8554638739033));
#55930=CARTESIAN_POINT('Ctrl Pts',(10.7155646400367,33.6474328922446,-2.42282503686346));
#55931=CARTESIAN_POINT('Ctrl Pts',(9.82859575068344,34.456339097072,-2.48107132898941));
#55932=CARTESIAN_POINT('Ctrl Pts',(9.82859575068344,35.76299667904,15.66537863478));
#55933=CARTESIAN_POINT('Ctrl Pts',(9.82859575068344,21.5387980714436,27.0087985025163));
#55934=CARTESIAN_POINT('Ctrl Pts',(9.82859575068344,-5.47000043107262,48.5475965739599));
#55935=CARTESIAN_POINT('Ctrl Pts',(9.82859575068344,-27.0087985025163,21.5387980714436));
#55936=CARTESIAN_POINT('Ctrl Pts',(9.82859575068344,-48.5475965739599,-5.47000043107262));
#55937=CARTESIAN_POINT('Ctrl Pts',(9.82859575068344,-21.5387980714436,-27.0087985025163));
#55938=CARTESIAN_POINT('Ctrl Pts',(9.82859575068344,5.47000043107262,-48.5475965739599));
#55939=CARTESIAN_POINT('Ctrl Pts',(9.82859575068344,27.0087985025163,-21.5387980714436));
#55940=CARTESIAN_POINT('Ctrl Pts',(9.82859575068344,33.6870643298952,-13.1645175995423));
#55941=CARTESIAN_POINT('Ctrl Pts',(9.82859575068344,34.456339097072,-2.48107132898941));
#55942=CARTESIAN_POINT('Ctrl Pts',(8.97989469943246,35.2942458419803,-2.54140584088581));
#55943=CARTESIAN_POINT('Ctrl Pts',(8.97989469943246,36.6326786278703,16.0463281716024));
#55944=CARTESIAN_POINT('Ctrl Pts',(8.97989469943246,22.0625769943999,27.6655964976071));
#55945=CARTESIAN_POINT('Ctrl Pts',(8.97989469943246,-5.60301950320719,49.7281734920069));
#55946=CARTESIAN_POINT('Ctrl Pts',(8.97989469943246,-27.6655964976071,22.0625769943999));
#55947=CARTESIAN_POINT('Ctrl Pts',(8.97989469943246,-49.7281734920069,-5.60301950320719));
#55948=CARTESIAN_POINT('Ctrl Pts',(8.97989469943246,-22.0625769943999,-27.6655964976071));
#55949=CARTESIAN_POINT('Ctrl Pts',(8.97989469943246,5.60301950320719,-49.7281734920069));
#55950=CARTESIAN_POINT('Ctrl Pts',(8.97989469943246,27.6655964976071,-22.0625769943999));
#55951=CARTESIAN_POINT('Ctrl Pts',(8.97989469943246,34.506263907037,-13.4846513798329));
#55952=CARTESIAN_POINT('Ctrl Pts',(8.97989469943246,35.2942458419803,-2.54140584088581));
#55953=CARTESIAN_POINT('Ctrl Pts',(8.1713316609345,36.1584562373913,-2.60363437968177));
#55954=CARTESIAN_POINT('Ctrl Pts',(8.1713316609345,37.5296617175133,16.4392365135503));
#55955=CARTESIAN_POINT('Ctrl Pts',(8.1713316609345,22.6027984365433,28.3430127596098));
#55956=CARTESIAN_POINT('Ctrl Pts',(8.1713316609345,-5.74021432306655,50.9458111961531));
#55957=CARTESIAN_POINT('Ctrl Pts',(8.1713316609345,-28.3430127596098,22.6027984365433));
#55958=CARTESIAN_POINT('Ctrl Pts',(8.1713316609345,-50.9458111961531,-5.74021432306655));
#55959=CARTESIAN_POINT('Ctrl Pts',(8.1713316609345,-22.6027984365433,-28.3430127596098));
#55960=CARTESIAN_POINT('Ctrl Pts',(8.1713316609345,5.74021432306655,-50.9458111961531));
#55961=CARTESIAN_POINT('Ctrl Pts',(8.1713316609345,28.3430127596098,-22.6027984365433));
#55962=CARTESIAN_POINT('Ctrl Pts',(8.1713316609345,35.3511798774411,-13.8148348310708));
#55963=CARTESIAN_POINT('Ctrl Pts',(8.1713316609345,36.1584562373913,-2.60363437968177));
#55964=CARTESIAN_POINT('Ctrl Pts',(7.40358438374929,37.0470976022564,-2.66762210066133));
#55965=CARTESIAN_POINT('Ctrl Pts',(7.40358438374929,38.4520022508761,16.843252256834));
#55966=CARTESIAN_POINT('Ctrl Pts',(7.40358438374929,23.1582917773139,29.039579376772));
#55967=CARTESIAN_POINT('Ctrl Pts',(7.40358438374929,-5.88128759945806,52.1978711540859));
#55968=CARTESIAN_POINT('Ctrl Pts',(7.40358438374929,-29.039579376772,23.1582917773139));
#55969=CARTESIAN_POINT('Ctrl Pts',(7.40358438374929,-52.1978711540859,-5.88128759945806));
#55970=CARTESIAN_POINT('Ctrl Pts',(7.40358438374929,-23.1582917773139,-29.039579376772));
#55971=CARTESIAN_POINT('Ctrl Pts',(7.40358438374929,5.88128759945806,-52.1978711540859));
#55972=CARTESIAN_POINT('Ctrl Pts',(7.40358438374929,29.039579376772,-23.1582917773139));
#55973=CARTESIAN_POINT('Ctrl Pts',(7.40358438374929,36.2199813696739,-14.1543524697407));
#55974=CARTESIAN_POINT('Ctrl Pts',(7.40358438374929,37.0470976022564,-2.66762210066133));
#55975=CARTESIAN_POINT('Ctrl Pts',(6.82198164612729,37.7766337007775,-2.72015325007928));
#55976=CARTESIAN_POINT('Ctrl Pts',(6.82198164612729,39.209203908172,17.1749316955253));
#55977=CARTESIAN_POINT('Ctrl Pts',(6.82198164612729,23.6143277673129,29.6114304207775));
#55978=CARTESIAN_POINT('Ctrl Pts',(6.82198164612729,-5.99710265346455,53.2257581880904));
#55979=CARTESIAN_POINT('Ctrl Pts',(6.82198164612729,-29.6114304207775,23.6143277673129));
#55980=CARTESIAN_POINT('Ctrl Pts',(6.82198164612729,-53.2257581880904,-5.99710265346455));
#55981=CARTESIAN_POINT('Ctrl Pts',(6.82198164612729,-23.6143277673129,-29.6114304207775));
#55982=CARTESIAN_POINT('Ctrl Pts',(6.82198164612729,5.99710265346455,-53.2257581880904));
#55983=CARTESIAN_POINT('Ctrl Pts',(6.82198164612729,29.6114304207775,-23.6143277673129));
#55984=CARTESIAN_POINT('Ctrl Pts',(6.82198164612729,36.9332297914701,-14.4330817561407));
#55985=CARTESIAN_POINT('Ctrl Pts',(6.82198164612729,37.7766337007775,-2.72015325007928));
#55986=CARTESIAN_POINT('Ctrl Pts',(6.40395249919757,38.3340026926033,-2.76028729395988));
#55987=CARTESIAN_POINT('Ctrl Pts',(6.40395249919757,39.787709516313,17.4283363381844));
#55988=CARTESIAN_POINT('Ctrl Pts',(6.40395249919757,23.9627413968747,30.048327293349));
#55989=CARTESIAN_POINT('Ctrl Pts',(6.40395249919757,-6.08558589647433,54.0110686902236));
#55990=CARTESIAN_POINT('Ctrl Pts',(6.40395249919757,-30.048327293349,23.9627413968747));
#55991=CARTESIAN_POINT('Ctrl Pts',(6.40395249919757,-54.0110686902236,-6.08558589647433));
#55992=CARTESIAN_POINT('Ctrl Pts',(6.40395249919757,-23.9627413968747,-30.048327293349));
#55993=CARTESIAN_POINT('Ctrl Pts',(6.40395249919757,6.08558589647433,-54.0110686902236));
#55994=CARTESIAN_POINT('Ctrl Pts',(6.40395249919757,30.048327293349,-23.9627413968747));
#55995=CARTESIAN_POINT('Ctrl Pts',(6.40395249919757,37.4781549220891,-14.646032234764));
#55996=CARTESIAN_POINT('Ctrl Pts',(6.40395249919757,38.3340026926033,-2.76028729395988));
#55997=CARTESIAN_POINT('Ctrl Pts',(6.13331019225912,38.7101044651372,-2.78736896743619));
#55998=CARTESIAN_POINT('Ctrl Pts',(6.13331019225912,40.1780738670996,17.5993288703672));
#55999=CARTESIAN_POINT('Ctrl Pts',(6.13331019225912,24.1978441485076,30.3431368191721));
#56000=CARTESIAN_POINT('Ctrl Pts',(6.13331019225912,-6.14529267066447,54.5409809676797));
#56001=CARTESIAN_POINT('Ctrl Pts',(6.13331019225912,-30.3431368191721,24.1978441485076));
#56002=CARTESIAN_POINT('Ctrl Pts',(6.13331019225912,-54.5409809676797,-6.14529267066447));
#56003=CARTESIAN_POINT('Ctrl Pts',(6.13331019225912,-24.1978441485076,-30.3431368191721));
#56004=CARTESIAN_POINT('Ctrl Pts',(6.13331019225912,6.14529267066447,-54.5409809676797));
#56005=CARTESIAN_POINT('Ctrl Pts',(6.13331019225912,30.3431368191721,-24.1978441485076));
#56006=CARTESIAN_POINT('Ctrl Pts',(6.13331019225912,37.8458598187191,-14.7897270826059));
#56007=CARTESIAN_POINT('Ctrl Pts',(6.13331019225912,38.7101044651372,-2.78736896743619));
#56008=CARTESIAN_POINT('Ctrl Pts',(6.,38.8992859601968,-2.80099121505934));
#56009=CARTESIAN_POINT('Ctrl Pts',(6.,40.374429526373,17.6853391613169));
#56010=CARTESIAN_POINT('Ctrl Pts',(6.,24.3161022724906,30.4914278162532));
#56011=CARTESIAN_POINT('Ctrl Pts',(6.,-6.17532554376255,54.8075300887438));
#56012=CARTESIAN_POINT('Ctrl Pts',(6.,-30.4914278162532,24.3161022724906));
#56013=CARTESIAN_POINT('Ctrl Pts',(6.,-54.8075300887438,-6.17532554376255));
#56014=CARTESIAN_POINT('Ctrl Pts',(6.,-24.3161022724906,-30.4914278162532));
#56015=CARTESIAN_POINT('Ctrl Pts',(6.,6.17532554376255,-54.8075300887438));
#56016=CARTESIAN_POINT('Ctrl Pts',(6.,30.4914278162532,-24.3161022724906));
#56017=CARTESIAN_POINT('Ctrl Pts',(6.,38.0308176337714,-14.8620064711446));
#56018=CARTESIAN_POINT('Ctrl Pts',(6.,38.8992859601968,-2.80099121505934));
#56019=CARTESIAN_POINT('Ctrl Pts',(24.5,26.9302749158019,-1.93914748261463));
#56020=CARTESIAN_POINT('Ctrl Pts',(23.5178991898112,27.3082121037186,0.976729634524829));
#56021=CARTESIAN_POINT('Ctrl Pts',(22.3947886245986,27.292619732882,3.87921761795231));
#56022=CARTESIAN_POINT('Ctrl Pts',(21.1743874927566,26.982974376293,6.70537618061041));
#56023=CARTESIAN_POINT('Ctrl Pts',(20.5031871793443,26.8126745830804,8.25971635902861));
#56024=CARTESIAN_POINT('Ctrl Pts',(19.8411792966425,26.5351229273328,9.80106908179735));
#56025=CARTESIAN_POINT('Ctrl Pts',(19.1295827650289,26.1983895630578,11.3029592184858));
#56026=CARTESIAN_POINT('Ctrl Pts',(18.8261415870933,26.054798687939,11.9433998220584));
#56027=CARTESIAN_POINT('Ctrl Pts',(18.5104994276281,25.8995059296898,12.5819483349197));
#56028=CARTESIAN_POINT('Ctrl Pts',(18.2016639423759,25.7504555752122,13.1744818344469));
#56029=CARTESIAN_POINT('Ctrl Pts',(17.6747132403633,25.4961383329334,14.1854924159764));
#56030=CARTESIAN_POINT('Ctrl Pts',(17.2016343370993,25.234137247781,15.0794665673296));
#56031=CARTESIAN_POINT('Ctrl Pts',(16.872935292646,25.0561420993951,15.6789596275853));
#56032=CARTESIAN_POINT('Ctrl Pts',(16.6342454025477,24.9268881720619,16.1142907764943));
#56033=CARTESIAN_POINT('Ctrl Pts',(16.5014949770664,24.8554353423937,16.3490513597629));
#56034=CARTESIAN_POINT('Ctrl Pts',(16.3424569562979,24.7713057233,16.6271276317564));
#56035=CARTESIAN_POINT('Ctrl Pts',(15.993118510103,24.5865089667059,17.2379421546763));
#56036=CARTESIAN_POINT('Ctrl Pts',(15.6312480487537,24.4025072310428,17.842238323798));
#56037=CARTESIAN_POINT('Ctrl Pts',(15.2503296894305,24.2327051324582,18.4383275548583));
#56038=CARTESIAN_POINT('Ctrl Pts',(14.7484414179076,24.0089782375114,19.2237194545343));
#56039=CARTESIAN_POINT('Ctrl Pts',(14.2669345517206,23.7821697043648,19.9782075196444));
#56040=CARTESIAN_POINT('Ctrl Pts',(13.7912435751455,23.5895005313304,20.6850186190487));
#56041=CARTESIAN_POINT('Ctrl Pts',(13.5533980868579,23.4931659448132,21.0384241687508));
#56042=CARTESIAN_POINT('Ctrl Pts',(13.3161115657262,23.4047239475972,21.3818868765805));
#56043=CARTESIAN_POINT('Ctrl Pts',(13.0766514227367,23.3278398910295,21.7168098997672));
#56044=CARTESIAN_POINT('Ctrl Pts',(12.9188702359555,23.2771806976525,21.9374919365312));
#56045=CARTESIAN_POINT('Ctrl Pts',(12.760152636041,23.2315393210602,22.1544736717658));
#56046=CARTESIAN_POINT('Ctrl Pts',(12.5997389313808,23.1920716652435,22.3682108834076));
#56047=CARTESIAN_POINT('Ctrl Pts',(12.5166971934814,23.1716403514927,22.4788567259566));
#56048=CARTESIAN_POINT('Ctrl Pts',(12.4397215765388,23.1541581369635,22.5801970534995));
#56049=CARTESIAN_POINT('Ctrl Pts',(12.3478597934844,23.135666399718,22.6992700418308));
#56050=CARTESIAN_POINT('Ctrl Pts',(11.9116121727781,23.0478499421241,23.2647424953666));
#56051=CARTESIAN_POINT('Ctrl Pts',(10.7144663992386,22.7494221199229,24.8644224033158));
#56052=CARTESIAN_POINT('Ctrl Pts',(9.56604185022483,22.9954826851968,26.1397381390956));
#56053=CARTESIAN_POINT('Ctrl Pts',(9.07284645450935,23.1011543533655,26.687427449212));
#56054=CARTESIAN_POINT('Ctrl Pts',(8.57333454993108,23.2942014462969,27.200709354055));
#56055=CARTESIAN_POINT('Ctrl Pts',(8.00348148263612,23.5910390275427,27.7971969467927));
#56056=CARTESIAN_POINT('Ctrl Pts',(7.63919428966324,23.7807969413751,28.1785106630337));
#56057=CARTESIAN_POINT('Ctrl Pts',(7.24388644384776,24.0230902706367,28.5986372279999));
#56058=CARTESIAN_POINT('Ctrl Pts',(6.94254646282495,24.224686334644,28.9297076532741));
#56059=CARTESIAN_POINT('Ctrl Pts',(6.9143356486524,24.243559333442,28.9607017690026));
#56060=CARTESIAN_POINT('Ctrl Pts',(6.8866963504054,24.2622024336213,28.9911617715523));
#56061=CARTESIAN_POINT('Ctrl Pts',(6.85962514029879,24.2805982312137,29.0210854076675));
#56062=CARTESIAN_POINT('Ctrl Pts',(6.4400006207374,24.5657472029905,29.4849247180966));
#56063=CARTESIAN_POINT('Ctrl Pts',(6.15412442492902,24.8218403166442,29.7963100363863));
#56064=CARTESIAN_POINT('Ctrl Pts',(6.,24.9583551264995,29.9679914138325));
#56065=CARTESIAN_POINT('Ctrl Pts',(2.09999999999999,6.75186083300313,7.02307776555548));
#56066=CARTESIAN_POINT('Ctrl Pts',(2.73333333333332,6.75186083300313,7.02307776555548));
#56067=CARTESIAN_POINT('Ctrl Pts',(3.36743543952785,6.75183177141242,7.02311078228488));
#56068=CARTESIAN_POINT('Ctrl Pts',(4.25158796552468,6.75181603731384,7.02312801127863));
#56069=CARTESIAN_POINT('Ctrl Pts',(4.76433649975501,6.74814750679869,7.02673437605219));
#56070=CARTESIAN_POINT('Ctrl Pts',(5.76343391408727,6.73741073604095,7.03732555416368));
#56071=CARTESIAN_POINT('Ctrl Pts',(6.49282537630615,6.73758367376741,7.037202522005));
#56072=CARTESIAN_POINT('Ctrl Pts',(7.02318175216964,6.75287253869763,7.02196831057607));
#56073=CARTESIAN_POINT('Ctrl Pts',(7.14965217142688,6.75668208482572,7.01826529498886));
#56074=CARTESIAN_POINT('Ctrl Pts',(7.33684129238207,6.76279679807891,7.01243069802765));
#56075=CARTESIAN_POINT('Ctrl Pts',(7.52512455501651,6.76947383888626,7.00614752519297));
#56076=CARTESIAN_POINT('Ctrl Pts',(7.90060975758075,6.78395137112435,6.99260449234284));
#56077=CARTESIAN_POINT('Ctrl Pts',(8.46111568560639,6.81022178214197,6.96807725147119));
#56078=CARTESIAN_POINT('Ctrl Pts',(9.0649318004708,6.84956899053507,6.92958262645135));
#56079=CARTESIAN_POINT('Ctrl Pts',(9.52832373202331,6.8881411385333,6.89002179737934));
#56080=CARTESIAN_POINT('Ctrl Pts',(9.75191892912806,6.90990515851168,6.8670359880604));
#56081=CARTESIAN_POINT('Ctrl Pts',(10.3693392952773,6.9748999842145,6.79732375550614));
#56082=CARTESIAN_POINT('Ctrl Pts',(11.1025266505574,7.08737323265808,6.68172752983343));
#56083=CARTESIAN_POINT('Ctrl Pts',(12.0426911089806,7.26677575080387,6.48709341783056));
#56084=CARTESIAN_POINT('Ctrl Pts',(12.499722130795,7.3594489260534,6.38005936900193));
#56085=CARTESIAN_POINT('Ctrl Pts',(13.0012698578513,7.46041400993639,6.25761556166667));
#56086=CARTESIAN_POINT('Ctrl Pts',(13.5007180547461,7.57082916437595,6.12120949789655));
#56087=CARTESIAN_POINT('Ctrl Pts',(14.4711813662111,7.81513023260049,5.8104756958165));
#56088=CARTESIAN_POINT('Ctrl Pts',(15.1519969212886,8.00485912494299,5.54793502163326));
#56089=CARTESIAN_POINT('Ctrl Pts',(15.8847991347671,8.19595990286687,5.25102186548175));
#56090=CARTESIAN_POINT('Ctrl Pts',(16.3872971149165,8.33252921025319,5.0295981284336));
#56091=CARTESIAN_POINT('Ctrl Pts',(17.3643064948304,8.61235770932072,4.54363935262331));
#56092=CARTESIAN_POINT('Ctrl Pts',(18.0507589576911,8.80903169625677,4.14872708560309));
#56093=CARTESIAN_POINT('Ctrl Pts',(18.6483680950931,8.96006699947368,3.79286285126064));
#56094=CARTESIAN_POINT('Ctrl Pts',(18.9044434426896,9.02412347576023,3.63492996765564));
#56095=CARTESIAN_POINT('Ctrl Pts',(19.4121342092306,9.15024194464128,3.30386179229804));
#56096=CARTESIAN_POINT('Ctrl Pts',(20.2666508045858,9.35464157539163,2.70286662391449));
#56097=CARTESIAN_POINT('Ctrl Pts',(20.9684455414225,9.49456951845435,2.15371671276294));
#56098=CARTESIAN_POINT('Ctrl Pts',(22.6563363377109,9.73492158768411,0.813372498605933));
#56099=CARTESIAN_POINT('Ctrl Pts',(23.7241254823848,9.75490295250663,-0.169822791436732));
#56100=CARTESIAN_POINT('Ctrl Pts',(24.6950729185804,9.64173030469554,-1.20656804782375));
#56101=CARTESIAN_POINT('Ctrl Pts',(2.09999999999999,9.3606448320155,10.2943894298461));
#56102=CARTESIAN_POINT('Ctrl Pts',(2.73333333333332,9.3606448320155,10.2943894298461));
#56103=CARTESIAN_POINT('Ctrl Pts',(3.36780698153315,9.36061008131633,10.2944242783898));
#56104=CARTESIAN_POINT('Ctrl Pts',(4.25233231972465,9.36058995842981,10.2944437790382));
#56105=CARTESIAN_POINT('Ctrl Pts',(4.76998297705552,9.35518711781965,10.2994669666885));
#56106=CARTESIAN_POINT('Ctrl Pts',(5.76686224093397,9.33945332871658,10.3141494019522));
#56107=CARTESIAN_POINT('Ctrl Pts',(6.48740862524488,9.3398050883223,10.3138785526291));
#56108=CARTESIAN_POINT('Ctrl Pts',(7.0061130401074,9.36188714675425,10.2930675210009));
#56109=CARTESIAN_POINT('Ctrl Pts',(7.13243989848971,9.36746702831866,10.2879375119643));
#56110=CARTESIAN_POINT('Ctrl Pts',(7.31802664417342,9.37637918639968,10.279898312667));
#56111=CARTESIAN_POINT('Ctrl Pts',(7.5049699541733,9.38611799055235,10.2712361195763));
#56112=CARTESIAN_POINT('Ctrl Pts',(7.87708859115843,9.40720946420748,10.252591673622));
#56113=CARTESIAN_POINT('Ctrl Pts',(8.43135921890744,9.44543964035596,10.2188661544007));
#56114=CARTESIAN_POINT('Ctrl Pts',(9.02534159402558,9.50254288340357,10.1660693364088));
#56115=CARTESIAN_POINT('Ctrl Pts',(9.47887696115925,9.55835634760375,10.1119599660578));
#56116=CARTESIAN_POINT('Ctrl Pts',(9.69679911910571,9.58977777808015,10.0805889174017));
#56117=CARTESIAN_POINT('Ctrl Pts',(10.2969891502313,9.68347956139936,9.98557550000814));
#56118=CARTESIAN_POINT('Ctrl Pts',(11.0126425549871,9.84610155233706,9.82790341081631));
#56119=CARTESIAN_POINT('Ctrl Pts',(11.9399904897231,10.1078040659667,9.56020772764343));
#56120=CARTESIAN_POINT('Ctrl Pts',(12.3932824025843,10.243807857196,9.41208245856254));
#56121=CARTESIAN_POINT('Ctrl Pts',(12.8921398066301,10.3924251346088,9.24213401999094));
#56122=CARTESIAN_POINT('Ctrl Pts',(13.3792097412206,10.5529434552443,9.05554252681676));
#56123=CARTESIAN_POINT('Ctrl Pts',(14.3391036396927,10.9117909671869,8.6266652169495));
#56124=CARTESIAN_POINT('Ctrl Pts',(15.0151384665191,11.1929514360095,8.26160510734747));
#56125=CARTESIAN_POINT('Ctrl Pts',(15.7464682979872,11.4782327955903,7.84625032020446));
#56126=CARTESIAN_POINT('Ctrl Pts',(16.2431121097701,11.6811022331859,7.53930863556436));
#56127=CARTESIAN_POINT('Ctrl Pts',(17.2175647308135,12.1010374264068,6.86032054045774));
#56128=CARTESIAN_POINT('Ctrl Pts',(17.902233226602,12.3991880824743,6.30544044686097));
#56129=CARTESIAN_POINT('Ctrl Pts',(18.4992586458284,12.6303406807946,5.80396967282006));
#56130=CARTESIAN_POINT('Ctrl Pts',(18.7551887763511,12.7288128543355,5.58197357903342));
#56131=CARTESIAN_POINT('Ctrl Pts',(19.2633718823391,12.9238162767338,5.1151491998172));
#56132=CARTESIAN_POINT('Ctrl Pts',(20.11959381405,13.2431270393567,4.26551003148763));
#56133=CARTESIAN_POINT('Ctrl Pts',(20.8219603861067,13.4673930095846,3.48645537953313));
#56134=CARTESIAN_POINT('Ctrl Pts',(22.5090412631404,13.8688229753371,1.58275022437511));
#56135=CARTESIAN_POINT('Ctrl Pts',(23.5814142719244,13.9428296252028,0.176915545464796));
#56136=CARTESIAN_POINT('Ctrl Pts',(24.5630597774298,13.8254029813209,-1.32144457270545));
#56137=CARTESIAN_POINT('Ctrl Pts',(2.09999999999999,15.4478074963777,17.9274499798575));
#56138=CARTESIAN_POINT('Ctrl Pts',(2.73333333333332,15.4478074963777,17.9274499798575));
#56139=CARTESIAN_POINT('Ctrl Pts',(3.36868154479411,15.4477062395499,17.9275615025271));
#56140=CARTESIAN_POINT('Ctrl Pts',(4.25408340297134,15.4476482838215,17.9276224710576));
#56141=CARTESIAN_POINT('Ctrl Pts',(4.78315784529757,15.4380783144895,17.9360630069014));
#56142=CARTESIAN_POINT('Ctrl Pts',(5.77489961286181,15.410701705442,17.9602815974078));
#56143=CARTESIAN_POINT('Ctrl Pts',(6.47472773803472,15.4116671302561,17.9595561186054));
#56144=CARTESIAN_POINT('Ctrl Pts',(6.96650688012029,15.4484582579053,17.9266626909592));
#56145=CARTESIAN_POINT('Ctrl Pts',(7.09250370718804,15.4581514578408,17.9182183607075));
#56146=CARTESIAN_POINT('Ctrl Pts',(7.27439470054606,15.4734212590436,17.9051740564475));
#56147=CARTESIAN_POINT('Ctrl Pts',(7.45825749071973,15.4901434795058,17.8910941766856));
#56148=CARTESIAN_POINT('Ctrl Pts',(7.82264750929872,15.526250828117,17.8608873548829));
#56149=CARTESIAN_POINT('Ctrl Pts',(8.36272090805856,15.5913967531887,17.8065467726089));
#56150=CARTESIAN_POINT('Ctrl Pts',(8.9347937479117,15.6878654162987,17.7221276981452));
#56151=CARTESIAN_POINT('Ctrl Pts',(9.3673174608011,15.7812559606787,17.6363424287067));
#56152=CARTESIAN_POINT('Ctrl Pts',(9.57367322901424,15.8334515307549,17.5869341162243));
#56153=CARTESIAN_POINT('Ctrl Pts',(10.1399697938406,15.9882956088782,17.4380475272674));
#56154=CARTESIAN_POINT('Ctrl Pts',(10.8299043390251,16.260489724366,17.1894479356455));
#56155=CARTESIAN_POINT('Ctrl Pts',(11.7453472913653,16.7114886332834,16.7550898933566));
#56156=CARTESIAN_POINT('Ctrl Pts',(12.1960662260621,16.9479824207621,16.5125039644984));
#56157=CARTESIAN_POINT('Ctrl Pts',(12.6932389229874,17.2075602912353,16.2328252357149));
#56158=CARTESIAN_POINT('Ctrl Pts',(13.1762447636157,17.4848403459161,15.9305412231499));
#56159=CARTESIAN_POINT('Ctrl Pts',(14.1425321130376,18.1177228777731,15.2209165121274));
#56160=CARTESIAN_POINT('Ctrl Pts',(14.8241183447167,18.6162256731906,14.6135421497294));
#56161=CARTESIAN_POINT('Ctrl Pts',(15.557455076331,19.1224107044634,13.9219028509968));
#56162=CARTESIAN_POINT('Ctrl Pts',(16.0657546221985,19.488599800816,13.4050818951716));
#56163=CARTESIAN_POINT('Ctrl Pts',(17.0556206253738,20.2465726772756,12.2587322070762));
#56164=CARTESIAN_POINT('Ctrl Pts',(17.7495638140097,20.7856973165121,11.3220806623194));
#56165=CARTESIAN_POINT('Ctrl Pts',(18.3487436972501,21.2036838733817,10.4790901221427));
#56166=CARTESIAN_POINT('Ctrl Pts',(18.612025577843,21.3865661773176,10.0983329331232));
#56167=CARTESIAN_POINT('Ctrl Pts',(19.1297981766656,21.7465060383579,9.30187623430936));
#56168=CARTESIAN_POINT('Ctrl Pts',(20.0013796142357,22.3387585237374,7.85056974085133));
#56169=CARTESIAN_POINT('Ctrl Pts',(20.7092009017835,22.7574098818365,6.52651913010203));
#56170=CARTESIAN_POINT('Ctrl Pts',(22.4028783154293,23.5268367952951,3.29839169345834));
#56171=CARTESIAN_POINT('Ctrl Pts',(23.5047783389009,23.72392704974,0.858352285640053));
#56172=CARTESIAN_POINT('Ctrl Pts',(24.5021398191099,23.5781496343124,-1.7386710629416));
#56173=CARTESIAN_POINT('Ctrl Pts',(2.09999999999999,21.5349701607399,25.5605105298689));
#56174=CARTESIAN_POINT('Ctrl Pts',(2.73333333333332,21.5349701607399,25.5605105298689));
#56175=CARTESIAN_POINT('Ctrl Pts',(3.36960345513781,21.5349002841666,25.5605959908683));
#56176=CARTESIAN_POINT('Ctrl Pts',(4.25591992477685,21.5348462612853,25.5606536627902));
#56177=CARTESIAN_POINT('Ctrl Pts',(4.79634591585354,21.5209380941788,25.5726342271993));
#56178=CARTESIAN_POINT('Ctrl Pts',(5.78315002628676,21.4819997663131,25.6063230410257));
#56179=CARTESIAN_POINT('Ctrl Pts',(6.46185830361957,21.4843332331369,25.6044986864714));
#56180=CARTESIAN_POINT('Ctrl Pts',(6.92808305094846,21.5334571899302,25.5614101034119));
#56181=CARTESIAN_POINT('Ctrl Pts',(7.05377527389461,21.5472310736336,25.5496786575521));
#56182=CARTESIAN_POINT('Ctrl Pts',(7.23219486078965,21.5685063162337,25.5319120478409));
#56183=CARTESIAN_POINT('Ctrl Pts',(7.41321273751603,21.5918930045168,25.5126713718753));
#56184=CARTESIAN_POINT('Ctrl Pts',(7.7705268524474,21.6421607895434,25.4715965020036));
#56185=CARTESIAN_POINT('Ctrl Pts',(8.29815375808789,21.7325147198659,25.398009361424));
#56186=CARTESIAN_POINT('Ctrl Pts',(8.85328711712096,21.8650097997443,25.284732553375));
#56187=CARTESIAN_POINT('Ctrl Pts',(9.27295730736894,21.9928668513882,25.1699371658014));
#56188=CARTESIAN_POINT('Ctrl Pts',(9.47380151199838,22.0644476167393,25.1037197872101));
#56189=CARTESIAN_POINT('Ctrl Pts',(10.0271380233308,22.2775584376402,24.9035623188132));
#56190=CARTESIAN_POINT('Ctrl Pts',(10.7235476395157,22.6663647053173,24.558430698775));
#56191=CARTESIAN_POINT('Ctrl Pts',(11.6486669181634,23.3175089627325,23.9475902405967));
#56192=CARTESIAN_POINT('Ctrl Pts',(12.1028988094896,23.6583108207624,23.6066868035363));
#56193=CARTESIAN_POINT('Ctrl Pts',(12.6025767950092,24.0316536446078,23.2143131766174));
#56194=CARTESIAN_POINT('Ctrl Pts',(13.0990670491153,24.4407347347225,22.7806015625178));
#56195=CARTESIAN_POINT('Ctrl Pts',(14.0799893422845,25.3640794214541,21.7696578909302));
#56196=CARTESIAN_POINT('Ctrl Pts',(14.7677959112514,26.0861779345459,20.9084699059958));
#56197=CARTESIAN_POINT('Ctrl Pts',(15.5028074614617,26.813528756118,19.9358348179631));
#56198=CARTESIAN_POINT('Ctrl Pts',(16.0203496811134,27.3522973394796,19.1928465593642));
#56199=CARTESIAN_POINT('Ctrl Pts',(17.0171201090766,28.4511404827417,17.5639244958532));
#56200=CARTESIAN_POINT('Ctrl Pts',(17.714304440299,29.2299144264984,16.2370885097335));
#56201=CARTESIAN_POINT('Ctrl Pts',(18.3140531613331,29.8312119354217,15.0493462693643));
#56202=CARTESIAN_POINT('Ctrl Pts',(18.57968756902,30.0985577909357,14.5049533809244));
#56203=CARTESIAN_POINT('Ctrl Pts',(19.0999585250603,30.6210412827048,13.3731171359211));
#56204=CARTESIAN_POINT('Ctrl Pts',(19.9749323946637,31.4801887347959,11.312487340323));
#56205=CARTESIAN_POINT('Ctrl Pts',(20.6834701629094,32.0857292798578,9.4412256669571));
#56206=CARTESIAN_POINT('Ctrl Pts',(22.3781974839993,33.2055779658264,4.88365565359388));
#56207=CARTESIAN_POINT('Ctrl Pts',(23.4839952293235,33.5107154880467,1.41138142910537));
#56208=CARTESIAN_POINT('Ctrl Pts',(24.4831092917558,33.3234857380685,-2.27663628466851));
#56209=CARTESIAN_POINT('Ctrl Pts',(2.09999999999999,25.0133488260897,29.9222594155897));
#56210=CARTESIAN_POINT('Ctrl Pts',(2.73333333333332,25.0133488260897,29.9222594155897));
#56211=CARTESIAN_POINT('Ctrl Pts',(3.37014129606584,25.0132924435726,29.9223328973726));
#56212=CARTESIAN_POINT('Ctrl Pts',(4.25699410199334,25.013238335837,29.9223902997194));
#56213=CARTESIAN_POINT('Ctrl Pts',(4.80385941094312,24.9967713049222,29.9364568785204));
#56214=CARTESIAN_POINT('Ctrl Pts',(5.78794827479898,24.9512639339237,29.9755275020668));
#56215=CARTESIAN_POINT('Ctrl Pts',(6.45435104299642,24.9545226111096,29.9729588969588));
#56216=CARTESIAN_POINT('Ctrl Pts',(6.90670004343609,25.0100143695501,29.9245879403802));
#56217=CARTESIAN_POINT('Ctrl Pts',(7.03223126266704,25.0261109239331,29.9109859351108));
#56218=CARTESIAN_POINT('Ctrl Pts',(7.20878525009786,25.0507211873179,29.8905989614722));
#56219=CARTESIAN_POINT('Ctrl Pts',(7.38829842209633,25.0778317796888,29.8684778712122));
#56220=CARTESIAN_POINT('Ctrl Pts',(7.74190502196492,25.1359797339948,29.8213652053168));
#56221=CARTESIAN_POINT('Ctrl Pts',(8.2632681014489,25.2403315305653,29.7371132972183));
#56222=CARTESIAN_POINT('Ctrl Pts',(8.8109192265095,25.3930143580939,29.607688829357));
#56223=CARTESIAN_POINT('Ctrl Pts',(9.22605445875268,25.5408427231815,29.4761049361433));
#56224=CARTESIAN_POINT('Ctrl Pts',(9.42544001170288,25.6239850096632,29.3998849476721));
#56225=CARTESIAN_POINT('Ctrl Pts',(9.97639186033999,25.872447788317,29.1687118961422));
#56226=CARTESIAN_POINT('Ctrl Pts',(10.678683794887,26.3323373759567,28.7644662975497));
#56227=CARTESIAN_POINT('Ctrl Pts',(11.608086592202,27.1000368221737,28.0503563808397));
#56228=CARTESIAN_POINT('Ctrl Pts',(12.0639991264766,27.5009668734956,27.6525244186972));
#56229=CARTESIAN_POINT('Ctrl Pts',(12.5648057854578,27.9395988072145,27.1951930011199));
#56230=CARTESIAN_POINT('Ctrl Pts',(13.0664437052645,28.4251541066641,26.6848057324192));
#56231=CARTESIAN_POINT('Ctrl Pts',(14.0522205556053,29.5136387397641,25.5016363032258));
#56232=CARTESIAN_POINT('Ctrl Pts',(14.7426920220945,30.363042461303,24.4952111898507));
#56233=CARTESIAN_POINT('Ctrl Pts',(15.4785261743036,31.2164651060287,23.361578969675));
#56234=CARTESIAN_POINT('Ctrl Pts',(15.9996237268621,31.8527864292697,22.4901162997247));
#56235=CARTESIAN_POINT('Ctrl Pts',(16.9994960598944,33.1448484343335,20.5866268135138));
#56236=CARTESIAN_POINT('Ctrl Pts',(17.6982394889886,34.0600327208692,19.0367862273239));
#56237=CARTESIAN_POINT('Ctrl Pts',(18.298237166506,34.7657918685104,17.6517850800479));
#56238=CARTESIAN_POINT('Ctrl Pts',(18.5651091495521,35.0809389837737,17.0144403165625));
#56239=CARTESIAN_POINT('Ctrl Pts',(19.0868378278895,35.6957114841769,15.6915333342249));
#56240=CARTESIAN_POINT('Ctrl Pts',(19.9639555678099,36.7065474912943,13.2834565162864));
#56241=CARTESIAN_POINT('Ctrl Pts',(20.6728745268687,37.4184664294856,11.0994371626769));
#56242=CARTESIAN_POINT('Ctrl Pts',(22.3678114775293,38.7375406454473,5.7819285727616));
#56243=CARTESIAN_POINT('Ctrl Pts',(23.4757593035169,39.1032101474444,1.72082814260715));
#56244=CARTESIAN_POINT('Ctrl Pts',(24.4767076204831,38.8918379719078,-2.59074546980443));
#56245=CARTESIAN_POINT('Ctrl Pts',(23.5150942984749,10.0178765673373,5.37305195213122E-15));
#56246=CARTESIAN_POINT('Ctrl Pts',(23.8466145076669,9.90590446299441,-0.33185457075138));
#56247=CARTESIAN_POINT('Ctrl Pts',(24.1779623791327,9.78743932459042,-0.667296721337579));
#56248=CARTESIAN_POINT('Ctrl Pts',(24.5,9.66248492718882,-1.00042650586162));
#56249=CARTESIAN_POINT('Ctrl Pts',(2.79812873401693,24.7266395770977,29.5627865234736));
#56250=CARTESIAN_POINT('Ctrl Pts',(2.93275536019486,24.5313029720328,29.3178596635568));
#56251=CARTESIAN_POINT('Ctrl Pts',(3.06761573260946,24.3357274348763,29.0726369769539));
#56252=CARTESIAN_POINT('Ctrl Pts',(3.20253312029778,24.1401036614866,28.8273556403295));
#56253=CARTESIAN_POINT('Origin',(2.9,0.,0.));
#56254=CARTESIAN_POINT('Ctrl Pts',(27.,9.2,0.));
#56255=CARTESIAN_POINT('Ctrl Pts',(27.,9.2,9.2));
#56256=CARTESIAN_POINT('Ctrl Pts',(27.,0.,9.2));
#56257=CARTESIAN_POINT('Ctrl Pts',(27.,-9.2,9.2));
#56258=CARTESIAN_POINT('Ctrl Pts',(27.,-9.2,0.));
#56259=CARTESIAN_POINT('Ctrl Pts',(27.,-9.2,-9.2));
#56260=CARTESIAN_POINT('Ctrl Pts',(27.,0.,-9.2));
#56261=CARTESIAN_POINT('Ctrl Pts',(27.,9.2,-9.2));
#56262=CARTESIAN_POINT('Ctrl Pts',(27.,9.2,0.));
#56263=CARTESIAN_POINT('Ctrl Pts',(26.796570998452,9.22636560737002,0.));
#56264=CARTESIAN_POINT('Ctrl Pts',(26.796570998452,9.22636560737001,9.22636560737001));
#56265=CARTESIAN_POINT('Ctrl Pts',(26.796570998452,0.,9.22636560737002));
#56266=CARTESIAN_POINT('Ctrl Pts',(26.796570998452,-9.22636560737001,9.22636560737001));
#56267=CARTESIAN_POINT('Ctrl Pts',(26.796570998452,-9.22636560737002,0.));
#56268=CARTESIAN_POINT('Ctrl Pts',(26.796570998452,-9.22636560737001,-9.22636560737001));
#56269=CARTESIAN_POINT('Ctrl Pts',(26.796570998452,0.,-9.22636560737002));
#56270=CARTESIAN_POINT('Ctrl Pts',(26.796570998452,9.22636560737001,-9.22636560737001));
#56271=CARTESIAN_POINT('Ctrl Pts',(26.796570998452,9.22636560737002,0.));
#56272=CARTESIAN_POINT('Ctrl Pts',(26.3874085880356,9.28597940593777,0.));
#56273=CARTESIAN_POINT('Ctrl Pts',(26.3874085880356,9.28597940593777,9.28597940593777));
#56274=CARTESIAN_POINT('Ctrl Pts',(26.3874085880356,0.,9.28597940593777));
#56275=CARTESIAN_POINT('Ctrl Pts',(26.3874085880356,-9.28597940593777,9.28597940593777));
#56276=CARTESIAN_POINT('Ctrl Pts',(26.3874085880356,-9.28597940593777,0.));
#56277=CARTESIAN_POINT('Ctrl Pts',(26.3874085880356,-9.28597940593777,-9.28597940593777));
#56278=CARTESIAN_POINT('Ctrl Pts',(26.3874085880356,0.,-9.28597940593777));
#56279=CARTESIAN_POINT('Ctrl Pts',(26.3874085880356,9.28597940593777,-9.28597940593777));
#56280=CARTESIAN_POINT('Ctrl Pts',(26.3874085880356,9.28597940593777,0.));
#56281=CARTESIAN_POINT('Ctrl Pts',(25.7667517823113,9.39604887090672,0.));
#56282=CARTESIAN_POINT('Ctrl Pts',(25.7667517823113,9.39604887090672,9.39604887090672));
#56283=CARTESIAN_POINT('Ctrl Pts',(25.7667517823113,0.,9.39604887090672));
#56284=CARTESIAN_POINT('Ctrl Pts',(25.7667517823113,-9.39604887090672,9.39604887090672));
#56285=CARTESIAN_POINT('Ctrl Pts',(25.7667517823113,-9.39604887090672,0.));
#56286=CARTESIAN_POINT('Ctrl Pts',(25.7667517823113,-9.39604887090672,-9.39604887090672));
#56287=CARTESIAN_POINT('Ctrl Pts',(25.7667517823113,0.,-9.39604887090672));
#56288=CARTESIAN_POINT('Ctrl Pts',(25.7667517823113,9.39604887090672,-9.39604887090672));
#56289=CARTESIAN_POINT('Ctrl Pts',(25.7667517823113,9.39604887090672,0.));
#56290=CARTESIAN_POINT('Ctrl Pts',(24.9253466419639,9.58420457526839,0.));
#56291=CARTESIAN_POINT('Ctrl Pts',(24.9253466419639,9.58420457526839,9.58420457526839));
#56292=CARTESIAN_POINT('Ctrl Pts',(24.9253466419639,0.,9.58420457526839));
#56293=CARTESIAN_POINT('Ctrl Pts',(24.9253466419639,-9.58420457526839,9.58420457526839));
#56294=CARTESIAN_POINT('Ctrl Pts',(24.9253466419639,-9.58420457526839,0.));
#56295=CARTESIAN_POINT('Ctrl Pts',(24.9253466419639,-9.58420457526839,-9.58420457526839));
#56296=CARTESIAN_POINT('Ctrl Pts',(24.9253466419639,0.,-9.58420457526839));
#56297=CARTESIAN_POINT('Ctrl Pts',(24.9253466419639,9.58420457526839,-9.58420457526839));
#56298=CARTESIAN_POINT('Ctrl Pts',(24.9253466419639,9.58420457526839,0.));
#56299=CARTESIAN_POINT('Ctrl Pts',(23.8505404645239,9.89058631634017,0.));
#56300=CARTESIAN_POINT('Ctrl Pts',(23.8505404645239,9.89058631634017,9.89058631634017));
#56301=CARTESIAN_POINT('Ctrl Pts',(23.8505404645239,0.,9.89058631634017));
#56302=CARTESIAN_POINT('Ctrl Pts',(23.8505404645239,-9.89058631634017,9.89058631634017));
#56303=CARTESIAN_POINT('Ctrl Pts',(23.8505404645239,-9.89058631634017,0.));
#56304=CARTESIAN_POINT('Ctrl Pts',(23.8505404645239,-9.89058631634017,-9.89058631634017));
#56305=CARTESIAN_POINT('Ctrl Pts',(23.8505404645239,0.,-9.89058631634017));
#56306=CARTESIAN_POINT('Ctrl Pts',(23.8505404645239,9.89058631634017,-9.89058631634017));
#56307=CARTESIAN_POINT('Ctrl Pts',(23.8505404645239,9.89058631634017,0.));
#56308=CARTESIAN_POINT('Ctrl Pts',(22.7532142104752,10.273481509771,0.));
#56309=CARTESIAN_POINT('Ctrl Pts',(22.7532142104752,10.273481509771,10.273481509771));
#56310=CARTESIAN_POINT('Ctrl Pts',(22.7532142104752,0.,10.273481509771));
#56311=CARTESIAN_POINT('Ctrl Pts',(22.7532142104752,-10.273481509771,10.273481509771));
#56312=CARTESIAN_POINT('Ctrl Pts',(22.7532142104752,-10.273481509771,0.));
#56313=CARTESIAN_POINT('Ctrl Pts',(22.7532142104752,-10.273481509771,-10.273481509771));
#56314=CARTESIAN_POINT('Ctrl Pts',(22.7532142104752,0.,-10.273481509771));
#56315=CARTESIAN_POINT('Ctrl Pts',(22.7532142104752,10.273481509771,-10.273481509771));
#56316=CARTESIAN_POINT('Ctrl Pts',(22.7532142104752,10.273481509771,0.));
#56317=CARTESIAN_POINT('Ctrl Pts',(21.6347255505832,10.7430346646081,0.));
#56318=CARTESIAN_POINT('Ctrl Pts',(21.6347255505832,10.7430346646081,10.7430346646081));
#56319=CARTESIAN_POINT('Ctrl Pts',(21.6347255505832,0.,10.7430346646081));
#56320=CARTESIAN_POINT('Ctrl Pts',(21.6347255505832,-10.7430346646081,10.7430346646081));
#56321=CARTESIAN_POINT('Ctrl Pts',(21.6347255505832,-10.7430346646081,0.));
#56322=CARTESIAN_POINT('Ctrl Pts',(21.6347255505832,-10.7430346646081,-10.7430346646081));
#56323=CARTESIAN_POINT('Ctrl Pts',(21.6347255505832,0.,-10.7430346646081));
#56324=CARTESIAN_POINT('Ctrl Pts',(21.6347255505832,10.7430346646081,-10.7430346646081));
#56325=CARTESIAN_POINT('Ctrl Pts',(21.6347255505832,10.7430346646081,0.));
#56326=CARTESIAN_POINT('Ctrl Pts',(20.4975894383762,11.3145134298179,0.));
#56327=CARTESIAN_POINT('Ctrl Pts',(20.4975894383762,11.3145134298179,11.3145134298179));
#56328=CARTESIAN_POINT('Ctrl Pts',(20.4975894383762,0.,11.3145134298179));
#56329=CARTESIAN_POINT('Ctrl Pts',(20.4975894383762,-11.3145134298179,11.3145134298179));
#56330=CARTESIAN_POINT('Ctrl Pts',(20.4975894383762,-11.3145134298179,0.));
#56331=CARTESIAN_POINT('Ctrl Pts',(20.4975894383762,-11.3145134298179,-11.3145134298179));
#56332=CARTESIAN_POINT('Ctrl Pts',(20.4975894383762,0.,-11.3145134298179));
#56333=CARTESIAN_POINT('Ctrl Pts',(20.4975894383762,11.3145134298179,-11.3145134298179));
#56334=CARTESIAN_POINT('Ctrl Pts',(20.4975894383762,11.3145134298179,0.));
#56335=CARTESIAN_POINT('Ctrl Pts',(19.3456615791409,12.0038530129696,0.));
#56336=CARTESIAN_POINT('Ctrl Pts',(19.3456615791409,12.0038530129696,12.0038530129696));
#56337=CARTESIAN_POINT('Ctrl Pts',(19.3456615791409,0.,12.0038530129696));
#56338=CARTESIAN_POINT('Ctrl Pts',(19.3456615791409,-12.0038530129696,12.0038530129696));
#56339=CARTESIAN_POINT('Ctrl Pts',(19.3456615791409,-12.0038530129696,0.));
#56340=CARTESIAN_POINT('Ctrl Pts',(19.3456615791409,-12.0038530129696,-12.0038530129696));
#56341=CARTESIAN_POINT('Ctrl Pts',(19.3456615791409,0.,-12.0038530129696));
#56342=CARTESIAN_POINT('Ctrl Pts',(19.3456615791409,12.0038530129696,-12.0038530129696));
#56343=CARTESIAN_POINT('Ctrl Pts',(19.3456615791409,12.0038530129696,0.));
#56344=CARTESIAN_POINT('Ctrl Pts',(18.1843885347784,12.8237912132616,0.));
#56345=CARTESIAN_POINT('Ctrl Pts',(18.1843885347784,12.8237912132616,12.8237912132616));
#56346=CARTESIAN_POINT('Ctrl Pts',(18.1843885347784,0.,12.8237912132616));
#56347=CARTESIAN_POINT('Ctrl Pts',(18.1843885347784,-12.8237912132616,12.8237912132616));
#56348=CARTESIAN_POINT('Ctrl Pts',(18.1843885347784,-12.8237912132616,0.));
#56349=CARTESIAN_POINT('Ctrl Pts',(18.1843885347784,-12.8237912132616,-12.8237912132616));
#56350=CARTESIAN_POINT('Ctrl Pts',(18.1843885347784,0.,-12.8237912132616));
#56351=CARTESIAN_POINT('Ctrl Pts',(18.1843885347784,12.8237912132616,-12.8237912132616));
#56352=CARTESIAN_POINT('Ctrl Pts',(18.1843885347784,12.8237912132616,0.));
#56353=CARTESIAN_POINT('Ctrl Pts',(17.0210036637821,13.7799946040807,0.));
#56354=CARTESIAN_POINT('Ctrl Pts',(17.0210036637821,13.7799946040807,13.7799946040807));
#56355=CARTESIAN_POINT('Ctrl Pts',(17.0210036637821,0.,13.7799946040807));
#56356=CARTESIAN_POINT('Ctrl Pts',(17.0210036637821,-13.7799946040807,13.7799946040807));
#56357=CARTESIAN_POINT('Ctrl Pts',(17.0210036637821,-13.7799946040807,0.));
#56358=CARTESIAN_POINT('Ctrl Pts',(17.0210036637821,-13.7799946040807,-13.7799946040807));
#56359=CARTESIAN_POINT('Ctrl Pts',(17.0210036637821,0.,-13.7799946040807));
#56360=CARTESIAN_POINT('Ctrl Pts',(17.0210036637821,13.7799946040807,-13.7799946040807));
#56361=CARTESIAN_POINT('Ctrl Pts',(17.0210036637821,13.7799946040807,0.));
#56362=CARTESIAN_POINT('Ctrl Pts',(15.8649034353727,14.8662985491428,0.));
#56363=CARTESIAN_POINT('Ctrl Pts',(15.8649034353727,14.8662985491428,14.8662985491428));
#56364=CARTESIAN_POINT('Ctrl Pts',(15.8649034353727,0.,14.8662985491428));
#56365=CARTESIAN_POINT('Ctrl Pts',(15.8649034353727,-14.8662985491428,14.8662985491428));
#56366=CARTESIAN_POINT('Ctrl Pts',(15.8649034353727,-14.8662985491428,0.));
#56367=CARTESIAN_POINT('Ctrl Pts',(15.8649034353727,-14.8662985491428,-14.8662985491428));
#56368=CARTESIAN_POINT('Ctrl Pts',(15.8649034353727,0.,-14.8662985491428));
#56369=CARTESIAN_POINT('Ctrl Pts',(15.8649034353727,14.8662985491428,-14.8662985491428));
#56370=CARTESIAN_POINT('Ctrl Pts',(15.8649034353727,14.8662985491428,0.));
#56371=CARTESIAN_POINT('Ctrl Pts',(14.7267277676362,16.0674034956045,0.));
#56372=CARTESIAN_POINT('Ctrl Pts',(14.7267277676362,16.0674034956045,16.0674034956045));
#56373=CARTESIAN_POINT('Ctrl Pts',(14.7267277676362,0.,16.0674034956045));
#56374=CARTESIAN_POINT('Ctrl Pts',(14.7267277676362,-16.0674034956045,16.0674034956045));
#56375=CARTESIAN_POINT('Ctrl Pts',(14.7267277676362,-16.0674034956045,0.));
#56376=CARTESIAN_POINT('Ctrl Pts',(14.7267277676362,-16.0674034956045,-16.0674034956045));
#56377=CARTESIAN_POINT('Ctrl Pts',(14.7267277676362,0.,-16.0674034956045));
#56378=CARTESIAN_POINT('Ctrl Pts',(14.7267277676362,16.0674034956045,-16.0674034956045));
#56379=CARTESIAN_POINT('Ctrl Pts',(14.7267277676362,16.0674034956045,0.));
#56380=CARTESIAN_POINT('Ctrl Pts',(13.6172459538847,17.362757468191,0.));
#56381=CARTESIAN_POINT('Ctrl Pts',(13.6172459538847,17.362757468191,17.362757468191));
#56382=CARTESIAN_POINT('Ctrl Pts',(13.6172459538847,0.,17.362757468191));
#56383=CARTESIAN_POINT('Ctrl Pts',(13.6172459538847,-17.362757468191,17.362757468191));
#56384=CARTESIAN_POINT('Ctrl Pts',(13.6172459538847,-17.362757468191,0.));
#56385=CARTESIAN_POINT('Ctrl Pts',(13.6172459538847,-17.362757468191,-17.362757468191));
#56386=CARTESIAN_POINT('Ctrl Pts',(13.6172459538847,0.,-17.362757468191));
#56387=CARTESIAN_POINT('Ctrl Pts',(13.6172459538847,17.362757468191,-17.362757468191));
#56388=CARTESIAN_POINT('Ctrl Pts',(13.6172459538847,17.362757468191,0.));
#56389=CARTESIAN_POINT('Ctrl Pts',(12.5462580187496,18.7300247619529,0.));
#56390=CARTESIAN_POINT('Ctrl Pts',(12.5462580187496,18.7300247619529,18.7300247619529));
#56391=CARTESIAN_POINT('Ctrl Pts',(12.5462580187496,0.,18.7300247619529));
#56392=CARTESIAN_POINT('Ctrl Pts',(12.5462580187496,-18.7300247619529,18.7300247619529));
#56393=CARTESIAN_POINT('Ctrl Pts',(12.5462580187496,-18.7300247619529,0.));
#56394=CARTESIAN_POINT('Ctrl Pts',(12.5462580187496,-18.7300247619529,-18.7300247619529));
#56395=CARTESIAN_POINT('Ctrl Pts',(12.5462580187496,0.,-18.7300247619529));
#56396=CARTESIAN_POINT('Ctrl Pts',(12.5462580187496,18.7300247619529,-18.7300247619529));
#56397=CARTESIAN_POINT('Ctrl Pts',(12.5462580187496,18.7300247619529,0.));
#56398=CARTESIAN_POINT('Ctrl Pts',(11.5215838208076,20.1483844597128,0.));
#56399=CARTESIAN_POINT('Ctrl Pts',(11.5215838208076,20.1483844597128,20.1483844597128));
#56400=CARTESIAN_POINT('Ctrl Pts',(11.5215838208076,0.,20.1483844597128));
#56401=CARTESIAN_POINT('Ctrl Pts',(11.5215838208076,-20.1483844597128,20.1483844597128));
#56402=CARTESIAN_POINT('Ctrl Pts',(11.5215838208076,-20.1483844597128,0.));
#56403=CARTESIAN_POINT('Ctrl Pts',(11.5215838208076,-20.1483844597128,-20.1483844597128));
#56404=CARTESIAN_POINT('Ctrl Pts',(11.5215838208076,0.,-20.1483844597128));
#56405=CARTESIAN_POINT('Ctrl Pts',(11.5215838208076,20.1483844597128,-20.1483844597128));
#56406=CARTESIAN_POINT('Ctrl Pts',(11.5215838208076,20.1483844597128,0.));
#56407=CARTESIAN_POINT('Ctrl Pts',(10.5477031262524,21.602527086122,0.));
#56408=CARTESIAN_POINT('Ctrl Pts',(10.5477031262524,21.602527086122,21.602527086122));
#56409=CARTESIAN_POINT('Ctrl Pts',(10.5477031262524,0.,21.602527086122));
#56410=CARTESIAN_POINT('Ctrl Pts',(10.5477031262524,-21.602527086122,21.602527086122));
#56411=CARTESIAN_POINT('Ctrl Pts',(10.5477031262524,-21.602527086122,0.));
#56412=CARTESIAN_POINT('Ctrl Pts',(10.5477031262524,-21.602527086122,-21.602527086122));
#56413=CARTESIAN_POINT('Ctrl Pts',(10.5477031262524,0.,-21.602527086122));
#56414=CARTESIAN_POINT('Ctrl Pts',(10.5477031262524,21.602527086122,-21.602527086122));
#56415=CARTESIAN_POINT('Ctrl Pts',(10.5477031262524,21.602527086122,0.));
#56416=CARTESIAN_POINT('Ctrl Pts',(9.62553662153839,23.0838998256659,0.));
#56417=CARTESIAN_POINT('Ctrl Pts',(9.62553662153839,23.0838998256659,23.0838998256659));
#56418=CARTESIAN_POINT('Ctrl Pts',(9.62553662153839,0.,23.0838998256659));
#56419=CARTESIAN_POINT('Ctrl Pts',(9.62553662153839,-23.0838998256659,23.0838998256659));
#56420=CARTESIAN_POINT('Ctrl Pts',(9.62553662153839,-23.0838998256659,0.));
#56421=CARTESIAN_POINT('Ctrl Pts',(9.62553662153839,-23.0838998256659,-23.0838998256659));
#56422=CARTESIAN_POINT('Ctrl Pts',(9.62553662153839,0.,-23.0838998256659));
#56423=CARTESIAN_POINT('Ctrl Pts',(9.62553662153839,23.0838998256659,-23.0838998256659));
#56424=CARTESIAN_POINT('Ctrl Pts',(9.62553662153839,23.0838998256659,0.));
#56425=CARTESIAN_POINT('Ctrl Pts',(8.75359166551105,24.5886478127263,0.));
#56426=CARTESIAN_POINT('Ctrl Pts',(8.75359166551105,24.5886478127262,24.5886478127262));
#56427=CARTESIAN_POINT('Ctrl Pts',(8.75359166551105,0.,24.5886478127263));
#56428=CARTESIAN_POINT('Ctrl Pts',(8.75359166551105,-24.5886478127262,24.5886478127262));
#56429=CARTESIAN_POINT('Ctrl Pts',(8.75359166551105,-24.5886478127263,0.));
#56430=CARTESIAN_POINT('Ctrl Pts',(8.75359166551105,-24.5886478127262,-24.5886478127262));
#56431=CARTESIAN_POINT('Ctrl Pts',(8.75359166551105,0.,-24.5886478127263));
#56432=CARTESIAN_POINT('Ctrl Pts',(8.75359166551105,24.5886478127262,-24.5886478127262));
#56433=CARTESIAN_POINT('Ctrl Pts',(8.75359166551105,24.5886478127263,0.));
#56434=CARTESIAN_POINT('Ctrl Pts',(7.92870053877921,26.1164647205758,0.));
#56435=CARTESIAN_POINT('Ctrl Pts',(7.92870053877921,26.1164647205758,26.1164647205758));
#56436=CARTESIAN_POINT('Ctrl Pts',(7.92870053877921,0.,26.1164647205758));
#56437=CARTESIAN_POINT('Ctrl Pts',(7.92870053877921,-26.1164647205758,26.1164647205758));
#56438=CARTESIAN_POINT('Ctrl Pts',(7.92870053877921,-26.1164647205758,0.));
#56439=CARTESIAN_POINT('Ctrl Pts',(7.92870053877921,-26.1164647205758,-26.1164647205758));
#56440=CARTESIAN_POINT('Ctrl Pts',(7.92870053877921,0.,-26.1164647205758));
#56441=CARTESIAN_POINT('Ctrl Pts',(7.92870053877921,26.1164647205758,-26.1164647205758));
#56442=CARTESIAN_POINT('Ctrl Pts',(7.92870053877921,26.1164647205758,0.));
#56443=CARTESIAN_POINT('Ctrl Pts',(7.14689760675259,27.6690738550248,0.));
#56444=CARTESIAN_POINT('Ctrl Pts',(7.14689760675259,27.6690738550248,27.6690738550248));
#56445=CARTESIAN_POINT('Ctrl Pts',(7.1468976067526,0.,27.6690738550248));
#56446=CARTESIAN_POINT('Ctrl Pts',(7.1468976067526,-27.6690738550248,27.6690738550248));
#56447=CARTESIAN_POINT('Ctrl Pts',(7.1468976067526,-27.6690738550248,0.));
#56448=CARTESIAN_POINT('Ctrl Pts',(7.1468976067526,-27.6690738550248,-27.6690738550248));
#56449=CARTESIAN_POINT('Ctrl Pts',(7.1468976067526,0.,-27.6690738550248));
#56450=CARTESIAN_POINT('Ctrl Pts',(7.14689760675259,27.6690738550248,-27.6690738550248));
#56451=CARTESIAN_POINT('Ctrl Pts',(7.14689760675259,27.6690738550248,0.));
#56452=CARTESIAN_POINT('Ctrl Pts',(6.40416480933221,29.248955946805,0.));
#56453=CARTESIAN_POINT('Ctrl Pts',(6.40416480933221,29.248955946805,29.248955946805));
#56454=CARTESIAN_POINT('Ctrl Pts',(6.40416480933221,0.,29.248955946805));
#56455=CARTESIAN_POINT('Ctrl Pts',(6.40416480933221,-29.248955946805,29.248955946805));
#56456=CARTESIAN_POINT('Ctrl Pts',(6.40416480933221,-29.248955946805,0.));
#56457=CARTESIAN_POINT('Ctrl Pts',(6.40416480933221,-29.248955946805,-29.248955946805));
#56458=CARTESIAN_POINT('Ctrl Pts',(6.40416480933221,0.,-29.248955946805));
#56459=CARTESIAN_POINT('Ctrl Pts',(6.40416480933221,29.248955946805,-29.248955946805));
#56460=CARTESIAN_POINT('Ctrl Pts',(6.40416480933221,29.248955946805,0.));
#56461=CARTESIAN_POINT('Ctrl Pts',(5.69731071687183,30.8577859595634,0.));
#56462=CARTESIAN_POINT('Ctrl Pts',(5.69731071687183,30.8577859595634,30.8577859595634));
#56463=CARTESIAN_POINT('Ctrl Pts',(5.69731071687183,0.,30.8577859595634));
#56464=CARTESIAN_POINT('Ctrl Pts',(5.69731071687183,-30.8577859595634,30.8577859595634));
#56465=CARTESIAN_POINT('Ctrl Pts',(5.69731071687183,-30.8577859595634,0.));
#56466=CARTESIAN_POINT('Ctrl Pts',(5.69731071687183,-30.8577859595634,-30.8577859595634));
#56467=CARTESIAN_POINT('Ctrl Pts',(5.69731071687183,0.,-30.8577859595634));
#56468=CARTESIAN_POINT('Ctrl Pts',(5.69731071687183,30.8577859595634,-30.8577859595634));
#56469=CARTESIAN_POINT('Ctrl Pts',(5.69731071687183,30.8577859595634,0.));
#56470=CARTESIAN_POINT('Ctrl Pts',(5.02401496259691,32.4964011792533,0.));
#56471=CARTESIAN_POINT('Ctrl Pts',(5.02401496259691,32.4964011792533,32.4964011792533));
#56472=CARTESIAN_POINT('Ctrl Pts',(5.02401496259691,0.,32.4964011792533));
#56473=CARTESIAN_POINT('Ctrl Pts',(5.02401496259691,-32.4964011792533,32.4964011792533));
#56474=CARTESIAN_POINT('Ctrl Pts',(5.02401496259691,-32.4964011792533,0.));
#56475=CARTESIAN_POINT('Ctrl Pts',(5.02401496259691,-32.4964011792533,-32.4964011792533));
#56476=CARTESIAN_POINT('Ctrl Pts',(5.02401496259691,0.,-32.4964011792533));
#56477=CARTESIAN_POINT('Ctrl Pts',(5.02401496259691,32.4964011792533,-32.4964011792533));
#56478=CARTESIAN_POINT('Ctrl Pts',(5.02401496259691,32.4964011792533,0.));
#56479=CARTESIAN_POINT('Ctrl Pts',(4.38267277981043,34.1651137045816,0.));
#56480=CARTESIAN_POINT('Ctrl Pts',(4.38267277981043,34.1651137045815,34.1651137045815));
#56481=CARTESIAN_POINT('Ctrl Pts',(4.38267277981043,0.,34.1651137045816));
#56482=CARTESIAN_POINT('Ctrl Pts',(4.38267277981043,-34.1651137045815,34.1651137045815));
#56483=CARTESIAN_POINT('Ctrl Pts',(4.38267277981043,-34.1651137045816,0.));
#56484=CARTESIAN_POINT('Ctrl Pts',(4.38267277981043,-34.1651137045815,-34.1651137045815));
#56485=CARTESIAN_POINT('Ctrl Pts',(4.38267277981043,0.,-34.1651137045816));
#56486=CARTESIAN_POINT('Ctrl Pts',(4.38267277981043,34.1651137045815,-34.1651137045815));
#56487=CARTESIAN_POINT('Ctrl Pts',(4.38267277981043,34.1651137045816,0.));
#56488=CARTESIAN_POINT('Ctrl Pts',(3.89437496746067,35.5241326822989,0.));
#56489=CARTESIAN_POINT('Ctrl Pts',(3.89437496746067,35.5241326822989,35.5241326822989));
#56490=CARTESIAN_POINT('Ctrl Pts',(3.89437496746067,0.,35.5241326822989));
#56491=CARTESIAN_POINT('Ctrl Pts',(3.89437496746066,-35.5241326822989,35.5241326822989));
#56492=CARTESIAN_POINT('Ctrl Pts',(3.89437496746066,-35.5241326822989,0.));
#56493=CARTESIAN_POINT('Ctrl Pts',(3.89437496746066,-35.5241326822989,-35.5241326822989));
#56494=CARTESIAN_POINT('Ctrl Pts',(3.89437496746067,0.,-35.5241326822989));
#56495=CARTESIAN_POINT('Ctrl Pts',(3.89437496746067,35.5241326822989,-35.5241326822989));
#56496=CARTESIAN_POINT('Ctrl Pts',(3.89437496746067,35.5241326822989,0.));
#56497=CARTESIAN_POINT('Ctrl Pts',(3.5418673953418,36.5568488026925,0.));
#56498=CARTESIAN_POINT('Ctrl Pts',(3.5418673953418,36.5568488026925,36.5568488026925));
#56499=CARTESIAN_POINT('Ctrl Pts',(3.5418673953418,0.,36.5568488026925));
#56500=CARTESIAN_POINT('Ctrl Pts',(3.5418673953418,-36.5568488026925,36.5568488026925));
#56501=CARTESIAN_POINT('Ctrl Pts',(3.5418673953418,-36.5568488026925,0.));
#56502=CARTESIAN_POINT('Ctrl Pts',(3.5418673953418,-36.5568488026925,-36.5568488026925));
#56503=CARTESIAN_POINT('Ctrl Pts',(3.5418673953418,0.,-36.5568488026925));
#56504=CARTESIAN_POINT('Ctrl Pts',(3.5418673953418,36.5568488026925,-36.5568488026925));
#56505=CARTESIAN_POINT('Ctrl Pts',(3.5418673953418,36.5568488026925,0.));
#56506=CARTESIAN_POINT('Ctrl Pts',(3.31294245015623,37.2512891119684,0.));
#56507=CARTESIAN_POINT('Ctrl Pts',(3.31294245015623,37.2512891119684,37.2512891119684));
#56508=CARTESIAN_POINT('Ctrl Pts',(3.31294245015623,0.,37.2512891119684));
#56509=CARTESIAN_POINT('Ctrl Pts',(3.31294245015623,-37.2512891119684,37.2512891119684));
#56510=CARTESIAN_POINT('Ctrl Pts',(3.31294245015623,-37.2512891119684,0.));
#56511=CARTESIAN_POINT('Ctrl Pts',(3.31294245015623,-37.2512891119684,-37.2512891119684));
#56512=CARTESIAN_POINT('Ctrl Pts',(3.31294245015623,0.,-37.2512891119684));
#56513=CARTESIAN_POINT('Ctrl Pts',(3.31294245015623,37.2512891119684,-37.2512891119684));
#56514=CARTESIAN_POINT('Ctrl Pts',(3.31294245015623,37.2512891119684,0.));
#56515=CARTESIAN_POINT('Ctrl Pts',(3.2,37.6,0.));
#56516=CARTESIAN_POINT('Ctrl Pts',(3.2,37.6,37.6));
#56517=CARTESIAN_POINT('Ctrl Pts',(3.2,0.,37.6));
#56518=CARTESIAN_POINT('Ctrl Pts',(3.2,-37.6,37.6));
#56519=CARTESIAN_POINT('Ctrl Pts',(3.2,-37.6,0.));
#56520=CARTESIAN_POINT('Ctrl Pts',(3.2,-37.6,-37.6));
#56521=CARTESIAN_POINT('Ctrl Pts',(3.2,0.,-37.6));
#56522=CARTESIAN_POINT('Ctrl Pts',(3.2,37.6,-37.6));
#56523=CARTESIAN_POINT('Ctrl Pts',(3.2,37.6,0.));
#56524=CARTESIAN_POINT('',(27.,9.2,0.));
#56525=CARTESIAN_POINT('Ctrl Pts',(24.5,9.71413754081038,0.));
#56526=CARTESIAN_POINT('Ctrl Pts',(24.584270852469,9.69059102176396,0.));
#56527=CARTESIAN_POINT('Ctrl Pts',(24.8823684230922,9.60913381736612,0.));
#56528=CARTESIAN_POINT('Ctrl Pts',(25.3906552690265,9.48132788945834,0.));
#56529=CARTESIAN_POINT('Ctrl Pts',(25.892339495915,9.37377670323605,0.));
#56530=CARTESIAN_POINT('Ctrl Pts',(26.3874085880356,9.28597940593777,0.));
#56531=CARTESIAN_POINT('Ctrl Pts',(26.796570998452,9.22636560737002,0.));
#56532=CARTESIAN_POINT('Ctrl Pts',(27.,9.2,0.));
#56533=CARTESIAN_POINT('',(27.,-9.2,-1.12667505521557E-15));
#56534=CARTESIAN_POINT('Origin',(27.,0.,0.));
#56535=CARTESIAN_POINT('Origin',(27.,0.,0.));
#56536=CARTESIAN_POINT('',(3.2,37.5892271801377,-0.899999999999994));
#56537=CARTESIAN_POINT('Origin',(3.2,0.,0.));
#56538=CARTESIAN_POINT('',(24.5,5.24229587453786,-8.17819063886291));
#56539=CARTESIAN_POINT('Ctrl Pts',(3.2,37.5892271801377,-0.9));
#56540=CARTESIAN_POINT('Ctrl Pts',(3.45174020122667,36.8117541621245,-0.9));
#56541=CARTESIAN_POINT('Ctrl Pts',(3.71840125351367,36.0251069070192,-0.899999999999995));
#56542=CARTESIAN_POINT('Ctrl Pts',(4.,35.2340925362767,-0.899999999999995));
#56543=CARTESIAN_POINT('Ctrl Pts',(4.62816481945855,33.4695697690894,-0.900000000000002));
#56544=CARTESIAN_POINT('Ctrl Pts',(5.32582968819375,31.7073778438848,-0.839717528293596));
#56545=CARTESIAN_POINT('Ctrl Pts',(6.03866110767478,30.0825526385231,-0.844879409428011));
#56546=CARTESIAN_POINT('Ctrl Pts',(6.32798219793006,29.4230752543307,-0.846974492552523));
#56547=CARTESIAN_POINT('Ctrl Pts',(6.61604117565574,28.793782414028,-0.861009606870751));
#56548=CARTESIAN_POINT('Ctrl Pts',(6.89476148100328,28.2061545880624,-0.893825964111232));
#56549=CARTESIAN_POINT('Ctrl Pts',(7.65522892458988,26.6028561486637,-0.983362932963847));
#56550=CARTESIAN_POINT('Ctrl Pts',(8.35226708789681,25.307434370521,-1.09931216348024));
#56551=CARTESIAN_POINT('Ctrl Pts',(8.78926323543883,24.5226424560649,-1.19512255048227));
#56552=CARTESIAN_POINT('Ctrl Pts',(8.9903195843563,24.1615697146506,-1.23920368645418));
#56553=CARTESIAN_POINT('Ctrl Pts',(9.18275522864328,23.8242551291094,-1.28645191173913));
#56554=CARTESIAN_POINT('Ctrl Pts',(9.37496047156673,23.4940308964114,-1.34002181064069));
#56555=CARTESIAN_POINT('Ctrl Pts',(9.48075234026397,23.312271865623,-1.36950726912516));
#56556=CARTESIAN_POINT('Ctrl Pts',(9.58626091274252,23.1330836509346,-1.40088640835537));
#56557=CARTESIAN_POINT('Ctrl Pts',(9.69257910363365,22.9544806736799,-1.43495784272423));
#56558=CARTESIAN_POINT('Ctrl Pts',(10.0319880480858,22.3843106258459,-1.54372708981334));
#56559=CARTESIAN_POINT('Ctrl Pts',(10.3788056757338,21.8199482988106,-1.68100872063375));
#56560=CARTESIAN_POINT('Ctrl Pts',(10.7756849097841,21.1980699537259,-1.85708105784221));
#56561=CARTESIAN_POINT('Ctrl Pts',(10.8890930417026,21.0203683877436,-1.90739367974876));
#56562=CARTESIAN_POINT('Ctrl Pts',(11.0576203534459,20.7579535709124,-1.98378827882632));
#56563=CARTESIAN_POINT('Ctrl Pts',(11.2725125504481,20.4310649639431,-2.08497651593983));
#56564=CARTESIAN_POINT('Ctrl Pts',(11.5968279601822,19.9377245170328,-2.23768985331333));
#56565=CARTESIAN_POINT('Ctrl Pts',(12.025567884829,19.2993337801102,-2.44965947375353));
#56566=CARTESIAN_POINT('Ctrl Pts',(12.532035905153,18.5840189796223,-2.68594697261969));
#56567=CARTESIAN_POINT('Ctrl Pts',(13.0988763174395,17.7834366720487,-2.95040059634461));
#56568=CARTESIAN_POINT('Ctrl Pts',(13.7495416909273,16.8976545731049,-3.30146477931067));
#56569=CARTESIAN_POINT('Ctrl Pts',(14.4398764933743,16.0059407465834,-3.67134635070127));
#56570=CARTESIAN_POINT('Ctrl Pts',(14.7901814029647,15.553447651533,-3.85903981475072));
#56571=CARTESIAN_POINT('Ctrl Pts',(15.1459546146389,15.1068649503278,-4.0457097304312));
#56572=CARTESIAN_POINT('Ctrl Pts',(15.4570717747561,14.7276262420568,-4.19832359076494));
#56573=CARTESIAN_POINT('Ctrl Pts',(15.7998231422506,14.3098267680006,-4.36645513744121));
#56574=CARTESIAN_POINT('Ctrl Pts',(16.0676294526253,13.990318693849,-4.50331995895759));
#56575=CARTESIAN_POINT('Ctrl Pts',(16.3615308021931,13.6447281514167,-4.65432808429673));
#56576=CARTESIAN_POINT('Ctrl Pts',(17.0296616056386,12.859091450129,-4.99761735553682));
#56577=CARTESIAN_POINT('Ctrl Pts',(17.7084691891668,12.0886798104406,-5.35674638147456));
#56578=CARTESIAN_POINT('Ctrl Pts',(18.4207032016838,11.3350011751768,-5.68212942088499));
#56579=CARTESIAN_POINT('Ctrl Pts',(18.8298642043985,10.902031251374,-5.86905401074141));
#56580=CARTESIAN_POINT('Ctrl Pts',(19.2113759274554,10.5047768811947,-6.04970003189267));
#56581=CARTESIAN_POINT('Ctrl Pts',(19.5701113609878,10.1352032844547,-6.21809496346388));
#56582=CARTESIAN_POINT('Ctrl Pts',(20.1215476022469,9.56710697724541,-6.47694608167746));
#56583=CARTESIAN_POINT('Ctrl Pts',(20.6514912601264,9.02382054581082,-6.73117610025783));
#56584=CARTESIAN_POINT('Ctrl Pts',(21.3979544325339,8.30110396122067,-7.03003130093698));
#56585=CARTESIAN_POINT('Ctrl Pts',(21.8107631281408,7.90142759190171,-7.19530405668434));
#56586=CARTESIAN_POINT('Ctrl Pts',(22.3076315954255,7.42611128017324,-7.38765428460632));
#56587=CARTESIAN_POINT('Ctrl Pts',(22.8472772293734,6.90153052972702,-7.58806809630901));
#56588=CARTESIAN_POINT('Ctrl Pts',(23.3953136567666,6.36879322533974,-7.79159808424252));
#56589=CARTESIAN_POINT('Ctrl Pts',(23.9608264582666,5.8087958334843,-7.99400612701712));
#56590=CARTESIAN_POINT('Ctrl Pts',(24.5,5.24229587453786,-8.17819063886291));
#56591=CARTESIAN_POINT('',(24.5,7.16983932323689,-6.55422552562448));
#56592=CARTESIAN_POINT('Ctrl Pts',(24.5,5.24229587453786,-8.17819063886291));
#56593=CARTESIAN_POINT('Ctrl Pts',(24.5,5.64521806942229,-7.91991378359311));
#56594=CARTESIAN_POINT('Ctrl Pts',(24.5,6.02903768297008,-7.63187011183746));
#56595=CARTESIAN_POINT('Ctrl Pts',(24.5,6.66464379880506,-7.07668969209044));
#56596=CARTESIAN_POINT('Ctrl Pts',(24.5,6.92481388700865,-6.82226528119806));
#56597=CARTESIAN_POINT('Ctrl Pts',(24.5,7.16983932323689,-6.55422552562448));
#56598=CARTESIAN_POINT('Ctrl Pts',(24.5,7.16983932323689,-6.55422552562448));
#56599=CARTESIAN_POINT('Ctrl Pts',(23.8274939345993,7.72087585355875,-6.22993425436329));
#56600=CARTESIAN_POINT('Ctrl Pts',(23.3366347314239,8.10243836675503,-5.9971074697364));
#56601=CARTESIAN_POINT('Ctrl Pts',(22.5855494187791,8.69228987173019,-5.63439342300611));
#56602=CARTESIAN_POINT('Ctrl Pts',(22.2454144275548,8.95940884355763,-5.4701354658546));
#56603=CARTESIAN_POINT('Ctrl Pts',(21.8382660751901,9.285050095425,-5.26284147008233));
#56604=CARTESIAN_POINT('Ctrl Pts',(21.3802156960109,9.65774830624375,-5.02425880299215));
#56605=CARTESIAN_POINT('Ctrl Pts',(20.7694693299338,10.1546894468861,-4.70614205523307));
#56606=CARTESIAN_POINT('Ctrl Pts',(20.1629003036551,10.6565278673439,-4.38627069785178));
#56607=CARTESIAN_POINT('Ctrl Pts',(19.5574857571565,11.1735047521273,-4.09023617084508));
#56608=CARTESIAN_POINT('Ctrl Pts',(18.6418529423121,11.9553838843044,-3.64251166732608));
#56609=CARTESIAN_POINT('Ctrl Pts',(17.773481333357,12.7723018260926,-3.16504296577866));
#56610=CARTESIAN_POINT('Ctrl Pts',(16.9621253129276,13.5883953552262,-2.76110771822243));
#56611=CARTESIAN_POINT('Ctrl Pts',(16.8133360681893,13.7380533805297,-2.68703268963603));
#56612=CARTESIAN_POINT('Ctrl Pts',(16.6656205375718,13.8886489787092,-2.61462956901353));
#56613=CARTESIAN_POINT('Ctrl Pts',(16.5183901926363,14.0408164096359,-2.54382268324666));
#56614=CARTESIAN_POINT('Ctrl Pts',(15.7264522885453,14.8593104257425,-2.16295923601354));
#56615=CARTESIAN_POINT('Ctrl Pts',(14.9462259716364,15.7452570124731,-1.74040949812692));
#56616=CARTESIAN_POINT('Ctrl Pts',(14.2963150411565,16.5251374105151,-1.42162688464704));
#56617=CARTESIAN_POINT('Ctrl Pts',(13.9908350931921,16.8917073699346,-1.27178835814949));
#56618=CARTESIAN_POINT('Ctrl Pts',(13.7077063565862,17.2419142372062,-1.13921261589477));
#56619=CARTESIAN_POINT('Ctrl Pts',(13.4460198946299,17.5732908880439,-1.02322593212869));
#56620=CARTESIAN_POINT('Ctrl Pts',(12.8297897879206,18.3536303346477,-0.750095690771559));
#56621=CARTESIAN_POINT('Ctrl Pts',(12.341051952675,19.0193845631393,-0.520653486972896));
#56622=CARTESIAN_POINT('Ctrl Pts',(11.9631039144853,19.5480150790474,-0.35462224598778));
#56623=CARTESIAN_POINT('Ctrl Pts',(11.6627866324515,19.9680645665328,-0.222693922548958));
#56624=CARTESIAN_POINT('Ctrl Pts',(11.3909151560383,20.3600418064951,-0.108420555322461));
#56625=CARTESIAN_POINT('Ctrl Pts',(11.1111871729018,20.775057671175,1.50053580671994E-15));
#56626=CARTESIAN_POINT('Ctrl Pts',(2.09999999999999,9.70239382419368,0.9));
#56627=CARTESIAN_POINT('Ctrl Pts',(2.73333333333333,9.70239382419368,0.9));
#56628=CARTESIAN_POINT('Ctrl Pts',(3.36632387111522,9.70238311374191,0.899943572704684));
#56629=CARTESIAN_POINT('Ctrl Pts',(4.12418390810446,9.70237979485746,0.899926556305573));
#56630=CARTESIAN_POINT('Ctrl Pts',(4.36793405804848,9.70227889326302,0.901142755072256));
#56631=CARTESIAN_POINT('Ctrl Pts',(4.86516733785842,9.70182686384601,0.906703885275862));
#56632=CARTESIAN_POINT('Ctrl Pts',(5.74558933798915,9.70077369524553,0.919837119111666));
#56633=CARTESIAN_POINT('Ctrl Pts',(6.51837592843883,9.70075915441346,0.920043366739036));
#56634=CARTESIAN_POINT('Ctrl Pts',(7.1031128831408,9.70255678431008,0.896330940156011));
#56635=CARTESIAN_POINT('Ctrl Pts',(7.23026824315571,9.70301993681095,0.891007254471877));
#56636=CARTESIAN_POINT('Ctrl Pts',(7.42494888780729,9.70386111674548,0.882248192098819));
#56637=CARTESIAN_POINT('Ctrl Pts',(7.61951912013724,9.70483286951889,0.872784906947758));
#56638=CARTESIAN_POINT('Ctrl Pts',(8.01076648546345,9.70700730924683,0.852173583936991));
#56639=CARTESIAN_POINT('Ctrl Pts',(8.6008368585707,9.7109991524828,0.814319361374828));
#56640=CARTESIAN_POINT('Ctrl Pts',(9.25154787508086,9.71589427768064,0.755208645277658));
#56641=CARTESIAN_POINT('Ctrl Pts',(9.76267229657535,9.71954704831515,0.694519587021701));
#56642=CARTESIAN_POINT('Ctrl Pts',(10.014171082006,9.72118810845726,0.65910761044294));
#56643=CARTESIAN_POINT('Ctrl Pts',(10.7177517881878,9.72539449907129,0.550905934553037));
#56644=CARTESIAN_POINT('Ctrl Pts',(11.8208631668899,9.7387414708566,0.30695723782105));
#56645=CARTESIAN_POINT('Ctrl Pts',(12.8080214119101,9.74360244998835,0.00601043568995343));
#56646=CARTESIAN_POINT('Ctrl Pts',(13.5604126906717,9.73617681748438,-0.231382581987876));
#56647=CARTESIAN_POINT('Ctrl Pts',(14.1415324087999,9.72798482552665,-0.434588673886165));
#56648=CARTESIAN_POINT('Ctrl Pts',(15.2007205223741,9.70191685856208,-0.866738392578812));
#56649=CARTESIAN_POINT('Ctrl Pts',(15.9284934234743,9.66540770021948,-1.21113245671502));
#56650=CARTESIAN_POINT('Ctrl Pts',(16.6747552776732,9.60865895503553,-1.56555224791166));
#56651=CARTESIAN_POINT('Ctrl Pts',(17.2497622997617,9.55601631928308,-1.85742036071714));
#56652=CARTESIAN_POINT('Ctrl Pts',(18.2984408124205,9.42723341754466,-2.44688146345142));
#56653=CARTESIAN_POINT('Ctrl Pts',(19.023654255104,9.29844614565911,-2.89446970327295));
#56654=CARTESIAN_POINT('Ctrl Pts',(19.7681836146925,9.13779726718118,-3.34781162099393));
#56655=CARTESIAN_POINT('Ctrl Pts',(20.3331355916067,8.99879342938229,-3.70764381764044));
#56656=CARTESIAN_POINT('Ctrl Pts',(21.3722795878879,8.68312647686188,-4.41282175870863));
#56657=CARTESIAN_POINT('Ctrl Pts',(22.0962322041254,8.39994687509579,-4.92488812724573));
#56658=CARTESIAN_POINT('Ctrl Pts',(23.2302270680055,7.90257741264269,-5.69145757370445));
#56659=CARTESIAN_POINT('Ctrl Pts',(23.8854423668127,7.55670872152269,-6.13564425905366));
#56660=CARTESIAN_POINT('Ctrl Pts',(24.5000000001022,7.16983932310749,-6.55422552562591));
#56661=CARTESIAN_POINT('Ctrl Pts',(2.09999999999999,13.886302003518,0.9));
#56662=CARTESIAN_POINT('Ctrl Pts',(2.73333333333333,13.886302003518,0.9));
#56663=CARTESIAN_POINT('Ctrl Pts',(3.36613013456572,13.886293466186,0.899934636656705));
#56664=CARTESIAN_POINT('Ctrl Pts',(4.12377198935332,13.8862908337435,0.899915275189073));
#56665=CARTESIAN_POINT('Ctrl Pts',(4.36466956133672,13.8861969875265,0.901644022806547));
#56666=CARTESIAN_POINT('Ctrl Pts',(4.86001353404206,13.8857766744056,0.909581065394921));
#56667=CARTESIAN_POINT('Ctrl Pts',(5.74114344094781,13.8847964321218,0.928387766932829));
#56668=CARTESIAN_POINT('Ctrl Pts',(6.52371165318003,13.8847857317307,0.928826747414305));
#56669=CARTESIAN_POINT('Ctrl Pts',(7.12008868672732,13.8864582425445,0.894425264736249));
#56670=CARTESIAN_POINT('Ctrl Pts',(7.2473920845663,13.886908806475,0.886799179992507));
#56671=CARTESIAN_POINT('Ctrl Pts',(7.44367696450914,13.8877691576202,0.874193604263346));
#56672=CARTESIAN_POINT('Ctrl Pts',(7.63959093335125,13.8887879198323,0.860585277112663));
#56673=CARTESIAN_POINT('Ctrl Pts',(8.03420776743963,13.891091359666,0.830913205754772));
#56674=CARTESIAN_POINT('Ctrl Pts',(8.63054063110045,13.8953340247099,0.776366915874588));
#56675=CARTESIAN_POINT('Ctrl Pts',(9.29110414788195,13.9000524777747,0.690945060637293));
#56676=CARTESIAN_POINT('Ctrl Pts',(9.81209171470009,13.9029382846741,0.602989957084009));
#56677=CARTESIAN_POINT('Ctrl Pts',(10.0692653859326,13.9039233252519,0.551564607071378));
#56678=CARTESIAN_POINT('Ctrl Pts',(10.7901161263785,13.905801040616,0.394264167844574));
#56679=CARTESIAN_POINT('Ctrl Pts',(11.9164140743865,13.9153944782979,0.0402610058985021));
#56680=CARTESIAN_POINT('Ctrl Pts',(12.9133300122381,13.9101438826876,-0.392622143318933));
#56681=CARTESIAN_POINT('Ctrl Pts',(13.6697345269123,13.8898038073169,-0.732507745058096));
#56682=CARTESIAN_POINT('Ctrl Pts',(14.2631482815798,13.8697611392688,-1.0268202159191));
#56683=CARTESIAN_POINT('Ctrl Pts',(15.3329170876201,13.8143188664754,-1.64805789896314));
#56684=CARTESIAN_POINT('Ctrl Pts',(16.065400822286,13.7476864604472,-2.1401844399863));
#56685=CARTESIAN_POINT('Ctrl Pts',(16.8131024396104,13.6516057483624,-2.64427530685194));
#56686=CARTESIAN_POINT('Ctrl Pts',(17.3939205030447,13.5638317918362,-3.06247796039152));
#56687=CARTESIAN_POINT('Ctrl Pts',(18.4451570754854,13.3544577672646,-3.90129822129329));
#56688=CARTESIAN_POINT('Ctrl Pts',(19.1720430750714,13.1515971699246,-4.53544369462377));
#56689=CARTESIAN_POINT('Ctrl Pts',(19.9173987143267,12.902625551066,-5.17597857280555));
#56690=CARTESIAN_POINT('Ctrl Pts',(20.4826350906704,12.6889939496253,-5.68486006256131));
#56691=CARTESIAN_POINT('Ctrl Pts',(21.5194164976709,12.2087215604998,-6.67751869749508));
#56692=CARTESIAN_POINT('Ctrl Pts',(22.2433236988674,11.7831123238236,-7.39621420284916));
#56693=CARTESIAN_POINT('Ctrl Pts',(23.3780713364062,11.0396851260099,-8.46963766904746));
#56694=CARTESIAN_POINT('Ctrl Pts',(24.0312127056184,10.5284370227301,-9.08844396340443));
#56695=CARTESIAN_POINT('Ctrl Pts',(24.6419825553303,9.96056935923752,-9.66798043909671));
#56696=CARTESIAN_POINT('Ctrl Pts',(2.09999999999999,23.6487544219413,0.9));
#56697=CARTESIAN_POINT('Ctrl Pts',(2.73333333333333,23.6487544219413,0.9));
#56698=CARTESIAN_POINT('Ctrl Pts',(3.36565166989018,23.648723186002,0.899810674604605));
#56699=CARTESIAN_POINT('Ctrl Pts',(4.1227770961911,23.6487135356683,0.899754412481333));
#56700=CARTESIAN_POINT('Ctrl Pts',(4.35701428556174,23.6486339129901,0.902631341193944));
#56701=CARTESIAN_POINT('Ctrl Pts',(4.84795832867355,23.6482823455618,0.916015675715051));
#56702=CARTESIAN_POINT('Ctrl Pts',(5.73069615138054,23.6474648422221,0.948050758092538));
#56703=CARTESIAN_POINT('Ctrl Pts',(6.53614700405502,23.6474243933554,0.949253331942218));
#56704=CARTESIAN_POINT('Ctrl Pts',(7.15941198676745,23.6487878326115,0.888431899181333));
#56705=CARTESIAN_POINT('Ctrl Pts',(7.28705556652675,23.6492079046684,0.875410302124557));
#56706=CARTESIAN_POINT('Ctrl Pts',(7.48703947127753,23.6501100122595,0.853609697064992));
#56707=CARTESIAN_POINT('Ctrl Pts',(7.68604134768081,23.6512342606514,0.830120478181656));
#56708=CARTESIAN_POINT('Ctrl Pts',(8.08839242481482,23.6538318226179,0.778768089003677));
#56709=CARTESIAN_POINT('Ctrl Pts',(8.69896725403256,23.6586132337531,0.683967884128669));
#56710=CARTESIAN_POINT('Ctrl Pts',(9.38146799592133,23.6628388218879,0.534448529854445));
#56711=CARTESIAN_POINT('Ctrl Pts',(9.92347326694303,23.6638129580854,0.379381577922531));
#56712=CARTESIAN_POINT('Ctrl Pts',(10.1922138317613,23.663170473224,0.288268137281189));
#56713=CARTESIAN_POINT('Ctrl Pts',(10.9469984854868,23.6592100918921,0.00858085944299974));
#56714=CARTESIAN_POINT('Ctrl Pts',(12.1071835656316,23.6588244502173,-0.615249067553259));
#56715=CARTESIAN_POINT('Ctrl Pts',(13.10934181009,23.6284698279663,-1.35870373313894));
#56716=CARTESIAN_POINT('Ctrl Pts',(13.8683634030329,23.5768907059628,-1.93925931749388));
#56717=CARTESIAN_POINT('Ctrl Pts',(14.4658081522521,23.5282487607608,-2.44691660663979));
#56718=CARTESIAN_POINT('Ctrl Pts',(15.5292065922307,23.4040225569915,-3.50091787875384));
#56719=CARTESIAN_POINT('Ctrl Pts',(16.25612925985,23.2671320804502,-4.33240603899768));
#56720=CARTESIAN_POINT('Ctrl Pts',(17.0018288855248,23.0785614632775,-5.18472180987648));
#56721=CARTESIAN_POINT('Ctrl Pts',(17.5709926777516,22.9116014373373,-5.88434164318249));
#56722=CARTESIAN_POINT('Ctrl Pts',(18.6067980794747,22.520519768836,-7.28568570527198));
#56723=CARTESIAN_POINT('Ctrl Pts',(19.3243460106793,22.1491525108876,-8.34596662426811));
#56724=CARTESIAN_POINT('Ctrl Pts',(20.0666634439746,21.6959815979795,-9.42157847934581));
#56725=CARTESIAN_POINT('Ctrl Pts',(20.6167925376506,21.3177487953732,-10.2604211543252));
#56726=CARTESIAN_POINT('Ctrl Pts',(21.6393809830421,20.4677589075133,-11.9080648199959));
#56727=CARTESIAN_POINT('Ctrl Pts',(22.3554885642927,19.7185230095471,-13.1029251946305));
#56728=CARTESIAN_POINT('Ctrl Pts',(23.4867409067233,18.408630119116,-14.8934828716927));
#56729=CARTESIAN_POINT('Ctrl Pts',(24.1253373265787,17.5278847743971,-15.9063459622623));
#56730=CARTESIAN_POINT('Ctrl Pts',(24.7277571265287,16.5516187964772,-16.8576639625222));
#56731=CARTESIAN_POINT('Ctrl Pts',(2.09999999999999,33.4112068403646,0.9));
#56732=CARTESIAN_POINT('Ctrl Pts',(2.73333333333333,33.4112068403646,0.9));
#56733=CARTESIAN_POINT('Ctrl Pts',(3.36511452663434,33.4111761653147,0.899840745554594));
#56734=CARTESIAN_POINT('Ctrl Pts',(4.12170983818995,33.4111667671358,0.899796306780195));
#56735=CARTESIAN_POINT('Ctrl Pts',(4.34927019961831,33.4111030790715,0.903743099070193));
#56736=CARTESIAN_POINT('Ctrl Pts',(4.83587450315472,33.4108253785101,0.92242175897404));
#56737=CARTESIAN_POINT('Ctrl Pts',(5.72001145403567,33.4101755509066,0.967787576946441));
#56738=CARTESIAN_POINT('Ctrl Pts',(6.54876301828212,33.4101411791828,0.97075247449325));
#56739=CARTESIAN_POINT('Ctrl Pts',(7.19754212980654,33.4112032548265,0.880480590233061));
#56740=CARTESIAN_POINT('Ctrl Pts',(7.32550057368378,33.4115919397608,0.862020988728711));
#56741=CARTESIAN_POINT('Ctrl Pts',(7.52895904796954,33.4125344491362,0.830573953588618));
#56742=CARTESIAN_POINT('Ctrl Pts',(7.73081337870169,33.4137623486153,0.796794277431493));
#56743=CARTESIAN_POINT('Ctrl Pts',(8.14024610125225,33.416644671293,0.722660084039429));
#56744=CARTESIAN_POINT('Ctrl Pts',(8.76331513085336,33.4219612775907,0.585414526276326));
#56745=CARTESIAN_POINT('Ctrl Pts',(9.46278822378255,33.4256153655972,0.367459274710017));
#56746=CARTESIAN_POINT('Ctrl Pts',(10.0176548667882,33.4245339217562,0.141184776125187));
#56747=CARTESIAN_POINT('Ctrl Pts',(10.2919127083958,33.4221691705248,0.00852806418557635));
#56748=CARTESIAN_POINT('Ctrl Pts',(11.0596838975171,33.4121382406894,-0.39741540036137));
#56749=CARTESIAN_POINT('Ctrl Pts',(12.2113609303221,33.4016448516588,-1.27944658677757));
#56750=CARTESIAN_POINT('Ctrl Pts',(13.2034544750666,33.3476280317028,-2.31751121998455));
#56751=CARTESIAN_POINT('Ctrl Pts',(13.958790347696,33.2656790468827,-3.13274228974461));
#56752=CARTESIAN_POINT('Ctrl Pts',(14.542824409456,33.1913245084766,-3.83240360300729));
#56753=CARTESIAN_POINT('Ctrl Pts',(15.5915804267801,33.0041588224546,-5.29349765081425));
#56754=CARTESIAN_POINT('Ctrl Pts',(16.3123204181258,32.8020629110146,-6.45249308889002));
#56755=CARTESIAN_POINT('Ctrl Pts',(17.0563550542797,32.5245018229527,-7.64998966563405));
#56756=CARTESIAN_POINT('Ctrl Pts',(17.6162778419526,32.2852973888993,-8.61371409555214));
#56757=CARTESIAN_POINT('Ctrl Pts',(18.6451709005287,31.7226316969721,-10.5658949269178));
#56758=CARTESIAN_POINT('Ctrl Pts',(19.3594051248222,31.1901454406191,-12.0481304710539));
#56759=CARTESIAN_POINT('Ctrl Pts',(20.1008987914504,30.5386549627683,-13.5595949879592));
#56760=CARTESIAN_POINT('Ctrl Pts',(20.6466183193975,30.003280804915,-14.7231785594183));
#56761=CARTESIAN_POINT('Ctrl Pts',(21.6663807536096,28.7938945751524,-17.0275349953218));
#56762=CARTESIAN_POINT('Ctrl Pts',(22.3810364687107,27.7280363584589,-18.7018955338072));
#56763=CARTESIAN_POINT('Ctrl Pts',(23.5117483399784,25.8614793339912,-21.216829058667));
#56764=CARTESIAN_POINT('Ctrl Pts',(24.1480627906507,24.61701655753,-22.6285410064029));
#56765=CARTESIAN_POINT('Ctrl Pts',(24.7493903499091,23.2364939785392,-23.9577803684282));
#56766=CARTESIAN_POINT('Ctrl Pts',(2.09999999999999,38.9897510794637,0.9));
#56767=CARTESIAN_POINT('Ctrl Pts',(2.73333333333333,38.9897510794637,0.9));
#56768=CARTESIAN_POINT('Ctrl Pts',(3.36478879685081,38.9897220570697,0.89985896409509));
#56769=CARTESIAN_POINT('Ctrl Pts',(4.12107778498996,38.989713228803,0.899821396098744));
#56770=CARTESIAN_POINT('Ctrl Pts',(4.34481509744132,38.9896587133212,0.904351569922351));
#56771=CARTESIAN_POINT('Ctrl Pts',(4.82897515227901,38.989423652051,0.925991788001339));
#56772=CARTESIAN_POINT('Ctrl Pts',(5.71380230618561,38.9888696861857,0.979014362623941));
#56773=CARTESIAN_POINT('Ctrl Pts',(6.55610955603432,38.9888414597256,0.98318304814543));
#56774=CARTESIAN_POINT('Ctrl Pts',(7.21873857123617,38.9897305837832,0.875215691307443));
#56775=CARTESIAN_POINT('Ctrl Pts',(7.34686387089368,38.9901009601951,0.853636790127038));
#56776=CARTESIAN_POINT('Ctrl Pts',(7.55218952294518,38.991065815581,0.816553666708369));
#56777=CARTESIAN_POINT('Ctrl Pts',(7.75555264488831,38.9923519711669,0.776785625693149));
#56778=CARTESIAN_POINT('Ctrl Pts',(8.16869603838144,38.9953940636619,0.689360805961949));
#56779=CARTESIAN_POINT('Ctrl Pts',(8.79805341970188,39.0010104332016,0.527343393080334));
#56780=CARTESIAN_POINT('Ctrl Pts',(9.50502666554615,39.0043196140019,0.269763699750302));
#56781=CARTESIAN_POINT('Ctrl Pts',(10.064431266213,39.0020570255402,0.00315136578276065));
#56782=CARTESIAN_POINT('Ctrl Pts',(10.3401531790778,38.9987170953899,-0.152616667959919));
#56783=CARTESIAN_POINT('Ctrl Pts',(11.1103010543903,38.9852807309237,-0.627999100260067));
#56784=CARTESIAN_POINT('Ctrl Pts',(12.254576959855,38.9694318216162,-1.64974102780262));
#56785=CARTESIAN_POINT('Ctrl Pts',(13.2428711731431,38.9024766882624,-2.85423024818584));
#56786=CARTESIAN_POINT('Ctrl Pts',(13.9964017017256,38.8035591455185,-3.80267703087181));
#56787=CARTESIAN_POINT('Ctrl Pts',(14.5753786143845,38.7150140796801,-4.61020769734798));
#56788=CARTESIAN_POINT('Ctrl Pts',(15.6192592403265,38.492440052229,-6.30454904922076));
#56789=CARTESIAN_POINT('Ctrl Pts',(16.3373913183118,38.2535226204795,-7.65097529021429));
#56790=CARTESIAN_POINT('Ctrl Pts',(17.0806205854546,37.9256324686629,-9.04571732323448));
#56791=CARTESIAN_POINT('Ctrl Pts',(17.6370003403016,37.6452040748109,-10.1616972682833));
#56792=CARTESIAN_POINT('Ctrl Pts',(18.6627915222875,36.984538240599,-12.4306082839159));
#56793=CARTESIAN_POINT('Ctrl Pts',(19.3754523008299,36.3603136908351,-14.1544547728556));
#56794=CARTESIAN_POINT('Ctrl Pts',(20.1166123028179,35.5959813536198,-15.9150758011866));
#56795=CARTESIAN_POINT('Ctrl Pts',(20.6599948765211,34.970628879379,-17.26545899592));
#56796=CARTESIAN_POINT('Ctrl Pts',(21.6777842655078,33.5558510677647,-19.9461245033443));
#56797=CARTESIAN_POINT('Ctrl Pts',(22.391798977594,32.3094239354671,-21.8948863198921));
#56798=CARTESIAN_POINT('Ctrl Pts',(23.5225016210748,30.1253828617895,-24.8241019273224));
#56799=CARTESIAN_POINT('Ctrl Pts',(24.157514841919,28.6731789929379,-26.4644737024698));
#56800=CARTESIAN_POINT('Ctrl Pts',(24.7577717974218,27.0616688848421,-28.0099816319188));
#56801=CARTESIAN_POINT('',(24.5,19.2888993183199,-18.8928124716178));
#56802=CARTESIAN_POINT('Ctrl Pts',(24.5,19.2888993183199,-18.8928124716178));
#56803=CARTESIAN_POINT('Ctrl Pts',(24.5,18.4146674682996,-18.0152760071265));
#56804=CARTESIAN_POINT('Ctrl Pts',(24.5,17.5558967018297,-17.1519793443978));
#56805=CARTESIAN_POINT('Ctrl Pts',(24.5,14.0106747121728,-13.5812560497461));
#56806=CARTESIAN_POINT('Ctrl Pts',(24.5,10.2531955099118,-9.78418534540856));
#56807=CARTESIAN_POINT('Ctrl Pts',(24.5,7.16983932323689,-6.55422552562448));
#56808=CARTESIAN_POINT('',(10.2670750393577,34.1526563890204,0.));
#56809=CARTESIAN_POINT('Ctrl Pts',(10.2670750393577,34.1526563890204,-4.68375338513738E-16));
#56810=CARTESIAN_POINT('Ctrl Pts',(11.2293198185888,33.2721453537472,-0.465431410556517));
#56811=CARTESIAN_POINT('Ctrl Pts',(12.092802582344,32.5668339115407,-1.14700595996091));
#56812=CARTESIAN_POINT('Ctrl Pts',(14.3080979519049,30.8500805090056,-3.2126602051371));
#56813=CARTESIAN_POINT('Ctrl Pts',(14.8952017874601,30.4291106260349,-3.86523333611874));
#56814=CARTESIAN_POINT('Ctrl Pts',(17.0803363586062,28.6861024817812,-6.7160879710462));
#56815=CARTESIAN_POINT('Ctrl Pts',(17.6922811489506,28.1624534567924,-7.58672157878782));
#56816=CARTESIAN_POINT('Ctrl Pts',(19.0755427322033,26.8718943495686,-9.71692181817951));
#56817=CARTESIAN_POINT('Ctrl Pts',(20.2687424742408,25.6862391985472,-11.6130226450378));
#56818=CARTESIAN_POINT('Ctrl Pts',(22.3267279388309,22.9384152527353,-15.2120800399172));
#56819=CARTESIAN_POINT('Ctrl Pts',(23.4192562717209,21.3312428140497,-17.071137473725));
#56820=CARTESIAN_POINT('Ctrl Pts',(24.5,19.2888993183199,-18.8928124716178));
#56821=CARTESIAN_POINT('Ctrl Pts',(6.,38.9878978038234,0.971506478939046));
#56822=CARTESIAN_POINT('Ctrl Pts',(7.51604047332547,36.8303135352266,0.968297921939491));
#56823=CARTESIAN_POINT('Ctrl Pts',(9.08449301626627,35.2778821774931,0.481732853248133));
#56824=CARTESIAN_POINT('Ctrl Pts',(9.8624969752411,34.5273296915935,0.184503206613648));
#56825=CARTESIAN_POINT('Ctrl Pts',(10.0667253012217,34.3359882803962,0.0969078380449349));
#56826=CARTESIAN_POINT('Ctrl Pts',(10.2670750393577,34.1526563890204,1.64798730217797E-16));
#56827=CARTESIAN_POINT('Origin',(24.5,8.5,0.));
#56828=CARTESIAN_POINT('',(24.5,15.2746652201978,-22.2639754404033));
#56829=CARTESIAN_POINT('Ctrl Pts',(24.5,5.24229587453786,-8.17819063886291));
#56830=CARTESIAN_POINT('Ctrl Pts',(24.5,7.79421491150921,-11.6489323742096));
#56831=CARTESIAN_POINT('Ctrl Pts',(24.5,11.1172362590846,-16.3395906941412));
#56832=CARTESIAN_POINT('Ctrl Pts',(24.5,15.2746652201978,-22.2639754404033));
#56833=CARTESIAN_POINT('Origin',(24.5,0.,0.));
#56834=CARTESIAN_POINT('Ctrl Pts',(24.5,15.2746649873443,-22.2639756001573));
#56835=CARTESIAN_POINT('Ctrl Pts',(24.5,27.,-14.2195648714001));
#56836=CARTESIAN_POINT('Ctrl Pts',(24.5,27.,0.));
#56837=CARTESIAN_POINT('Ctrl Pts',(24.5,27.,27.));
#56838=CARTESIAN_POINT('Ctrl Pts',(24.5,0.,27.));
#56839=CARTESIAN_POINT('Ctrl Pts',(24.5,-27.,27.));
#56840=CARTESIAN_POINT('Ctrl Pts',(24.5,-27.,0.));
#56841=CARTESIAN_POINT('Ctrl Pts',(24.5,-27.,-27.));
#56842=CARTESIAN_POINT('Ctrl Pts',(24.5,0.,-27.));
#56843=CARTESIAN_POINT('Ctrl Pts',(24.5,8.37155243023015,-27.));
#56844=CARTESIAN_POINT('Ctrl Pts',(24.5,15.2746649873443,-22.2639756001573));
#56845=CARTESIAN_POINT('Ctrl Pts',(24.3078118955742,15.2932132103474,-22.2910110333212));
#56846=CARTESIAN_POINT('Ctrl Pts',(24.3078118955742,27.0327864487698,-14.2368318727032));
#56847=CARTESIAN_POINT('Ctrl Pts',(24.3078118955742,27.0327864487698,0.));
#56848=CARTESIAN_POINT('Ctrl Pts',(24.3078118955742,27.0327864487698,27.0327864487698));
#56849=CARTESIAN_POINT('Ctrl Pts',(24.3078118955742,0.,27.0327864487698));
#56850=CARTESIAN_POINT('Ctrl Pts',(24.3078118955742,-27.0327864487698,27.0327864487698));
#56851=CARTESIAN_POINT('Ctrl Pts',(24.3078118955742,-27.0327864487698,0.));
#56852=CARTESIAN_POINT('Ctrl Pts',(24.3078118955742,-27.0327864487698,-27.0327864487698));
#56853=CARTESIAN_POINT('Ctrl Pts',(24.3078118955742,0.,-27.0327864487698));
#56854=CARTESIAN_POINT('Ctrl Pts',(24.3078118955742,8.38171811448488,-27.0327864487698));
#56855=CARTESIAN_POINT('Ctrl Pts',(24.3078118955742,15.2932132103474,-22.2910110333212));
#56856=CARTESIAN_POINT('Ctrl Pts',(23.9225830034177,15.3326657652955,-22.348516106032));
#56857=CARTESIAN_POINT('Ctrl Pts',(23.9225830034177,27.1025240819344,-14.2735592356203));
#56858=CARTESIAN_POINT('Ctrl Pts',(23.9225830034177,27.1025240819344,0.));
#56859=CARTESIAN_POINT('Ctrl Pts',(23.9225830034177,27.1025240819344,27.1025240819344));
#56860=CARTESIAN_POINT('Ctrl Pts',(23.9225830034177,0.,27.1025240819344));
#56861=CARTESIAN_POINT('Ctrl Pts',(23.9225830034177,-27.1025240819344,27.1025240819344));
#56862=CARTESIAN_POINT('Ctrl Pts',(23.9225830034177,-27.1025240819344,0.));
#56863=CARTESIAN_POINT('Ctrl Pts',(23.9225830034177,-27.1025240819344,-27.1025240819344));
#56864=CARTESIAN_POINT('Ctrl Pts',(23.9225830034177,0.,-27.1025240819344));
#56865=CARTESIAN_POINT('Ctrl Pts',(23.9225830034177,8.40334079049961,-27.1025240819344));
#56866=CARTESIAN_POINT('Ctrl Pts',(23.9225830034177,15.3326657652955,-22.348516106032));
#56867=CARTESIAN_POINT('Ctrl Pts',(23.3421815947946,15.3989129006907,-22.4450762994792));
#56868=CARTESIAN_POINT('Ctrl Pts',(23.3421815947946,27.2196246963933,-14.3352303387232));
#56869=CARTESIAN_POINT('Ctrl Pts',(23.3421815947946,27.2196246963933,0.));
#56870=CARTESIAN_POINT('Ctrl Pts',(23.3421815947946,27.2196246963933,27.2196246963933));
#56871=CARTESIAN_POINT('Ctrl Pts',(23.3421815947946,0.,27.2196246963933));
#56872=CARTESIAN_POINT('Ctrl Pts',(23.3421815947946,-27.2196246963933,27.2196246963933));
#56873=CARTESIAN_POINT('Ctrl Pts',(23.3421815947946,-27.2196246963933,0.));
#56874=CARTESIAN_POINT('Ctrl Pts',(23.3421815947946,-27.2196246963933,-27.2196246963933));
#56875=CARTESIAN_POINT('Ctrl Pts',(23.3421815947946,0.,-27.2196246963933));
#56876=CARTESIAN_POINT('Ctrl Pts',(23.3421815947946,8.43964871396458,-27.2196246963933));
#56877=CARTESIAN_POINT('Ctrl Pts',(23.3421815947946,15.3989129006907,-22.4450762994792));
#56878=CARTESIAN_POINT('Ctrl Pts',(22.5631762070947,15.5014369037694,-22.5945127620704));
#56879=CARTESIAN_POINT('Ctrl Pts',(22.5631762070947,27.4008494948041,-14.4306724786236));
#56880=CARTESIAN_POINT('Ctrl Pts',(22.5631762070947,27.4008494948041,0.));
#56881=CARTESIAN_POINT('Ctrl Pts',(22.5631762070947,27.4008494948041,27.4008494948041));
#56882=CARTESIAN_POINT('Ctrl Pts',(22.5631762070947,0.,27.4008494948041));
#56883=CARTESIAN_POINT('Ctrl Pts',(22.5631762070947,-27.4008494948041,27.4008494948041));
#56884=CARTESIAN_POINT('Ctrl Pts',(22.5631762070947,-27.4008494948041,0.));
#56885=CARTESIAN_POINT('Ctrl Pts',(22.5631762070947,-27.4008494948041,-27.4008494948041));
#56886=CARTESIAN_POINT('Ctrl Pts',(22.5631762070947,0.,-27.4008494948041));
#56887=CARTESIAN_POINT('Ctrl Pts',(22.5631762070947,8.49583882142956,-27.4008494948041));
#56888=CARTESIAN_POINT('Ctrl Pts',(22.5631762070947,15.5014369037694,-22.5945127620704));
#56889=CARTESIAN_POINT('Ctrl Pts',(21.5808622776984,15.6536636723535,-22.8163947519049));
#56890=CARTESIAN_POINT('Ctrl Pts',(21.5808622776984,27.6699305355455,-14.5723841569379));
#56891=CARTESIAN_POINT('Ctrl Pts',(21.5808622776984,27.6699305355455,0.));
#56892=CARTESIAN_POINT('Ctrl Pts',(21.5808622776984,27.6699305355455,27.6699305355455));
#56893=CARTESIAN_POINT('Ctrl Pts',(21.5808622776984,0.,27.6699305355455));
#56894=CARTESIAN_POINT('Ctrl Pts',(21.5808622776984,-27.6699305355455,27.6699305355455));
#56895=CARTESIAN_POINT('Ctrl Pts',(21.5808622776984,-27.6699305355455,0.));
#56896=CARTESIAN_POINT('Ctrl Pts',(21.5808622776984,-27.6699305355455,-27.6699305355455));
#56897=CARTESIAN_POINT('Ctrl Pts',(21.5808622776984,0.,-27.6699305355455));
#56898=CARTESIAN_POINT('Ctrl Pts',(21.5808622776984,8.57926941552391,-27.6699305355455));
#56899=CARTESIAN_POINT('Ctrl Pts',(21.5808622776984,15.6536636723535,-22.8163947519049));
#56900=CARTESIAN_POINT('Ctrl Pts',(20.5902243197586,15.8306138323376,-23.0743129483166));
#56901=CARTESIAN_POINT('Ctrl Pts',(20.5902243197586,27.9827134557292,-14.7371114541311));
#56902=CARTESIAN_POINT('Ctrl Pts',(20.5902243197586,27.9827134557292,0.));
#56903=CARTESIAN_POINT('Ctrl Pts',(20.5902243197586,27.9827134557292,27.9827134557292));
#56904=CARTESIAN_POINT('Ctrl Pts',(20.5902243197586,0.,27.9827134557292));
#56905=CARTESIAN_POINT('Ctrl Pts',(20.5902243197586,-27.9827134557292,27.9827134557292));
#56906=CARTESIAN_POINT('Ctrl Pts',(20.5902243197586,-27.9827134557292,0.));
#56907=CARTESIAN_POINT('Ctrl Pts',(20.5902243197586,-27.9827134557292,-27.9827134557292));
#56908=CARTESIAN_POINT('Ctrl Pts',(20.5902243197586,0.,-27.9827134557292));
#56909=CARTESIAN_POINT('Ctrl Pts',(20.5902243197586,8.6762501049905,-27.9827134557292));
#56910=CARTESIAN_POINT('Ctrl Pts',(20.5902243197586,15.8306138323376,-23.0743129483166));
#56911=CARTESIAN_POINT('Ctrl Pts',(19.591895069338,16.0331232490547,-23.3694856880348));
#56912=CARTESIAN_POINT('Ctrl Pts',(19.591895069338,28.3406757583979,-14.9256324979946));
#56913=CARTESIAN_POINT('Ctrl Pts',(19.591895069338,28.3406757583979,0.));
#56914=CARTESIAN_POINT('Ctrl Pts',(19.591895069338,28.3406757583979,28.3406757583979));
#56915=CARTESIAN_POINT('Ctrl Pts',(19.591895069338,0.,28.3406757583979));
#56916=CARTESIAN_POINT('Ctrl Pts',(19.591895069338,-28.3406757583979,28.3406757583979));
#56917=CARTESIAN_POINT('Ctrl Pts',(19.591895069338,-28.3406757583979,0.));
#56918=CARTESIAN_POINT('Ctrl Pts',(19.591895069338,-28.3406757583979,-28.3406757583979));
#56919=CARTESIAN_POINT('Ctrl Pts',(19.591895069338,0.,-28.3406757583979));
#56920=CARTESIAN_POINT('Ctrl Pts',(19.591895069338,8.78723900072521,-28.3406757583979));
#56921=CARTESIAN_POINT('Ctrl Pts',(19.591895069338,16.0331232490547,-23.3694856880348));
#56922=CARTESIAN_POINT('Ctrl Pts',(18.5871162949016,16.2621527784708,-23.7033134910576));
#56923=CARTESIAN_POINT('Ctrl Pts',(18.5871162949016,28.7455158841458,-15.1388417732027));
#56924=CARTESIAN_POINT('Ctrl Pts',(18.5871162949016,28.7455158841458,0.));
#56925=CARTESIAN_POINT('Ctrl Pts',(18.5871162949016,28.7455158841458,28.7455158841458));
#56926=CARTESIAN_POINT('Ctrl Pts',(18.5871162949016,0.,28.7455158841458));
#56927=CARTESIAN_POINT('Ctrl Pts',(18.5871162949016,-28.7455158841458,28.7455158841458));
#56928=CARTESIAN_POINT('Ctrl Pts',(18.5871162949016,-28.7455158841458,0.));
#56929=CARTESIAN_POINT('Ctrl Pts',(18.5871162949016,-28.7455158841458,-28.7455158841458));
#56930=CARTESIAN_POINT('Ctrl Pts',(18.5871162949016,0.,-28.7455158841458));
#56931=CARTESIAN_POINT('Ctrl Pts',(18.5871162949016,8.91276271696817,-28.7455158841458));
#56932=CARTESIAN_POINT('Ctrl Pts',(18.5871162949016,16.2621527784708,-23.7033134910576));
#56933=CARTESIAN_POINT('Ctrl Pts',(17.577868433379,16.5186756279781,-24.0772148805183));
#56934=CARTESIAN_POINT('Ctrl Pts',(17.577868433379,29.1989541063548,-15.3776452626794));
#56935=CARTESIAN_POINT('Ctrl Pts',(17.577868433379,29.1989541063548,0.));
#56936=CARTESIAN_POINT('Ctrl Pts',(17.577868433379,29.1989541063548,29.1989541063548));
#56937=CARTESIAN_POINT('Ctrl Pts',(17.577868433379,0.,29.1989541063548));
#56938=CARTESIAN_POINT('Ctrl Pts',(17.577868433379,-29.1989541063548,29.1989541063548));
#56939=CARTESIAN_POINT('Ctrl Pts',(17.577868433379,-29.1989541063548,0.));
#56940=CARTESIAN_POINT('Ctrl Pts',(17.577868433379,-29.1989541063548,-29.1989541063548));
#56941=CARTESIAN_POINT('Ctrl Pts',(17.577868433379,0.,-29.1989541063548));
#56942=CARTESIAN_POINT('Ctrl Pts',(17.577868433379,9.053354637379,-29.1989541063548));
#56943=CARTESIAN_POINT('Ctrl Pts',(17.577868433379,16.5186756279781,-24.0772148805183));
#56944=CARTESIAN_POINT('Ctrl Pts',(16.5668667015923,16.8035054746331,-24.4923758520602));
#56945=CARTESIAN_POINT('Ctrl Pts',(16.5668667015923,29.7024287073398,-15.6428004385983));
#56946=CARTESIAN_POINT('Ctrl Pts',(16.5668667015923,29.7024287073398,0.));
#56947=CARTESIAN_POINT('Ctrl Pts',(16.5668667015923,29.7024287073398,29.7024287073398));
#56948=CARTESIAN_POINT('Ctrl Pts',(16.5668667015923,0.,29.7024287073398));
#56949=CARTESIAN_POINT('Ctrl Pts',(16.5668667015923,-29.7024287073398,29.7024287073398));
#56950=CARTESIAN_POINT('Ctrl Pts',(16.5668667015923,-29.7024287073398,0.));
#56951=CARTESIAN_POINT('Ctrl Pts',(16.5668667015923,-29.7024287073398,-29.7024287073398));
#56952=CARTESIAN_POINT('Ctrl Pts',(16.5668667015923,0.,-29.7024287073398));
#56953=CARTESIAN_POINT('Ctrl Pts',(16.5668667015923,9.20946071217291,-29.7024287073398));
#56954=CARTESIAN_POINT('Ctrl Pts',(16.5668667015923,16.8035054746331,-24.4923758520602));
#56955=CARTESIAN_POINT('Ctrl Pts',(15.5576189940876,17.1170945776568,-24.9494556075887));
#56956=CARTESIAN_POINT('Ctrl Pts',(15.5576189940876,30.2567391153688,-15.9347283202968));
#56957=CARTESIAN_POINT('Ctrl Pts',(15.5576189940876,30.2567391153688,0.));
#56958=CARTESIAN_POINT('Ctrl Pts',(15.5576189940876,30.2567391153687,30.2567391153687));
#56959=CARTESIAN_POINT('Ctrl Pts',(15.5576189940876,0.,30.2567391153688));
#56960=CARTESIAN_POINT('Ctrl Pts',(15.5576189940876,-30.2567391153687,30.2567391153687));
#56961=CARTESIAN_POINT('Ctrl Pts',(15.5576189940876,-30.2567391153688,0.));
#56962=CARTESIAN_POINT('Ctrl Pts',(15.5576189940876,-30.2567391153687,-30.2567391153687));
#56963=CARTESIAN_POINT('Ctrl Pts',(15.5576189940876,0.,-30.2567391153688));
#56964=CARTESIAN_POINT('Ctrl Pts',(15.5576189940876,9.38132881007796,-30.2567391153688));
#56965=CARTESIAN_POINT('Ctrl Pts',(15.5576189940876,17.1170945776568,-24.9494556075887));
#56966=CARTESIAN_POINT('Ctrl Pts',(14.5544447688713,17.4593421723157,-25.4483072749091));
#56967=CARTESIAN_POINT('Ctrl Pts',(14.5544447688713,30.8617072153858,-16.2533351033827));
#56968=CARTESIAN_POINT('Ctrl Pts',(14.5544447688713,30.8617072153858,0.));
#56969=CARTESIAN_POINT('Ctrl Pts',(14.5544447688713,30.8617072153858,30.8617072153858));
#56970=CARTESIAN_POINT('Ctrl Pts',(14.5544447688713,0.,30.8617072153858));
#56971=CARTESIAN_POINT('Ctrl Pts',(14.5544447688713,-30.8617072153858,30.8617072153858));
#56972=CARTESIAN_POINT('Ctrl Pts',(14.5544447688713,-30.8617072153858,0.));
#56973=CARTESIAN_POINT('Ctrl Pts',(14.5544447688713,-30.8617072153858,-30.8617072153858));
#56974=CARTESIAN_POINT('Ctrl Pts',(14.5544447688713,0.,-30.8617072153858));
#56975=CARTESIAN_POINT('Ctrl Pts',(14.5544447688713,9.56890370518571,-30.8617072153858));
#56976=CARTESIAN_POINT('Ctrl Pts',(14.5544447688713,17.4593421723157,-25.4483072749091));
#56977=CARTESIAN_POINT('Ctrl Pts',(13.5625963827217,17.8292752645412,-25.9875126418238));
#56978=CARTESIAN_POINT('Ctrl Pts',(13.5625963827217,31.5156131110873,-16.5977150035204));
#56979=CARTESIAN_POINT('Ctrl Pts',(13.5625963827217,31.5156131110873,0.));
#56980=CARTESIAN_POINT('Ctrl Pts',(13.5625963827217,31.5156131110873,31.5156131110873));
#56981=CARTESIAN_POINT('Ctrl Pts',(13.5625963827217,0.,31.5156131110873));
#56982=CARTESIAN_POINT('Ctrl Pts',(13.5625963827217,-31.5156131110873,31.5156131110873));
#56983=CARTESIAN_POINT('Ctrl Pts',(13.5625963827217,-31.5156131110873,0.));
#56984=CARTESIAN_POINT('Ctrl Pts',(13.5625963827217,-31.5156131110873,-31.5156131110873));
#56985=CARTESIAN_POINT('Ctrl Pts',(13.5625963827217,0.,-31.5156131110873));
#56986=CARTESIAN_POINT('Ctrl Pts',(13.5625963827217,9.77165213075244,-31.5156131110873));
#56987=CARTESIAN_POINT('Ctrl Pts',(13.5625963827217,17.8292752645412,-25.9875126418238));
#56988=CARTESIAN_POINT('Ctrl Pts',(12.5880795783847,18.2250438427861,-26.5643751770515));
#56989=CARTESIAN_POINT('Ctrl Pts',(12.5880795783847,32.2151866612413,-16.966145799029));
#56990=CARTESIAN_POINT('Ctrl Pts',(12.5880795783847,32.2151866612413,0.));
#56991=CARTESIAN_POINT('Ctrl Pts',(12.5880795783847,32.2151866612413,32.2151866612413));
#56992=CARTESIAN_POINT('Ctrl Pts',(12.5880795783847,0.,32.2151866612413));
#56993=CARTESIAN_POINT('Ctrl Pts',(12.5880795783847,-32.2151866612413,32.2151866612413));
#56994=CARTESIAN_POINT('Ctrl Pts',(12.5880795783847,-32.2151866612413,0.));
#56995=CARTESIAN_POINT('Ctrl Pts',(12.5880795783847,-32.2151866612413,-32.2151866612413));
#56996=CARTESIAN_POINT('Ctrl Pts',(12.5880795783847,0.,-32.2151866612413));
#56997=CARTESIAN_POINT('Ctrl Pts',(12.5880795783847,9.98856015497159,-32.2151866612413));
#56998=CARTESIAN_POINT('Ctrl Pts',(12.5880795783847,18.2250438427861,-26.5643751770515));
#56999=CARTESIAN_POINT('Ctrl Pts',(11.6370973936883,18.6443245145603,-27.1755083609041));
#57000=CARTESIAN_POINT('Ctrl Pts',(11.6370973936883,32.9563209608992,-17.3564645861551));
#57001=CARTESIAN_POINT('Ctrl Pts',(11.6370973936883,32.9563209608992,0.));
#57002=CARTESIAN_POINT('Ctrl Pts',(11.6370973936883,32.9563209608992,32.9563209608992));
#57003=CARTESIAN_POINT('Ctrl Pts',(11.6370973936883,0.,32.9563209608992));
#57004=CARTESIAN_POINT('Ctrl Pts',(11.6370973936883,-32.9563209608992,32.9563209608992));
#57005=CARTESIAN_POINT('Ctrl Pts',(11.6370973936883,-32.9563209608992,0.));
#57006=CARTESIAN_POINT('Ctrl Pts',(11.6370973936883,-32.9563209608992,-32.9563209608992));
#57007=CARTESIAN_POINT('Ctrl Pts',(11.6370973936883,0.,-32.9563209608992));
#57008=CARTESIAN_POINT('Ctrl Pts',(11.6370973936883,10.2183544011726,-32.9563209608992));
#57009=CARTESIAN_POINT('Ctrl Pts',(11.6370973936883,18.6443245145603,-27.1755083609041));
#57010=CARTESIAN_POINT('Ctrl Pts',(10.7155646400367,19.084590376709,-27.8172290415595));
#57011=CARTESIAN_POINT('Ctrl Pts',(10.7155646400367,33.7345493729701,-17.7663190080147));
#57012=CARTESIAN_POINT('Ctrl Pts',(10.7155646400367,33.7345493729701,0.));
#57013=CARTESIAN_POINT('Ctrl Pts',(10.7155646400367,33.7345493729701,33.7345493729701));
#57014=CARTESIAN_POINT('Ctrl Pts',(10.7155646400367,0.,33.7345493729701));
#57015=CARTESIAN_POINT('Ctrl Pts',(10.7155646400367,-33.7345493729701,33.7345493729701));
#57016=CARTESIAN_POINT('Ctrl Pts',(10.7155646400367,-33.7345493729701,0.));
#57017=CARTESIAN_POINT('Ctrl Pts',(10.7155646400367,-33.7345493729701,-33.7345493729701));
#57018=CARTESIAN_POINT('Ctrl Pts',(10.7155646400367,0.,-33.7345493729701));
#57019=CARTESIAN_POINT('Ctrl Pts',(10.7155646400367,10.4596499550373,-33.7345493729701));
#57020=CARTESIAN_POINT('Ctrl Pts',(10.7155646400367,19.084590376709,-27.8172290415595));
#57021=CARTESIAN_POINT('Ctrl Pts',(9.82859575068344,19.5433963611581,-28.485973347994));
#57022=CARTESIAN_POINT('Ctrl Pts',(9.82859575068344,34.5455499147423,-18.1934328900321));
#57023=CARTESIAN_POINT('Ctrl Pts',(9.82859575068344,34.5455499147423,0.));
#57024=CARTESIAN_POINT('Ctrl Pts',(9.82859575068344,34.5455499147423,34.5455499147423));
#57025=CARTESIAN_POINT('Ctrl Pts',(9.82859575068344,0.,34.5455499147423));
#57026=CARTESIAN_POINT('Ctrl Pts',(9.82859575068344,-34.5455499147423,34.5455499147423));
#57027=CARTESIAN_POINT('Ctrl Pts',(9.82859575068344,-34.5455499147423,0.));
#57028=CARTESIAN_POINT('Ctrl Pts',(9.82859575068344,-34.5455499147423,-34.5455499147423));
#57029=CARTESIAN_POINT('Ctrl Pts',(9.82859575068344,0.,-34.5455499147423));
#57030=CARTESIAN_POINT('Ctrl Pts',(9.82859575068344,10.7111067534221,-34.5455499147423));
#57031=CARTESIAN_POINT('Ctrl Pts',(9.82859575068344,19.5433963611581,-28.485973347994));
#57032=CARTESIAN_POINT('Ctrl Pts',(8.97989469943246,20.0186512506371,-29.1786931734031));
#57033=CARTESIAN_POINT('Ctrl Pts',(8.97989469943246,35.3856260818179,-18.6358594661302));
#57034=CARTESIAN_POINT('Ctrl Pts',(8.97989469943246,35.3856260818179,0.));
#57035=CARTESIAN_POINT('Ctrl Pts',(8.97989469943246,35.3856260818179,35.3856260818179));
#57036=CARTESIAN_POINT('Ctrl Pts',(8.97989469943246,0.,35.3856260818179));
#57037=CARTESIAN_POINT('Ctrl Pts',(8.97989469943246,-35.3856260818179,35.3856260818179));
#57038=CARTESIAN_POINT('Ctrl Pts',(8.97989469943246,-35.3856260818179,0.));
#57039=CARTESIAN_POINT('Ctrl Pts',(8.97989469943246,-35.3856260818179,-35.3856260818179));
#57040=CARTESIAN_POINT('Ctrl Pts',(8.97989469943246,0.,-35.3856260818179));
#57041=CARTESIAN_POINT('Ctrl Pts',(8.97989469943246,10.9715786674244,-35.3856260818179));
#57042=CARTESIAN_POINT('Ctrl Pts',(8.97989469943246,20.0186512506371,-29.1786931734031));
#57043=CARTESIAN_POINT('Ctrl Pts',(8.1713316609345,20.5088253880975,-29.8931589273354));
#57044=CARTESIAN_POINT('Ctrl Pts',(8.1713316609345,36.2520740021093,-19.0921747405847));
#57045=CARTESIAN_POINT('Ctrl Pts',(8.1713316609345,36.2520740021093,0.));
#57046=CARTESIAN_POINT('Ctrl Pts',(8.1713316609345,36.2520740021093,36.2520740021093));
#57047=CARTESIAN_POINT('Ctrl Pts',(8.1713316609345,0.,36.2520740021093));
#57048=CARTESIAN_POINT('Ctrl Pts',(8.1713316609345,-36.2520740021093,36.2520740021093));
#57049=CARTESIAN_POINT('Ctrl Pts',(8.1713316609345,-36.2520740021093,0.));
#57050=CARTESIAN_POINT('Ctrl Pts',(8.1713316609345,-36.2520740021093,-36.2520740021093));
#57051=CARTESIAN_POINT('Ctrl Pts',(8.1713316609345,0.,-36.2520740021093));
#57052=CARTESIAN_POINT('Ctrl Pts',(8.1713316609345,11.2402273412312,-36.2520740021093));
#57053=CARTESIAN_POINT('Ctrl Pts',(8.1713316609345,20.5088253880975,-29.8931589273354));
#57054=CARTESIAN_POINT('Ctrl Pts',(7.40358438374929,21.0128566018474,-30.6278224144852));
#57055=CARTESIAN_POINT('Ctrl Pts',(7.40358438374929,37.1430161460138,-19.5613899113964));
#57056=CARTESIAN_POINT('Ctrl Pts',(7.40358438374929,37.1430161460139,0.));
#57057=CARTESIAN_POINT('Ctrl Pts',(7.40358438374929,37.1430161460138,37.1430161460138));
#57058=CARTESIAN_POINT('Ctrl Pts',(7.40358438374929,0.,37.1430161460139));
#57059=CARTESIAN_POINT('Ctrl Pts',(7.40358438374929,-37.1430161460138,37.1430161460138));
#57060=CARTESIAN_POINT('Ctrl Pts',(7.40358438374929,-37.1430161460139,0.));
#57061=CARTESIAN_POINT('Ctrl Pts',(7.40358438374929,-37.1430161460138,-37.1430161460138));
#57062=CARTESIAN_POINT('Ctrl Pts',(7.40358438374929,0.,-37.1430161460139));
#57063=CARTESIAN_POINT('Ctrl Pts',(7.40358438374929,11.5164706327126,-37.1430161460138));
#57064=CARTESIAN_POINT('Ctrl Pts',(7.40358438374929,21.0128566018474,-30.6278224144852));
#57065=CARTESIAN_POINT('Ctrl Pts',(6.82198164612729,21.426644412938,-31.2309493398479));
#57066=CARTESIAN_POINT('Ctrl Pts',(6.82198164612729,37.8744410845445,-19.946595258137));
#57067=CARTESIAN_POINT('Ctrl Pts',(6.82198164612729,37.8744410845445,0.));
#57068=CARTESIAN_POINT('Ctrl Pts',(6.82198164612729,37.8744410845445,37.8744410845445));
#57069=CARTESIAN_POINT('Ctrl Pts',(6.82198164612729,0.,37.8744410845445));
#57070=CARTESIAN_POINT('Ctrl Pts',(6.82198164612729,-37.8744410845445,37.8744410845445));
#57071=CARTESIAN_POINT('Ctrl Pts',(6.82198164612729,-37.8744410845445,0.));
#57072=CARTESIAN_POINT('Ctrl Pts',(6.82198164612729,-37.8744410845445,-37.8744410845445));
#57073=CARTESIAN_POINT('Ctrl Pts',(6.82198164612729,0.,-37.8744410845445));
#57074=CARTESIAN_POINT('Ctrl Pts',(6.82198164612729,11.743254418701,-37.8744410845445));
#57075=CARTESIAN_POINT('Ctrl Pts',(6.82198164612729,21.426644412938,-31.2309493398479));
#57076=CARTESIAN_POINT('Ctrl Pts',(6.40395249919757,21.7427802361891,-31.6917411320757));
#57077=CARTESIAN_POINT('Ctrl Pts',(6.40395249919757,38.433253158973,-20.2408939449244));
#57078=CARTESIAN_POINT('Ctrl Pts',(6.40395249919757,38.433253158973,0.));
#57079=CARTESIAN_POINT('Ctrl Pts',(6.40395249919757,38.433253158973,38.433253158973));
#57080=CARTESIAN_POINT('Ctrl Pts',(6.40395249919757,0.,38.433253158973));
#57081=CARTESIAN_POINT('Ctrl Pts',(6.40395249919757,-38.433253158973,38.433253158973));
#57082=CARTESIAN_POINT('Ctrl Pts',(6.40395249919757,-38.433253158973,0.));
#57083=CARTESIAN_POINT('Ctrl Pts',(6.40395249919757,-38.433253158973,-38.433253158973));
#57084=CARTESIAN_POINT('Ctrl Pts',(6.40395249919757,0.,-38.433253158973));
#57085=CARTESIAN_POINT('Ctrl Pts',(6.40395249919757,11.9165182920241,-38.433253158973));
#57086=CARTESIAN_POINT('Ctrl Pts',(6.40395249919757,21.7427802361891,-31.6917411320757));
#57087=CARTESIAN_POINT('Ctrl Pts',(6.13331019225912,21.9561025509032,-32.0026744856845));
#57088=CARTESIAN_POINT('Ctrl Pts',(6.13331019225912,38.8103286956251,-20.4394809839926));
#57089=CARTESIAN_POINT('Ctrl Pts',(6.13331019225912,38.8103286956251,0.));
#57090=CARTESIAN_POINT('Ctrl Pts',(6.13331019225912,38.8103286956251,38.8103286956251));
#57091=CARTESIAN_POINT('Ctrl Pts',(6.13331019225912,0.,38.8103286956251));
#57092=CARTESIAN_POINT('Ctrl Pts',(6.13331019225912,-38.8103286956251,38.8103286956251));
#57093=CARTESIAN_POINT('Ctrl Pts',(6.13331019225912,-38.8103286956251,0.));
#57094=CARTESIAN_POINT('Ctrl Pts',(6.13331019225912,-38.8103286956251,-38.8103286956251));
#57095=CARTESIAN_POINT('Ctrl Pts',(6.13331019225912,0.,-38.8103286956251));
#57096=CARTESIAN_POINT('Ctrl Pts',(6.13331019225912,12.0334333892552,-38.8103286956251));
#57097=CARTESIAN_POINT('Ctrl Pts',(6.13331019225912,21.9561025509032,-32.0026744856845));
#57098=CARTESIAN_POINT('Ctrl Pts',(6.,22.0634049817195,-32.1590758668939));
#57099=CARTESIAN_POINT('Ctrl Pts',(6.,39.,-20.5393714809112));
#57100=CARTESIAN_POINT('Ctrl Pts',(6.,39.,0.));
#57101=CARTESIAN_POINT('Ctrl Pts',(6.,39.,39.));
#57102=CARTESIAN_POINT('Ctrl Pts',(6.,0.,39.));
#57103=CARTESIAN_POINT('Ctrl Pts',(6.,-39.,39.));
#57104=CARTESIAN_POINT('Ctrl Pts',(6.,-39.,0.));
#57105=CARTESIAN_POINT('Ctrl Pts',(6.,-39.,-39.));
#57106=CARTESIAN_POINT('Ctrl Pts',(6.,0.,-39.));
#57107=CARTESIAN_POINT('Ctrl Pts',(6.,12.0922423992213,-39.));
#57108=CARTESIAN_POINT('Ctrl Pts',(6.,22.0634049817195,-32.1590758668939));
#57109=CARTESIAN_POINT('Ctrl Pts',(24.5,15.2746652201978,-22.2639754404033));
#57110=CARTESIAN_POINT('Ctrl Pts',(23.5178991898112,17.7900297317948,-20.7414389863023));
#57111=CARTESIAN_POINT('Ctrl Pts',(22.3947886245986,20.0495645305202,-18.9195767222114));
#57112=CARTESIAN_POINT('Ctrl Pts',(21.1743874927566,22.0660835472267,-16.915405191777));
#57113=CARTESIAN_POINT('Ctrl Pts',(20.5031871793432,23.1751354488541,-15.8131442021206));
#57114=CARTESIAN_POINT('Ctrl Pts',(19.8411792966403,24.2071629062566,-14.6351278759304));
#57115=CARTESIAN_POINT('Ctrl Pts',(19.1295827650253,25.1714380797582,-13.4354459468032));
#57116=CARTESIAN_POINT('Ctrl Pts',(18.8261415870907,25.5826272600038,-12.9238738950185));
#57117=CARTESIAN_POINT('Ctrl Pts',(18.5104994276268,25.9850411393693,-12.404332641861));
#57118=CARTESIAN_POINT('Ctrl Pts',(18.2016639423759,26.3553711077349,-11.9183617880446));
#57119=CARTESIAN_POINT('Ctrl Pts',(17.6747132403628,26.987246802486,-11.0891737743408));
#57120=CARTESIAN_POINT('Ctrl Pts',(17.2016343370984,27.5228289338585,-10.3269493110331));
#57121=CARTESIAN_POINT('Ctrl Pts',(16.8729352926451,27.8805533220886,-9.81400929094393));
#57122=CARTESIAN_POINT('Ctrl Pts',(16.6342454025473,28.1403204140616,-9.44152996954687));
#57123=CARTESIAN_POINT('Ctrl Pts',(16.5014949770662,28.2793135182913,-9.23929506825468));
#57124=CARTESIAN_POINT('Ctrl Pts',(16.3424569562978,28.4442683427237,-9.00014216371263));
#57125=CARTESIAN_POINT('Ctrl Pts',(15.993118510103,28.8066034735382,-8.47482561568167));
#57126=CARTESIAN_POINT('Ctrl Pts',(15.6312480487537,29.1643380375821,-7.95419476716189));
#57127=CARTESIAN_POINT('Ctrl Pts',(15.2503296894305,29.5245094879835,-7.44978258413541));
#57128=CARTESIAN_POINT('Ctrl Pts',(14.7484414179076,29.9990621638247,-6.78518201428077));
#57129=CARTESIAN_POINT('Ctrl Pts',(14.2669345517206,30.4475318788827,-6.13744034835409));
#57130=CARTESIAN_POINT('Ctrl Pts',(13.7912435751455,30.8800117840353,-5.54611601085555));
#57131=CARTESIAN_POINT('Ctrl Pts',(13.5533980868579,31.0962517366116,-5.25045384210628));
#57132=CARTESIAN_POINT('Ctrl Pts',(13.3161115657262,31.3096390113264,-4.9671616086599));
#57133=CARTESIAN_POINT('Ctrl Pts',(13.0766514227367,31.5235559498616,-4.69823014337086));
#57134=CARTESIAN_POINT('Ctrl Pts',(12.9188702359555,31.6645066233779,-4.52103019173643));
#57135=CARTESIAN_POINT('Ctrl Pts',(12.7601526360409,31.8056928422568,-4.35006042750501));
#57136=CARTESIAN_POINT('Ctrl Pts',(12.5997389313808,31.9481916423883,-4.1859403999119));
#57137=CARTESIAN_POINT('Ctrl Pts',(12.5166971934814,32.0219593297351,-4.10098000114603));
#57138=CARTESIAN_POINT('Ctrl Pts',(12.4397215765388,32.0902904057789,-4.02412719470386));
#57139=CARTESIAN_POINT('Ctrl Pts',(12.3478597934844,32.1718560071766,-3.93542897845831));
#57140=CARTESIAN_POINT('Ctrl Pts',(11.9116121727781,32.5592075080742,-3.51420499922096));
#57141=CARTESIAN_POINT('Ctrl Pts',(10.7144663992386,33.6238209182471,-2.28350062373506));
#57142=CARTESIAN_POINT('Ctrl Pts',(9.56604185022483,34.7743191636545,-1.6807321648514));
#57143=CARTESIAN_POINT('Ctrl Pts',(9.07284645450772,35.2684051163649,-1.42187090238518));
#57144=CARTESIAN_POINT('Ctrl Pts',(8.57333454992768,35.7900679626755,-1.25277516408929));
#57145=CARTESIAN_POINT('Ctrl Pts',(8.00348148263049,36.4414959462974,-1.11294819927946));
#57146=CARTESIAN_POINT('Ctrl Pts',(7.63919428965959,36.8579311384459,-1.02356169697667));
#57147=CARTESIAN_POINT('Ctrl Pts',(7.2438864438469,37.3374667334074,-0.951049621039589));
#57148=CARTESIAN_POINT('Ctrl Pts',(6.94254646282579,37.7220011048021,-0.902244736766912));
#57149=CARTESIAN_POINT('Ctrl Pts',(6.91433564865295,37.7580004025312,-0.897675726321375));
#57150=CARTESIAN_POINT('Ctrl Pts',(6.88669635040567,37.7934387743179,-0.89325998801799));
#57151=CARTESIAN_POINT('Ctrl Pts',(6.85962514029878,37.8283036072989,-0.888985319768479));
#57152=CARTESIAN_POINT('Ctrl Pts',(6.44000062073739,38.368735258912,-0.822724683343163));
#57153=CARTESIAN_POINT('Ctrl Pts',(6.15412442492902,38.7718575486186,-0.828800771638793));
#57154=CARTESIAN_POINT('Ctrl Pts',(6.,38.9911990462069,-0.828490759799982));
#57155=CARTESIAN_POINT('Ctrl Pts',(2.09999999999999,9.70057967382468,-0.9));
#57156=CARTESIAN_POINT('Ctrl Pts',(2.73333333333332,9.70057967382468,-0.9));
#57157=CARTESIAN_POINT('Ctrl Pts',(3.36699574607395,9.70059005321194,-0.899942825180981));
#57158=CARTESIAN_POINT('Ctrl Pts',(4.12579817395472,9.70059327517204,-0.899925538426819));
#57159=CARTESIAN_POINT('Ctrl Pts',(4.38275749788984,9.7007262380907,-0.898639486126413));
#57160=CARTESIAN_POINT('Ctrl Pts',(4.88872023230434,9.7013226080202,-0.892940393354486));
#57161=CARTESIAN_POINT('Ctrl Pts',(5.76576815117897,9.7027126091003,-0.879800331845227));
#57162=CARTESIAN_POINT('Ctrl Pts',(6.49294800367276,9.70272682384117,-0.880004039269183));
#57163=CARTESIAN_POINT('Ctrl Pts',(7.02334978980851,9.7003499446892,-0.901450813685861));
#57164=CARTESIAN_POINT('Ctrl Pts',(7.14973151012377,9.69983015215563,-0.906734178368804));
#57165=CARTESIAN_POINT('Ctrl Pts',(7.39956059419753,9.69883105549345,-0.917970126739818));
#57166=CARTESIAN_POINT('Ctrl Pts',(7.71335439531399,9.69758466503641,-0.933748103679502));
#57167=CARTESIAN_POINT('Ctrl Pts',(8.08760778694771,9.69583752317872,-0.956004462473258));
#57168=CARTESIAN_POINT('Ctrl Pts',(8.58202753816148,9.69285898041634,-0.99085924708594));
#57169=CARTESIAN_POINT('Ctrl Pts',(9.18585213220259,9.68729348127799,-1.04563537764413));
#57170=CARTESIAN_POINT('Ctrl Pts',(9.64252060159779,9.67961272832539,-1.10407520282726));
#57171=CARTESIAN_POINT('Ctrl Pts',(10.3691727925248,9.66316415892935,-1.21502210418074));
#57172=CARTESIAN_POINT('Ctrl Pts',(11.1023934939471,9.64291586397951,-1.37505182297649));
#57173=CARTESIAN_POINT('Ctrl Pts',(12.0425471796807,9.60260179231032,-1.63666268571367));
#57174=CARTESIAN_POINT('Ctrl Pts',(12.4995913073701,9.57670316757122,-1.77585592157297));
#57175=CARTESIAN_POINT('Ctrl Pts',(13.0011491477499,9.54392598331016,-1.93113784163963));
#57176=CARTESIAN_POINT('Ctrl Pts',(13.5006102383397,9.50612955297879,-2.1025105735227));
#57177=CARTESIAN_POINT('Ctrl Pts',(14.4710708057365,9.41550916749915,-2.48724983034416));
#57178=CARTESIAN_POINT('Ctrl Pts',(15.1518257104396,9.32856897303256,-2.79923279354156));
#57179=CARTESIAN_POINT('Ctrl Pts',(15.8845791715993,9.2156036499786,-3.13372913998994));
#57180=CARTESIAN_POINT('Ctrl Pts',(16.3870096096401,9.12766425587705,-3.3785113296341));
#57181=CARTESIAN_POINT('Ctrl Pts',(17.3639693983226,8.92220955647037,-3.90025233998292));
#57182=CARTESIAN_POINT('Ctrl Pts',(18.0500449337391,8.73620009317483,-4.29999527322685));
#57183=CARTESIAN_POINT('Ctrl Pts',(18.7841974918272,8.5100601990801,-4.71761880736));
#57184=CARTESIAN_POINT('Ctrl Pts',(19.2877316715229,8.33770758255159,-5.01626902913314));
#57185=CARTESIAN_POINT('Ctrl Pts',(20.270830255076,7.94468607642615,-5.63097621657333));
#57186=CARTESIAN_POINT('Ctrl Pts',(20.9685752777043,7.60361048672244,-6.08039129179283));
#57187=CARTESIAN_POINT('Ctrl Pts',(22.6570444653075,6.7053439134869,-7.10435307734314));
#57188=CARTESIAN_POINT('Ctrl Pts',(23.7241254823866,5.94930970418605,-7.73257301523402));
#57189=CARTESIAN_POINT('Ctrl Pts',(24.6950729185821,5.06818763168846,-8.29049117070007));
#57190=CARTESIAN_POINT('Ctrl Pts',(2.09999999999999,12.4900227849924,-0.9));
#57191=CARTESIAN_POINT('Ctrl Pts',(2.73333333333333,12.4900227849924,-0.9));
#57192=CARTESIAN_POINT('Ctrl Pts',(3.36711593286258,12.4900350732685,-0.899923338257865));
#57193=CARTESIAN_POINT('Ctrl Pts',(4.12606108559101,12.4900388828623,-0.899900267382887));
#57194=CARTESIAN_POINT('Ctrl Pts',(4.38492166674737,12.4901766322851,-0.898235423402214));
#57195=CARTESIAN_POINT('Ctrl Pts',(4.89214186044569,12.4907940394702,-0.890880104482316));
#57196=CARTESIAN_POINT('Ctrl Pts',(5.76871669674148,12.4922331404629,-0.873964960821528));
#57197=CARTESIAN_POINT('Ctrl Pts',(6.48935737656207,12.4922496348677,-0.874303891764717));
#57198=CARTESIAN_POINT('Ctrl Pts',(7.01200280711183,12.4897914851075,-0.901601722722426));
#57199=CARTESIAN_POINT('Ctrl Pts',(7.13826357206355,12.4892638554664,-0.908398677788786));
#57200=CARTESIAN_POINT('Ctrl Pts',(7.38673691586477,12.4882832497312,-0.922805797286931));
#57201=CARTESIAN_POINT('Ctrl Pts',(7.69892824648965,12.4871080942582,-0.943038576261421));
#57202=CARTESIAN_POINT('Ctrl Pts',(8.0705664804814,12.4854686042712,-0.971544342930977));
#57203=CARTESIAN_POINT('Ctrl Pts',(8.56088758368331,12.4825959523084,-1.01613710264616));
#57204=CARTESIAN_POINT('Ctrl Pts',(9.15814513041246,12.4769595906258,-1.08610160656213));
#57205=CARTESIAN_POINT('Ctrl Pts',(9.60777554034275,12.468746296037,-1.16049917233183));
#57206=CARTESIAN_POINT('Ctrl Pts',(10.3209062172087,12.4508324485273,-1.30136035149208));
#57207=CARTESIAN_POINT('Ctrl Pts',(11.0425437394732,12.4295262892971,-1.50493234803139));
#57208=CARTESIAN_POINT('Ctrl Pts',(11.9742896318204,12.3853339611956,-1.8399228903873));
#57209=CARTESIAN_POINT('Ctrl Pts',(12.4288761309409,12.3560398614547,-2.01876820477874));
#57210=CARTESIAN_POINT('Ctrl Pts',(12.9286708179861,12.3183165430442,-2.21862458063622));
#57211=CARTESIAN_POINT('Ctrl Pts',(13.4199962589649,12.2751874773222,-2.43712366209172));
#57212=CARTESIAN_POINT('Ctrl Pts',(14.3833021834327,12.1705259624137,-2.9310172387322));
#57213=CARTESIAN_POINT('Ctrl Pts',(15.0609069806317,12.0681822043469,-3.33319508099636));
#57214=CARTESIAN_POINT('Ctrl Pts',(15.7927902555254,11.932649685131,-3.76590395503156));
#57215=CARTESIAN_POINT('Ctrl Pts',(16.2911579735696,11.8276689824143,-4.0808892056978));
#57216=CARTESIAN_POINT('Ctrl Pts',(17.2659787139141,11.5797551229758,-4.75590720934297));
#57217=CARTESIAN_POINT('Ctrl Pts',(17.9510813915698,11.352641285026,-5.27484524120805));
#57218=CARTESIAN_POINT('Ctrl Pts',(18.6848997382068,11.074158593171,-5.81807378002929));
#57219=CARTESIAN_POINT('Ctrl Pts',(19.1880319937622,10.8620643305274,-6.20661118455775));
#57220=CARTESIAN_POINT('Ctrl Pts',(20.172357775901,10.3750481164233,-7.00893220254037));
#57221=CARTESIAN_POINT('Ctrl Pts',(20.8704864843064,9.94949961190826,-7.59709821983438));
#57222=CARTESIAN_POINT('Ctrl Pts',(22.5588413378293,8.82437146010007,-8.93943031422903));
#57223=CARTESIAN_POINT('Ctrl Pts',(23.6292145427077,7.87024728938886,-9.77160798313874));
#57224=CARTESIAN_POINT('Ctrl Pts',(24.6070641578141,6.74729640798646,-10.5188587391465));
#57225=CARTESIAN_POINT('Ctrl Pts',(2.09999999999999,18.0689090073278,-0.9));
#57226=CARTESIAN_POINT('Ctrl Pts',(2.73333333333332,18.0689090073278,-0.9));
#57227=CARTESIAN_POINT('Ctrl Pts',(3.36736559419821,18.0689314789609,-0.899865425636373));
#57228=CARTESIAN_POINT('Ctrl Pts',(4.12659875622228,18.0689384409667,-0.899825122261498));
#57229=CARTESIAN_POINT('Ctrl Pts',(4.38926345438438,18.0690862846866,-0.897386117530702));
#57230=CARTESIAN_POINT('Ctrl Pts',(4.89899520603675,18.069746945452,-0.886685515381575));
#57231=CARTESIAN_POINT('Ctrl Pts',(5.77464038746463,18.071286009881,-0.86222188815569));
#57232=CARTESIAN_POINT('Ctrl Pts',(6.48217933907112,18.0713158624184,-0.862943428769206));
#57233=CARTESIAN_POINT('Ctrl Pts',(6.98941530816473,18.0686994298788,-0.901392822899508));
#57234=CARTESIAN_POINT('Ctrl Pts',(7.11543652137778,18.0681565331617,-0.911206755481794));
#57235=CARTESIAN_POINT('Ctrl Pts',(7.36121956286345,18.0672138729335,-0.93185221447469));
#57236=CARTESIAN_POINT('Ctrl Pts',(7.67024245563845,18.0661849478685,-0.960846457117527));
#57237=CARTESIAN_POINT('Ctrl Pts',(8.03672088388777,18.0647641042642,-1.00158789539943));
#57238=CARTESIAN_POINT('Ctrl Pts',(8.51901276891291,18.0621154200779,-1.06515019836488));
#57239=CARTESIAN_POINT('Ctrl Pts',(9.10353634573336,18.0563613895553,-1.16450313421632));
#57240=CARTESIAN_POINT('Ctrl Pts',(9.53996031439373,18.0471397487516,-1.26934809663657));
#57241=CARTESIAN_POINT('Ctrl Pts',(10.2286868726423,18.0264576771242,-1.4667114867886));
#57242=CARTESIAN_POINT('Ctrl Pts',(10.9322529814026,18.0033848030989,-1.75351833023026));
#57243=CARTESIAN_POINT('Ctrl Pts',(11.8534175309074,17.9519701461305,-2.23291342512525));
#57244=CARTESIAN_POINT('Ctrl Pts',(12.3052433854515,17.9161742014927,-2.49039272798436));
#57245=CARTESIAN_POINT('Ctrl Pts',(12.8031166247441,17.8688536207807,-2.77894324840396));
#57246=CARTESIAN_POINT('Ctrl Pts',(13.2871795523955,17.8155736163136,-3.09023041616086));
#57247=CARTESIAN_POINT('Ctrl Pts',(14.2486094030008,17.6833109363502,-3.80395063248038));
#57248=CARTESIAN_POINT('Ctrl Pts',(14.9265925530568,17.5504089048378,-4.38797919240388));
#57249=CARTESIAN_POINT('Ctrl Pts',(15.6587039975819,17.3701999174313,-5.01739464023764));
#57250=CARTESIAN_POINT('Ctrl Pts',(16.159865983277,17.2304652392218,-5.47692008190156));
#57251=CARTESIAN_POINT('Ctrl Pts',(17.1407994058435,16.8957016774365,-6.46562803933544));
#57252=CARTESIAN_POINT('Ctrl Pts',(17.8296343470588,16.5850049496136,-7.22640249819829));
#57253=CARTESIAN_POINT('Ctrl Pts',(18.56460273973,16.2014274362579,-8.0214716671563));
#57254=CARTESIAN_POINT('Ctrl Pts',(19.0748031274678,15.9062727033236,-8.59692120486745));
#57255=CARTESIAN_POINT('Ctrl Pts',(20.0668883298028,15.2256796563853,-9.78160896677002));
#57256=CARTESIAN_POINT('Ctrl Pts',(20.7688293710982,14.6278203429455,-10.649754812288));
#57257=CARTESIAN_POINT('Ctrl Pts',(22.4601426409202,13.0448722721453,-12.628814335545));
#57258=CARTESIAN_POINT('Ctrl Pts',(23.5475123664675,11.6790030585503,-13.8811542175352));
#57259=CARTESIAN_POINT('Ctrl Pts',(24.5367146907742,10.0590378761085,-15.0082084052888));
#57260=CARTESIAN_POINT('Ctrl Pts',(2.09999999999999,27.8319598964147,-0.9));
#57261=CARTESIAN_POINT('Ctrl Pts',(2.73333333333333,27.8319598964147,-0.9));
#57262=CARTESIAN_POINT('Ctrl Pts',(3.36789044795187,27.8319876241424,-0.89982221409351));
#57263=CARTESIAN_POINT('Ctrl Pts',(4.12765289629168,27.831996167011,-0.89977046921849));
#57264=CARTESIAN_POINT('Ctrl Pts',(4.39698725464062,27.8321607554124,-0.895929159974803));
#57265=CARTESIAN_POINT('Ctrl Pts',(4.91109827079468,27.8328943097031,-0.879282199143232));
#57266=CARTESIAN_POINT('Ctrl Pts',(5.78522928181945,27.8346056768937,-0.84165461313598));
#57267=CARTESIAN_POINT('Ctrl Pts',(6.46973294865984,27.8346392832047,-0.843590781671977));
#57268=CARTESIAN_POINT('Ctrl Pts',(6.95067651024836,27.8317418569026,-0.899765981581546));
#57269=CARTESIAN_POINT('Ctrl Pts',(7.07629429939615,27.8311726695747,-0.914829100774546));
#57270=CARTESIAN_POINT('Ctrl Pts',(7.31750539815411,27.830297898526,-0.946050159135031));
#57271=CARTESIAN_POINT('Ctrl Pts',(7.62122509886065,27.8295244439959,-0.9899356060868));
#57272=CARTESIAN_POINT('Ctrl Pts',(7.97911623757604,27.8284951948722,-1.05124515340815));
#57273=CARTESIAN_POINT('Ctrl Pts',(8.44841085954398,27.8262539604227,-1.14651171885001));
#57274=CARTESIAN_POINT('Ctrl Pts',(9.01306407988194,27.8203481205507,-1.29445151760389));
#57275=CARTESIAN_POINT('Ctrl Pts',(9.43128909448383,27.8094728330774,-1.44915600718223));
#57276=CARTESIAN_POINT('Ctrl Pts',(10.0907382943461,27.7842139649744,-1.73964108221529));
#57277=CARTESIAN_POINT('Ctrl Pts',(10.7834515141013,27.7583882260773,-2.17179722470656));
#57278=CARTESIAN_POINT('Ctrl Pts',(11.7033986544081,27.6943968923929,-2.90904596552635));
#57279=CARTESIAN_POINT('Ctrl Pts',(12.1558218967572,27.647130029751,-3.30641843400165));
#57280=CARTESIAN_POINT('Ctrl Pts',(12.6542280666759,27.582969575709,-3.75198469320058));
#57281=CARTESIAN_POINT('Ctrl Pts',(13.1437548116734,27.5107186176355,-4.23653406986742));
#57282=CARTESIAN_POINT('Ctrl Pts',(14.1171239439967,27.3271714868175,-5.3520099831172));
#57283=CARTESIAN_POINT('Ctrl Pts',(14.8016839612719,27.1377343463863,-6.26369910268171));
#57284=CARTESIAN_POINT('Ctrl Pts',(15.5358005468912,26.8775022985013,-7.24012140721596));
#57285=CARTESIAN_POINT('Ctrl Pts',(16.0483854251272,26.6719324304959,-7.96755301690588));
#57286=CARTESIAN_POINT('Ctrl Pts',(17.0412489733341,26.1774693343013,-9.51866802157106));
#57287=CARTESIAN_POINT('Ctrl Pts',(17.7361882741502,25.7144627748922,-10.708934017746));
#57288=CARTESIAN_POINT('Ctrl Pts',(18.4727311807247,25.1427927030562,-11.9454322770708));
#57289=CARTESIAN_POINT('Ctrl Pts',(18.9926681482578,24.6948244944429,-12.856984892699));
#57290=CARTESIAN_POINT('Ctrl Pts',(19.993215775242,23.6653897614789,-14.7147792886911));
#57291=CARTESIAN_POINT('Ctrl Pts',(20.6988619738766,22.7591841007288,-16.0727729514956));
#57292=CARTESIAN_POINT('Ctrl Pts',(22.3925074251532,20.3625954625553,-19.1600243068367));
#57293=CARTESIAN_POINT('Ctrl Pts',(23.4934455914502,18.2609587529817,-21.14616843884));
#57294=CARTESIAN_POINT('Ctrl Pts',(24.4910863782171,15.7630437648442,-22.9288095711654));
#57295=CARTESIAN_POINT('Ctrl Pts',(2.09999999999999,34.805567674334,-0.9));
#57296=CARTESIAN_POINT('Ctrl Pts',(2.73333333333332,34.805567674334,-0.9));
#57297=CARTESIAN_POINT('Ctrl Pts',(3.36826743871256,34.8055967346523,-0.899835915143074));
#57298=CARTESIAN_POINT('Ctrl Pts',(4.12840588772228,34.8056056335578,-0.899790127261619));
#57299=CARTESIAN_POINT('Ctrl Pts',(4.4025114583892,34.8057820526053,-0.89490507727122));
#57300=CARTESIAN_POINT('Ctrl Pts',(4.91970796594585,34.8065669258982,-0.873924471880327));
#57301=CARTESIAN_POINT('Ctrl Pts',(5.79287353555174,34.8084012267811,-0.826944415738466));
#57302=CARTESIAN_POINT('Ctrl Pts',(6.46062808939426,34.8084327574831,-0.83018802637527));
#57303=CARTESIAN_POINT('Ctrl Pts',(6.92359088308148,34.8053357383561,-0.897514817877851));
#57304=CARTESIAN_POINT('Ctrl Pts',(7.04893740326678,34.804748375931,-0.916302103864695));
#57305=CARTESIAN_POINT('Ctrl Pts',(7.28704977969169,34.8039238169991,-0.954792702397151));
#57306=CARTESIAN_POINT('Ctrl Pts',(7.58724291600503,34.8033356004416,-1.00895581405421));
#57307=CARTESIAN_POINT('Ctrl Pts',(7.93954383598411,34.8025940050698,-1.08429063224267));
#57308=CARTESIAN_POINT('Ctrl Pts',(8.40075586732036,34.8006611522329,-1.20110613516639));
#57309=CARTESIAN_POINT('Ctrl Pts',(8.95399273182333,34.7946914626677,-1.38186135819649));
#57310=CARTESIAN_POINT('Ctrl Pts',(9.36427840538061,34.7827044460818,-1.57081212048793));
#57311=CARTESIAN_POINT('Ctrl Pts',(10.0148313303383,34.7542662135578,-1.92761296467034));
#57312=CARTESIAN_POINT('Ctrl Pts',(10.7126997709799,34.7263529856802,-2.47021587913641));
#57313=CARTESIAN_POINT('Ctrl Pts',(11.6386950163915,34.6527282846468,-3.39910531888624));
#57314=CARTESIAN_POINT('Ctrl Pts',(12.0933422150127,34.5969186241691,-3.89880693180439));
#57315=CARTESIAN_POINT('Ctrl Pts',(12.5933047205618,34.5203928739712,-4.45827819796938));
#57316=CARTESIAN_POINT('Ctrl Pts',(13.0908921604143,34.4332799259541,-5.07548512276185));
#57317=CARTESIAN_POINT('Ctrl Pts',(14.0727432149392,34.210693104137,-6.48656916810702));
#57318=CARTESIAN_POINT('Ctrl Pts',(14.7612503503968,33.9790719957191,-7.63560214898364));
#57319=CARTESIAN_POINT('Ctrl Pts',(15.4965030323713,33.6603033480339,-8.8605088817018));
#57320=CARTESIAN_POINT('Ctrl Pts',(16.014881454427,33.4054890971074,-9.78386054397124));
#57321=CARTESIAN_POINT('Ctrl Pts',(17.0125123260485,32.7936491966452,-11.7388593147722));
#57322=CARTESIAN_POINT('Ctrl Pts',(17.7100146172093,32.2196145267863,-13.2363029872184));
#57323=CARTESIAN_POINT('Ctrl Pts',(18.4472695543676,31.5115805969217,-14.7874452578874));
#57324=CARTESIAN_POINT('Ctrl Pts',(18.9707548965599,30.9524459159778,-15.9395047263215));
#57325=CARTESIAN_POINT('Ctrl Pts',(19.9740264837229,29.6706590049061,-18.2765031600774));
#57326=CARTESIAN_POINT('Ctrl Pts',(20.6810539289866,28.54203233395,-19.9829624932166));
#57327=CARTESIAN_POINT('Ctrl Pts',(22.3757767447239,25.5592752325617,-23.8579947070288));
#57328=CARTESIAN_POINT('Ctrl Pts',(23.4815899075194,22.9294129237493,-26.364359275229));
#57329=CARTESIAN_POINT('Ctrl Pts',(24.4815088739376,19.8034651938544,-28.6101490004946));
#57330=CARTESIAN_POINT('Ctrl Pts',(2.09999999999999,38.9897323410855,-0.9));
#57331=CARTESIAN_POINT('Ctrl Pts',(2.73333333333332,38.9897323410855,-0.9));
#57332=CARTESIAN_POINT('Ctrl Pts',(3.36849615379698,38.9897610649469,-0.899852059213593));
#57333=CARTESIAN_POINT('Ctrl Pts',(4.12885962395895,38.9897698170468,-0.899812187521165));
#57334=CARTESIAN_POINT('Ctrl Pts',(4.40583159898798,38.9899532662553,-0.894285767756435));
#57335=CARTESIAN_POINT('Ctrl Pts',(4.92485788889799,38.990768611501,-0.870670475322903));
#57336=CARTESIAN_POINT('Ctrl Pts',(5.79750326314279,38.9926765482163,-0.818103220835964));
#57337=CARTESIAN_POINT('Ctrl Pts',(6.45506243282504,38.992704760601,-0.822251386235662));
#57338=CARTESIAN_POINT('Ctrl Pts',(6.90763991463113,38.9894881916481,-0.895788682720272));
#57339=CARTESIAN_POINT('Ctrl Pts',(7.03283207401276,38.9888901159876,-0.91680271827912));
#57340=CARTESIAN_POINT('Ctrl Pts',(7.26916860321449,38.9880962384994,-0.959567402413746));
#57341=CARTESIAN_POINT('Ctrl Pts',(7.56737377775836,38.987619882036,-1.01979141838418));
#57342=CARTESIAN_POINT('Ctrl Pts',(7.91658095958571,38.9870532799917,-1.10336261682834));
#57343=CARTESIAN_POINT('Ctrl Pts',(8.37348791722709,38.9853096166242,-1.23286279651375));
#57344=CARTESIAN_POINT('Ctrl Pts',(8.92106444762905,38.9793115853919,-1.43302666782297));
#57345=CARTESIAN_POINT('Ctrl Pts',(9.32831366869251,38.9666594263059,-1.64284783605233));
#57346=CARTESIAN_POINT('Ctrl Pts',(9.97666156258205,38.936276009937,-2.04106314828367));
#57347=CARTESIAN_POINT('Ctrl Pts',(10.6788383765048,38.9069541794025,-2.65284302971923));
#57348=CARTESIAN_POINT('Ctrl Pts',(11.6082277531202,38.8272954085081,-3.69828340078152));
#57349=CARTESIAN_POINT('Ctrl Pts',(12.0641250472752,38.7662333808051,-4.25984491669686));
#57350=CARTESIAN_POINT('Ctrl Pts',(12.5649316129707,38.6821599570872,-4.88795818367918));
#57351=CARTESIAN_POINT('Ctrl Pts',(13.0665677015588,38.5858647600716,-5.58586750635022));
#57352=CARTESIAN_POINT('Ctrl Pts',(14.0523411482935,38.3394863474703,-7.17457852304705));
#57353=CARTESIAN_POINT('Ctrl Pts',(14.7427818946082,38.0822528719035,-8.4661717831259));
#57354=CARTESIAN_POINT('Ctrl Pts',(15.4785956174119,37.7280642874556,-9.84020415159883));
#57355=CARTESIAN_POINT('Ctrl Pts',(15.9996744207587,37.4434946991277,-10.8810259511239));
#57356=CARTESIAN_POINT('Ctrl Pts',(16.9995248066819,36.7608899240757,-13.0779693240867));
#57357=CARTESIAN_POINT('Ctrl Pts',(17.698187626898,36.1199220991796,-14.7595819219367));
#57358=CARTESIAN_POINT('Ctrl Pts',(18.4357383815742,35.3297290385984,-16.4993988315544));
#57359=CARTESIAN_POINT('Ctrl Pts',(18.9608457759147,34.7037521257359,-17.795429156587));
#57360=CARTESIAN_POINT('Ctrl Pts',(19.9653654503623,33.2702491455335,-20.4194610099597));
#57361=CARTESIAN_POINT('Ctrl Pts',(20.6729596776041,32.0078971340288,-22.3346914855994));
#57362=CARTESIAN_POINT('Ctrl Pts',(22.3680456304984,28.6727183627523,-26.6817849852975));
#57363=CARTESIAN_POINT('Ctrl Pts',(23.4757593035169,25.7258503646778,-29.4992019611683));
#57364=CARTESIAN_POINT('Ctrl Pts',(24.4767076204831,22.2231379796722,-32.0221667171178));
#57365=CARTESIAN_POINT('Ctrl Pts',(2.79759256767181,38.5299267367737,-0.89995268342482));
#57366=CARTESIAN_POINT('Ctrl Pts',(2.93204017151055,38.2166454242421,-0.899936609237971));
#57367=CARTESIAN_POINT('Ctrl Pts',(3.06669302905926,37.9029839075505,-0.899917784182059));
#57368=CARTESIAN_POINT('Ctrl Pts',(3.20139918604663,37.5892463829854,-0.899898741184433));
#57369=CARTESIAN_POINT('Origin',(0.249999999999999,0.,0.));
#57370=CARTESIAN_POINT('',(0.249999999999999,-38.75,-4.74550634669599E-15));
#57371=CARTESIAN_POINT('Origin',(2.9,0.,0.));
#57372=CARTESIAN_POINT('Origin',(27.1,0.,0.));
#57373=CARTESIAN_POINT('',(27.2,-8.7,-1.0654427152582E-15));
#57374=CARTESIAN_POINT('Origin',(27.2,0.,0.));
#57375=CARTESIAN_POINT('',(27.1,-8.95,-1.09605888523688E-15));
#57376=CARTESIAN_POINT('Origin',(28.8,0.,0.));
#57377=CARTESIAN_POINT('',(30.4,-8.7,-1.0654427152582E-15));
#57378=CARTESIAN_POINT('Origin',(30.4,0.,0.));
#57379=CARTESIAN_POINT('',(28.8,-8.7,-1.0654427152582E-15));
#57380=CARTESIAN_POINT('Origin',(30.7,0.,0.));
#57381=CARTESIAN_POINT('',(30.7,-8.4,-1.02870331128378E-15));
#57382=CARTESIAN_POINT('',(0.,0.,0.));
#57383=CARTESIAN_POINT('Origin',(1.5,4.65899107620574,2.68986975199944));
#57384=CARTESIAN_POINT('',(6.68133955674308,4.65899107620048,2.68986975199644));
#57385=CARTESIAN_POINT('',(6.4964847157299,4.78249346839053,2.47595733387918));
#57386=CARTESIAN_POINT('Ctrl Pts',(6.68133955674087,4.65899107619594,2.6898697519957));
#57387=CARTESIAN_POINT('Ctrl Pts',(6.67492308098284,4.66333926734057,2.68233846075464));
#57388=CARTESIAN_POINT('Ctrl Pts',(6.6685005684247,4.6676851311398,2.67481117074313));
#57389=CARTESIAN_POINT('Ctrl Pts',(6.6620720344556,4.67202864152121,2.66728791952006));
#57390=CARTESIAN_POINT('Ctrl Pts',(6.6073292890925,4.70901618548297,2.60322301327753));
#57391=CARTESIAN_POINT('Ctrl Pts',(6.55213434648286,4.74584349646411,2.53943317427317));
#57392=CARTESIAN_POINT('Ctrl Pts',(6.49649612060902,4.78249290359719,2.47595028107013));
#57393=CARTESIAN_POINT('',(1.6,4.78249346839052,2.4759573338791));
#57394=CARTESIAN_POINT('',(1.5,4.78249346839052,2.4759573338791));
#57395=CARTESIAN_POINT('',(1.6,4.53548868402095,2.90378217011979));
#57396=CARTESIAN_POINT('',(1.6,5.10274107620574,1.92127220614075));
#57397=CARTESIAN_POINT('',(6.49648471573067,4.53548868402103,2.90378217011975));
#57398=CARTESIAN_POINT('',(1.5,4.53548868402095,2.90378217011979));
#57399=CARTESIAN_POINT('Ctrl Pts',(6.49648471573075,4.53548868402095,2.90378217011979));
#57400=CARTESIAN_POINT('Ctrl Pts',(6.55337396234634,4.57295850701816,2.83888253293802));
#57401=CARTESIAN_POINT('Ctrl Pts',(6.60979834671122,4.61061413969367,2.77366106395288));
#57402=CARTESIAN_POINT('Ctrl Pts',(6.67094806990306,4.65195340556208,2.70205935512119));
#57403=CARTESIAN_POINT('Ctrl Pts',(6.67614580655144,4.65547147830345,2.69596587438841));
#57404=CARTESIAN_POINT('Ctrl Pts',(6.68133955672778,4.65899107621137,2.68986975198969));
#57405=CARTESIAN_POINT('Origin',(1.5,4.68474025750198,1.25527236874723));
#57406=CARTESIAN_POINT('',(6.9730266888256,4.68474025754297,1.25527236925909));
#57407=CARTESIAN_POINT('Ctrl Pts',(6.97303770557678,4.68473984672734,1.25526723923358));
#57408=CARTESIAN_POINT('Ctrl Pts',(6.85768162673857,4.71538888116549,1.63799446828719));
#57409=CARTESIAN_POINT('Ctrl Pts',(6.70189613372097,4.74746137538506,2.03849703114157));
#57410=CARTESIAN_POINT('Ctrl Pts',(6.49649612060898,4.7824929035972,2.47595028107023));
#57411=CARTESIAN_POINT('',(1.6,4.68474025750198,1.25527236874723));
#57412=CARTESIAN_POINT('',(1.5,4.68474025750198,1.25527236874723));
#57413=CARTESIAN_POINT('',(1.6,4.63118372339748,0.586489672284435));
#57414=CARTESIAN_POINT('Ctrl Pts',(6.45213506683142,4.78997609487978,2.5693960002115));
#57415=CARTESIAN_POINT('Ctrl Pts',(6.69496761877087,4.74945078078581,2.06333956306629));
#57416=CARTESIAN_POINT('Ctrl Pts',(6.87214261929782,4.7129326345547,1.60732229617945));
#57417=CARTESIAN_POINT('Ctrl Pts',(6.99737260418699,4.67812918220736,1.17271712435015));
#57418=CARTESIAN_POINT('Ctrl Pts',(6.59045151583296,4.71093147065315,2.6420974655224));
#57419=CARTESIAN_POINT('Ctrl Pts',(6.83894619948317,4.67186091612313,2.13090865278462));
#57420=CARTESIAN_POINT('Ctrl Pts',(7.02199092230211,4.63669438947174,1.6676886040292));
#57421=CARTESIAN_POINT('Ctrl Pts',(7.15213252925719,4.60270344939976,1.22335080384112));
#57422=CARTESIAN_POINT('Ctrl Pts',(6.7287679648345,4.63188684642653,2.7147989308333));
#57423=CARTESIAN_POINT('Ctrl Pts',(6.98292478019547,4.59427105146045,2.19847774250294));
#57424=CARTESIAN_POINT('Ctrl Pts',(7.17183922530641,4.56045614438878,1.72805491187896));
#57425=CARTESIAN_POINT('Ctrl Pts',(7.30689245432738,4.52727771659216,1.27398448333209));
#57426=CARTESIAN_POINT('Ctrl Pts',(6.86708441383604,4.5528422221999,2.7875003961442));
#57427=CARTESIAN_POINT('Ctrl Pts',(7.12690336090777,4.51668118679778,2.26604683222127));
#57428=CARTESIAN_POINT('Ctrl Pts',(7.32168752831071,4.48421789930582,1.78842121972871));
#57429=CARTESIAN_POINT('Ctrl Pts',(7.46165237939758,4.45185198378456,1.32461816282306));
#57430=CARTESIAN_POINT('',(6.94805436450009,4.54138228956796,2.62196828737462));
#57431=CARTESIAN_POINT('Ctrl Pts',(6.94805436450009,4.54138228956796,2.62196828737462));
#57432=CARTESIAN_POINT('Ctrl Pts',(6.85888718065088,4.58048619487533,2.64454493763046));
#57433=CARTESIAN_POINT('Ctrl Pts',(6.7680729844652,4.62053162275365,2.66766517619599));
#57434=CARTESIAN_POINT('Ctrl Pts',(6.68133955674308,4.65899107619524,2.68986975199342));
#57435=CARTESIAN_POINT('',(7.46165237939758,4.45185198378456,1.32461816282306));
#57436=CARTESIAN_POINT('Ctrl Pts',(6.94809164225473,4.54138208596012,2.62194359089516));
#57437=CARTESIAN_POINT('Ctrl Pts',(7.16787076968256,4.50975040784356,2.16421694982278));
#57438=CARTESIAN_POINT('Ctrl Pts',(7.33663088231394,4.4807623507912,1.73890326423272));
#57439=CARTESIAN_POINT('Ctrl Pts',(7.46165237939758,4.45185198378456,1.32461816282306));
#57440=CARTESIAN_POINT('',(7.17384635845297,4.59212072600797,1.23045504008007));
#57441=CARTESIAN_POINT('Ctrl Pts',(7.46165237939758,4.45185198378456,1.32461816282306));
#57442=CARTESIAN_POINT('Ctrl Pts',(7.36571703908271,4.49860823119237,1.29323045524206));
#57443=CARTESIAN_POINT('Ctrl Pts',(7.26978169876784,4.54536447860017,1.26184274766107));
#57444=CARTESIAN_POINT('Ctrl Pts',(7.17384635845297,4.59212072600797,1.23045504008007));
#57445=CARTESIAN_POINT('Ctrl Pts',(7.17384635845264,4.59212072600813,1.23045504008011));
#57446=CARTESIAN_POINT('Ctrl Pts',(7.10373004606762,4.62436150671956,1.23909393123514));
#57447=CARTESIAN_POINT('Ctrl Pts',(7.04027818843215,4.65362469478555,1.24693497884549));
#57448=CARTESIAN_POINT('Ctrl Pts',(6.97302668796278,4.68474025804403,1.25527236889283));
#57449=CARTESIAN_POINT('Origin',(1.5,2.68986975199945,4.65899107620574));
#57450=CARTESIAN_POINT('',(6.68133955674308,2.6898697519964,4.65899107620051));
#57451=CARTESIAN_POINT('',(6.4964847157299,2.90378217011975,4.53548868402103));
#57452=CARTESIAN_POINT('Ctrl Pts',(6.68133955674087,2.68986975199284,4.65899107619759));
#57453=CARTESIAN_POINT('Ctrl Pts',(6.67492308098284,2.69740104160513,4.65464288223185));
#57454=CARTESIAN_POINT('Ctrl Pts',(6.6685005684247,2.7049283150624,4.65029698975985));
#57455=CARTESIAN_POINT('Ctrl Pts',(6.6620720344556,2.71245153100584,4.64595341827232));
#57456=CARTESIAN_POINT('Ctrl Pts',(6.60732928909252,2.77651613682155,4.60896535395611));
#57457=CARTESIAN_POINT('Ctrl Pts',(6.55213434648287,2.84030444318649,4.57213538836559));
#57458=CARTESIAN_POINT('Ctrl Pts',(6.49649612060902,2.9037852073989,4.53548229371255));
#57459=CARTESIAN_POINT('',(1.6,2.90378217011979,4.53548868402095));
#57460=CARTESIAN_POINT('',(1.5,2.90378217011979,4.53548868402095));
#57461=CARTESIAN_POINT('',(1.6,2.4759573338791,4.78249346839052));
#57462=CARTESIAN_POINT('',(1.6,4.02111975199945,3.89039353034704));
#57463=CARTESIAN_POINT('',(6.49648471573067,2.47595733387918,4.78249346839053));
#57464=CARTESIAN_POINT('',(1.5,2.4759573338791,4.78249346839052));
#57465=CARTESIAN_POINT('Ctrl Pts',(6.49648471573075,2.4759573338791,4.78249346839052));
#57466=CARTESIAN_POINT('Ctrl Pts',(6.55337396234642,2.54085697106096,4.74502364539326));
#57467=CARTESIAN_POINT('Ctrl Pts',(6.60979834671138,2.6060784400462,4.7073680127177));
#57468=CARTESIAN_POINT('Ctrl Pts',(6.67094806990306,2.67768014887771,4.66602874684939));
#57469=CARTESIAN_POINT('Ctrl Pts',(6.67614580655144,2.68377362961048,4.66251067410802));
#57470=CARTESIAN_POINT('Ctrl Pts',(6.68133955672777,2.6898697520092,4.6589910762001));
#57471=CARTESIAN_POINT('Origin',(1.5,3.42946788875476,3.42946788875476));
#57472=CARTESIAN_POINT('',(6.9730266888256,3.42946788853432,3.42946788921854));
#57473=CARTESIAN_POINT('Ctrl Pts',(6.97303770557678,3.4294700977703,3.42946324107831));
#57474=CARTESIAN_POINT('Ctrl Pts',(6.85768162673857,3.26464932566841,3.77623926137783));
#57475=CARTESIAN_POINT('Ctrl Pts',(6.70189613372098,3.09217363899809,4.13912090220029));
#57476=CARTESIAN_POINT('Ctrl Pts',(6.49649612060898,2.90378520739886,4.53548229371264));
#57477=CARTESIAN_POINT('',(1.6,3.42946788875476,3.42946788875476));
#57478=CARTESIAN_POINT('',(1.5,3.42946788875476,3.42946788875476));
#57479=CARTESIAN_POINT('',(1.6,4.10539157077492,2.00735269363697));
#57480=CARTESIAN_POINT('Ctrl Pts',(6.45213506683141,2.86354298158031,4.62015025600519));
#57481=CARTESIAN_POINT('Ctrl Pts',(6.69496761877087,3.08147524865119,4.16162986864181));
#57482=CARTESIAN_POINT('Ctrl Pts',(6.87214261929781,3.27785823975936,3.74844825783789));
#57483=CARTESIAN_POINT('Ctrl Pts',(6.99737260418699,3.46502015180182,3.35466741224394));
#57484=CARTESIAN_POINT('Ctrl Pts',(6.59045151583295,2.758737596312,4.64358925974348));
#57485=CARTESIAN_POINT('Ctrl Pts',(6.83894619948317,2.98049590991795,4.18135148451713));
#57486=CARTESIAN_POINT('Ctrl Pts',(7.02199092230211,3.1816508288527,3.76260789142697));
#57487=CARTESIAN_POINT('Ctrl Pts',(7.15213252925719,3.37438271134589,3.3608045985664));
#57488=CARTESIAN_POINT('Ctrl Pts',(6.72876796483449,2.6539322110437,4.66702826348176));
#57489=CARTESIAN_POINT('Ctrl Pts',(6.98292478019547,2.87951657118472,4.20107310039245));
#57490=CARTESIAN_POINT('Ctrl Pts',(7.17183922530641,3.08544341794604,3.77676752501605));
#57491=CARTESIAN_POINT('Ctrl Pts',(7.30689245432738,3.28374527088997,3.36694178488886));
#57492=CARTESIAN_POINT('Ctrl Pts',(6.86708441383603,2.54912682577539,4.69046726722004));
#57493=CARTESIAN_POINT('Ctrl Pts',(7.12690336090777,2.77853723245148,4.22079471626778));
#57494=CARTESIAN_POINT('Ctrl Pts',(7.3216875283107,2.98923600703937,3.79092715860513));
#57495=CARTESIAN_POINT('Ctrl Pts',(7.46165237939758,3.19310783043405,3.37307897121132));
#57496=CARTESIAN_POINT('',(6.94805436450009,2.62196828737528,4.54138228956758));
#57497=CARTESIAN_POINT('Ctrl Pts',(6.94805436450009,2.62196828737528,4.54138228956758));
#57498=CARTESIAN_POINT('Ctrl Pts',(6.85888711552653,2.64454495411986,4.58048622343519));
#57499=CARTESIAN_POINT('Ctrl Pts',(6.76807293638612,2.6676651885047,4.62053164407293));
#57500=CARTESIAN_POINT('Ctrl Pts',(6.68133955674307,2.68986975199337,4.65899107619527));
#57501=CARTESIAN_POINT('',(7.46165237939758,3.19310783043405,3.37307897121132));
#57502=CARTESIAN_POINT('Ctrl Pts',(6.94809164225473,2.62198045928545,4.54136079998506));
#57503=CARTESIAN_POINT('Ctrl Pts',(7.16787076968256,2.82344994300837,4.12914206176917));
#57504=CARTESIAN_POINT('Ctrl Pts',(7.33663088231394,3.0110023919897,3.74631557694482));
#57505=CARTESIAN_POINT('Ctrl Pts',(7.46165237939758,3.19310783043405,3.37307897121132));
#57506=CARTESIAN_POINT('',(7.17384635845298,3.3616656859279,3.36166568592793));
#57507=CARTESIAN_POINT('Ctrl Pts',(7.46165237939758,3.19310783043405,3.37307897121132));
#57508=CARTESIAN_POINT('Ctrl Pts',(7.36571703908271,3.24929378226533,3.36927454278352));
#57509=CARTESIAN_POINT('Ctrl Pts',(7.26978169876785,3.30547973409662,3.36547011435573));
#57510=CARTESIAN_POINT('Ctrl Pts',(7.17384635845298,3.3616656859279,3.36166568592793));
#57511=CARTESIAN_POINT('Ctrl Pts',(7.17384635845271,3.361665685928,3.36166568592802));
#57512=CARTESIAN_POINT('Ctrl Pts',(7.10380439458403,3.38524254899043,3.38524254899052));
#57513=CARTESIAN_POINT('Ctrl Pts',(7.04024193630147,3.40670199458556,3.4067019945858));
#57514=CARTESIAN_POINT('Ctrl Pts',(6.9730266882762,3.42946788904522,3.42946788904572));
#57515=CARTESIAN_POINT('Origin',(1.5,2.60208521396521E-16,5.37973950399889));
#57516=CARTESIAN_POINT('',(6.68133955674308,-2.66020618484513E-14,5.37973950399284));
#57517=CARTESIAN_POINT('',(6.4964847157299,0.2470047843695,5.37973950399894));
#57518=CARTESIAN_POINT('Ctrl Pts',(6.68133955674087,-1.6530180002583E-12,
5.37973950398853));
#57519=CARTESIAN_POINT('Ctrl Pts',(6.67492308098284,0.00869638510872298,
5.37973950235977));
#57520=CARTESIAN_POINT('Ctrl Pts',(6.6685005684247,0.0173881413799499,5.37973948580553));
#57521=CARTESIAN_POINT('Ctrl Pts',(6.6620720344556,0.0260752232488897,5.3797394505259));
#57522=CARTESIAN_POINT('Ctrl Pts',(6.60732928909258,0.100050831526762,5.37973915009911));
#57523=CARTESIAN_POINT('Ctrl Pts',(6.5521343464829,0.173708108098482,5.37973761745967));
#57524=CARTESIAN_POINT('Ctrl Pts',(6.49649612060902,0.247010609884639,5.37973548846904));
#57525=CARTESIAN_POINT('',(1.6,0.247004784369567,5.37973950399889));
#57526=CARTESIAN_POINT('',(1.5,0.247004784369567,5.37973950399889));
#57527=CARTESIAN_POINT('',(1.6,-0.247004784369566,5.37973950399889));
#57528=CARTESIAN_POINT('',(1.6,1.775,5.37973950399889));
#57529=CARTESIAN_POINT('',(6.49648471573025,-0.247004784369127,5.37973950399919));
#57530=CARTESIAN_POINT('',(1.5,-0.247004784369566,5.37973950399889));
#57531=CARTESIAN_POINT('Ctrl Pts',(6.49648471573075,-0.247004784369566,
5.37973950399889));
#57532=CARTESIAN_POINT('Ctrl Pts',(6.5534522954077,-0.171961951002559,5.37973950399889));
#57533=CARTESIAN_POINT('Ctrl Pts',(6.60995374323598,-0.0965464591095595,
5.37973950399889));
#57534=CARTESIAN_POINT('Ctrl Pts',(6.67110204921906,-0.013866898540887,
5.37973950399889));
#57535=CARTESIAN_POINT('Ctrl Pts',(6.67622273755884,-0.00693492963715604,
5.37973950399889));
#57536=CARTESIAN_POINT('Ctrl Pts',(6.68133955672777,1.12630738069441E-11,
5.37973950399889));
#57537=CARTESIAN_POINT('Origin',(1.5,1.25527236874723,4.68474025750198));
#57538=CARTESIAN_POINT('',(6.9730266888256,1.25527236832443,4.68474025779341));
#57539=CARTESIAN_POINT('Ctrl Pts',(6.97303770557678,1.25527660564903,4.68473733700388));
#57540=CARTESIAN_POINT('Ctrl Pts',(6.85768162673857,0.93914961978766,4.90264379395559));
#57541=CARTESIAN_POINT('Ctrl Pts',(6.70189613372097,0.608340473184774,5.13067067013966));
#57542=CARTESIAN_POINT('Ctrl Pts',(6.49649612060898,0.247010609884559,5.37973548846909));
#57543=CARTESIAN_POINT('',(1.6,1.25527236874723,4.68474025750198));
#57544=CARTESIAN_POINT('',(1.5,1.25527236874723,4.68474025750198));
#57545=CARTESIAN_POINT('',(1.6,3.12761653072357,3.39413268276809));
#57546=CARTESIAN_POINT('Ctrl Pts',(6.45213506683129,0.169825838874388,5.43293898179196));
#57547=CARTESIAN_POINT('Ctrl Pts',(6.69496761877081,0.587820912143886,5.14481481171758));
#57548=CARTESIAN_POINT('Ctrl Pts',(6.87214261929779,0.964484376716749,4.88518053593885));
#57549=CARTESIAN_POINT('Ctrl Pts',(6.99737260418699,1.32346176996342,4.63773727615197));
#57550=CARTESIAN_POINT('Ctrl Pts',(6.59045151583283,0.0673422109094778,
5.40083506183456));
#57551=CARTESIAN_POINT('Ctrl Pts',(6.83894619948311,0.490509431605883,5.11140456270267));
#57552=CARTESIAN_POINT('Ctrl Pts',(7.02199092230209,0.874086498044711,4.84933943288195));
#57553=CARTESIAN_POINT('Ctrl Pts',(7.15213252925719,1.24189885083336,4.59773351518701));
#57554=CARTESIAN_POINT('Ctrl Pts',(6.72876796483437,-0.0351414170554326,
5.36873114187716));
#57555=CARTESIAN_POINT('Ctrl Pts',(6.98292478019541,0.39319795106788,5.07799431368776));
#57556=CARTESIAN_POINT('Ctrl Pts',(7.17183922530639,0.783688619372672,4.81349832982504));
#57557=CARTESIAN_POINT('Ctrl Pts',(7.30689245432738,1.1603359317033,4.55772975422206));
#57558=CARTESIAN_POINT('Ctrl Pts',(6.86708441383591,-0.137625045020343,
5.33662722191976));
#57559=CARTESIAN_POINT('Ctrl Pts',(7.12690336090771,0.295886470529877,5.04458406467285));
#57560=CARTESIAN_POINT('Ctrl Pts',(7.32168752831068,0.693290740700634,4.77765722676813));
#57561=CARTESIAN_POINT('Ctrl Pts',(7.46165237939758,1.07877301257324,4.51772599325711));
#57562=CARTESIAN_POINT('',(6.94805436450009,3.7775338412871E-13,5.2439365747499));
#57563=CARTESIAN_POINT('Ctrl Pts',(6.94805436450009,3.78588122203372E-13,
5.2439365747499));
#57564=CARTESIAN_POINT('Ctrl Pts',(6.85888652980283,1.57378817050387E-13,
5.28909020484362));
#57565=CARTESIAN_POINT('Ctrl Pts',(6.76807250396889,2.03924805264334E-15,
5.33533059841517));
#57566=CARTESIAN_POINT('Ctrl Pts',(6.68133955674308,-2.8570895649338E-14,
5.37973950398679));
#57567=CARTESIAN_POINT('',(7.46165237939758,1.07877301257324,4.51772599325711));
#57568=CARTESIAN_POINT('Ctrl Pts',(6.94809164225473,2.12859750591682E-5,
5.24392405018061));
#57569=CARTESIAN_POINT('Ctrl Pts',(7.16787076968256,0.380608346074387,4.98766689283114));
#57570=CARTESIAN_POINT('Ctrl Pts',(7.33663088231394,0.734446773846381,4.74990565622242));
#57571=CARTESIAN_POINT('Ctrl Pts',(7.46165237939758,1.07877301257324,4.51772599325711));
#57572=CARTESIAN_POINT('',(7.17384635845298,1.23045504008004,4.59212072600798));
#57573=CARTESIAN_POINT('Ctrl Pts',(7.46165237939758,1.07877301257324,4.51772599325711));
#57574=CARTESIAN_POINT('Ctrl Pts',(7.36571703908271,1.12933368840884,4.5425242375074));
#57575=CARTESIAN_POINT('Ctrl Pts',(7.26978169876785,1.17989436424444,4.56732248175769));
#57576=CARTESIAN_POINT('Ctrl Pts',(7.17384635845298,1.23045504008004,4.59212072600798));
#57577=CARTESIAN_POINT('Ctrl Pts',(7.17384635845272,1.23045504008007,4.5921207260081));
#57578=CARTESIAN_POINT('Ctrl Pts',(7.10380410095029,1.23908480708047,4.62432745491123));
#57579=CARTESIAN_POINT('Ctrl Pts',(7.04024207626729,1.24693945578929,4.65364140296857));
#57580=CARTESIAN_POINT('Ctrl Pts',(6.9730266882762,1.2552723688533,4.6847402578992));
#57581=CARTESIAN_POINT('Origin',(1.5,-2.68986975199944,4.65899107620574));
#57582=CARTESIAN_POINT('',(6.82679400487526,-2.90378217011979,4.53548868402095));
#57583=CARTESIAN_POINT('',(6.82679400487407,-2.4759573338791,4.78249346839052));
#57584=CARTESIAN_POINT('Ctrl Pts',(6.82679400487526,-2.90378217011979,4.53548868402095));
#57585=CARTESIAN_POINT('Ctrl Pts',(6.83650459025506,-2.68986975199908,4.65899107620594));
#57586=CARTESIAN_POINT('Ctrl Pts',(6.82679400487407,-2.4759573338791,4.78249346839052));
#57587=CARTESIAN_POINT('',(1.6,-2.4759573338791,4.78249346839052));
#57588=CARTESIAN_POINT('',(1.5,-2.4759573338791,4.78249346839052));
#57589=CARTESIAN_POINT('',(1.6,-2.90378217011979,4.53548868402095));
#57590=CARTESIAN_POINT('',(1.6,-1.35861975199944,5.42758862206442));
#57591=CARTESIAN_POINT('',(1.5,-2.90378217011979,4.53548868402095));
#57592=CARTESIAN_POINT('Origin',(1.5,-1.25527236874723,4.68474025750198));
#57593=CARTESIAN_POINT('',(7.28571428571429,-1.25527236874723,4.68474025750198));
#57594=CARTESIAN_POINT('Ctrl Pts',(6.82679400487407,-2.4759573338791,4.78249346839052));
#57595=CARTESIAN_POINT('Ctrl Pts',(7.11904573622593,-1.83368826213753,4.7310601618368));
#57596=CARTESIAN_POINT('Ctrl Pts',(7.28571428571429,-1.25527236874723,4.68474025750198));
#57597=CARTESIAN_POINT('',(7.38335469474708,-0.875998372174533,4.65436776006772));
#57598=CARTESIAN_POINT('Ctrl Pts',(7.28571428571429,-1.25527236874723,4.68474025750198));
#57599=CARTESIAN_POINT('Ctrl Pts',(7.34100687338275,-1.06338186755404,4.6693735468711));
#57600=CARTESIAN_POINT('Ctrl Pts',(7.38335469474708,-0.875998372174533,
4.65436776006772));
#57601=CARTESIAN_POINT('',(6.97302668913468,-1.25527236874723,4.68474025750198));
#57602=CARTESIAN_POINT('Ctrl Pts',(7.38335469474708,-0.875998372174534,
4.65436776006772));
#57603=CARTESIAN_POINT('Ctrl Pts',(7.3156799620785,-0.939686273403086,4.65946792679188));
#57604=CARTESIAN_POINT('Ctrl Pts',(7.24771026860098,-1.00309430560521,4.6645456814304));
#57605=CARTESIAN_POINT('Ctrl Pts',(7.1109529188272,-1.12952063537562,4.67466998051569));
#57606=CARTESIAN_POINT('Ctrl Pts',(7.04212976986549,-1.19256708728131,4.6797187795793));
#57607=CARTESIAN_POINT('Ctrl Pts',(6.97302668913468,-1.25527236874723,4.68474025750198));
#57608=CARTESIAN_POINT('',(1.6,-1.25527236874723,4.68474025750198));
#57609=CARTESIAN_POINT('',(1.5,-1.25527236874723,4.68474025750198));
#57610=CARTESIAN_POINT('',(1.6,1.31843731356659,4.47863598610718));
#57611=CARTESIAN_POINT('Origin',(6.9,0.,0.));
#57612=CARTESIAN_POINT('',(7.28571428571429,-3.42946788875475,3.42946788875476));
#57613=CARTESIAN_POINT('Ctrl Pts',(7.28571428571429,-3.42946788875475,3.42946788875476));
#57614=CARTESIAN_POINT('Ctrl Pts',(7.11904573622629,-3.18037415591191,3.95355069855613));
#57615=CARTESIAN_POINT('Ctrl Pts',(6.82679400487526,-2.90378217011979,4.53548868402095));
#57616=CARTESIAN_POINT('',(6.82679400487407,-4.53548868402095,2.90378217011979));
#57617=CARTESIAN_POINT('Ctrl Pts',(6.82679400487407,-4.53548868402095,2.90378217011979));
#57618=CARTESIAN_POINT('Ctrl Pts',(7.11904573622593,-3.95355069855084,3.18037415591442));
#57619=CARTESIAN_POINT('Ctrl Pts',(7.28571428571429,-3.42946788875475,3.42946788875476));
#57620=CARTESIAN_POINT('',(6.82679400487526,-4.78249346839052,2.4759573338791));
#57621=CARTESIAN_POINT('Ctrl Pts',(6.82679400487526,-4.78249346839052,2.4759573338791));
#57622=CARTESIAN_POINT('Ctrl Pts',(6.83650459025506,-4.65899107620553,2.68986975199981));
#57623=CARTESIAN_POINT('Ctrl Pts',(6.82679400487407,-4.53548868402095,2.90378217011979));
#57624=CARTESIAN_POINT('',(7.28571428571429,-4.68474025750198,1.25527236874723));
#57625=CARTESIAN_POINT('Ctrl Pts',(7.28571428571429,-4.68474025750198,1.25527236874723));
#57626=CARTESIAN_POINT('Ctrl Pts',(7.11904573622629,-4.73106016183727,1.83368826214337));
#57627=CARTESIAN_POINT('Ctrl Pts',(6.82679400487526,-4.78249346839052,2.4759573338791));
#57628=CARTESIAN_POINT('',(7.38335469474695,-4.65436776006777,0.875998372175109));
#57629=CARTESIAN_POINT('Ctrl Pts',(7.38335469474695,-4.65436776006777,0.875998372175109));
#57630=CARTESIAN_POINT('Ctrl Pts',(7.34100687338272,-4.66937354687111,1.06338186755417));
#57631=CARTESIAN_POINT('Ctrl Pts',(7.28571428571429,-4.68474025750198,1.25527236874723));
#57632=CARTESIAN_POINT('',(6.94805436450009,-5.2439365747499,3.79002385031413E-13));
#57633=CARTESIAN_POINT('Ctrl Pts',(6.94808683301109,-5.24392552271844,1.87509820678312E-5));
#57634=CARTESIAN_POINT('Ctrl Pts',(7.12497029401787,-5.03766626339576,0.3063486516447));
#57635=CARTESIAN_POINT('Ctrl Pts',(7.26874438305119,-4.84340706140497,0.595319568935955));
#57636=CARTESIAN_POINT('Ctrl Pts',(7.38338779618054,-4.65435739713307,0.876016191369865));
#57637=CARTESIAN_POINT('',(7.46165237939775,-4.51772599325679,-1.07877301257371));
#57638=CARTESIAN_POINT('Ctrl Pts',(7.46165237939775,-4.51772599325679,-1.07877301257371));
#57639=CARTESIAN_POINT('Ctrl Pts',(7.33663088231331,-4.7499056562241,-0.734446773842698));
#57640=CARTESIAN_POINT('Ctrl Pts',(7.16787076968654,-4.98766689283078,-0.380608346073431));
#57641=CARTESIAN_POINT('Ctrl Pts',(6.94809164225636,-5.24392405018006,-2.12859752396575E-5));
#57642=CARTESIAN_POINT('',(7.49999999999943,-4.44436879421741,-1.18641730474127));
#57643=CARTESIAN_POINT('Ctrl Pts',(7.50000000105064,-4.44436879327718,-1.18641730372645));
#57644=CARTESIAN_POINT('Ctrl Pts',(7.48748585582718,-4.46904262342706,-1.15059487498792));
#57645=CARTESIAN_POINT('Ctrl Pts',(7.47470152024076,-4.49349219992046,-1.11471212456586));
#57646=CARTESIAN_POINT('Ctrl Pts',(7.46165237939775,-4.51772599325679,-1.07877301257371));
#57647=CARTESIAN_POINT('',(7.49999999999943,1.18641730474065,4.44436879421757));
#57648=CARTESIAN_POINT('Origin',(7.5,0.,0.));
#57649=CARTESIAN_POINT('Ctrl Pts',(7.46165237939758,1.07877301257324,4.51772599325711));
#57650=CARTESIAN_POINT('Ctrl Pts',(7.47470152024065,1.11471212456534,4.49349219992073));
#57651=CARTESIAN_POINT('Ctrl Pts',(7.48748585582712,1.15059487498736,4.46904262342728));
#57652=CARTESIAN_POINT('Ctrl Pts',(7.50000000105064,1.18641730372584,4.44436879327734));
#57653=CARTESIAN_POINT('Ctrl Pts',(7.38338779618106,-0.876016191369523,
4.65435739713289));
#57654=CARTESIAN_POINT('Ctrl Pts',(7.26874438305275,-0.595319568934126,
4.84340706140535));
#57655=CARTESIAN_POINT('Ctrl Pts',(7.12497029402482,-0.306348651646226,
5.03766626339399));
#57656=CARTESIAN_POINT('Ctrl Pts',(6.94808683301396,-1.87509829813626E-5,
5.24392552271746));
#57657=CARTESIAN_POINT('Origin',(1.5,-4.65899107620574,2.68986975199945));
#57658=CARTESIAN_POINT('',(1.6,-4.53548868402095,2.90378217011979));
#57659=CARTESIAN_POINT('',(1.5,-4.53548868402095,2.90378217011979));
#57660=CARTESIAN_POINT('',(1.6,-4.78249346839052,2.4759573338791));
#57661=CARTESIAN_POINT('',(1.6,-4.21524107620573,3.45846729785813));
#57662=CARTESIAN_POINT('',(1.5,-4.78249346839052,2.4759573338791));
#57663=CARTESIAN_POINT('Origin',(1.5,-3.42946788875475,3.42946788875476));
#57664=CARTESIAN_POINT('',(1.6,-3.42946788875475,3.42946788875476));
#57665=CARTESIAN_POINT('',(1.5,-3.42946788875475,3.42946788875476));
#57666=CARTESIAN_POINT('',(1.6,-1.24762653078691,4.46648531837259));
#57667=CARTESIAN_POINT('Origin',(1.5,2.68986975199945,-4.65899107620574));
#57668=CARTESIAN_POINT('',(6.68133955674308,2.68986975199644,-4.65899107620048));
#57669=CARTESIAN_POINT('',(6.4964847157299,2.47595733387918,-4.78249346839053));
#57670=CARTESIAN_POINT('Ctrl Pts',(6.68133955674087,2.6898697519957,-4.65899107619594));
#57671=CARTESIAN_POINT('Ctrl Pts',(6.67492308098284,2.68233846075464,-4.66333926734057));
#57672=CARTESIAN_POINT('Ctrl Pts',(6.6685005684247,2.67481117074313,-4.6676851311398));
#57673=CARTESIAN_POINT('Ctrl Pts',(6.6620720344556,2.66728791952006,-4.67202864152121));
#57674=CARTESIAN_POINT('Ctrl Pts',(6.6073292890923,2.6032230132773,-4.7090161854831));
#57675=CARTESIAN_POINT('Ctrl Pts',(6.55213434648276,2.53943317427306,-4.74584349646418));
#57676=CARTESIAN_POINT('Ctrl Pts',(6.49649612060902,2.47595028107014,-4.78249290359719));
#57677=CARTESIAN_POINT('',(1.6,2.4759573338791,-4.78249346839052));
#57678=CARTESIAN_POINT('',(1.5,2.4759573338791,-4.78249346839052));
#57679=CARTESIAN_POINT('',(1.6,2.90378217011979,-4.53548868402095));
#57680=CARTESIAN_POINT('',(1.6,4.02111975199945,-3.89039353034704));
#57681=CARTESIAN_POINT('',(6.49648471573067,2.90378217011975,-4.53548868402103));
#57682=CARTESIAN_POINT('',(1.5,2.90378217011979,-4.53548868402095));
#57683=CARTESIAN_POINT('Ctrl Pts',(6.49648471573075,2.90378217011979,-4.53548868402095));
#57684=CARTESIAN_POINT('Ctrl Pts',(6.55337396234641,2.83888253293793,-4.5729585070182));
#57685=CARTESIAN_POINT('Ctrl Pts',(6.60979834671137,2.77366106395271,-4.61061413969377));
#57686=CARTESIAN_POINT('Ctrl Pts',(6.67094806990306,2.70205935512119,-4.65195340556208));
#57687=CARTESIAN_POINT('Ctrl Pts',(6.67614580655144,2.69596587438841,-4.65547147830345));
#57688=CARTESIAN_POINT('Ctrl Pts',(6.68133955672777,2.68986975198969,-4.65899107621137));
#57689=CARTESIAN_POINT('Origin',(1.5,1.25527236874722,-4.68474025750198));
#57690=CARTESIAN_POINT('',(6.9730266888256,1.25527236925909,-4.68474025754297));
#57691=CARTESIAN_POINT('Ctrl Pts',(6.97303770557678,1.25526723923358,-4.68473984672734));
#57692=CARTESIAN_POINT('Ctrl Pts',(6.85768162673857,1.63799446828719,-4.71538888116549));
#57693=CARTESIAN_POINT('Ctrl Pts',(6.70189613372097,2.03849703114157,-4.74746137538506));
#57694=CARTESIAN_POINT('Ctrl Pts',(6.49649612060898,2.47595028107023,-4.7824929035972));
#57695=CARTESIAN_POINT('',(1.6,1.25527236874722,-4.68474025750198));
#57696=CARTESIAN_POINT('',(1.5,1.25527236874722,-4.68474025750198));
#57697=CARTESIAN_POINT('',(1.6,2.20894193499413,-4.76111070924851));
#57698=CARTESIAN_POINT('Ctrl Pts',(6.45213506683142,2.5693960002115,-4.78997609487978));
#57699=CARTESIAN_POINT('Ctrl Pts',(6.69496761877087,2.06333956306628,-4.7494507807858));
#57700=CARTESIAN_POINT('Ctrl Pts',(6.87214261929781,1.60732229617945,-4.71293263455469));
#57701=CARTESIAN_POINT('Ctrl Pts',(6.99737260418699,1.17271712435015,-4.67812918220736));
#57702=CARTESIAN_POINT('Ctrl Pts',(6.59045151583296,2.6420974655224,-4.71093147065315));
#57703=CARTESIAN_POINT('Ctrl Pts',(6.83894619948317,2.13090865278461,-4.67186091612313));
#57704=CARTESIAN_POINT('Ctrl Pts',(7.02199092230211,1.6676886040292,-4.63669438947174));
#57705=CARTESIAN_POINT('Ctrl Pts',(7.15213252925719,1.22335080384112,-4.60270344939976));
#57706=CARTESIAN_POINT('Ctrl Pts',(6.7287679648345,2.7147989308333,-4.63188684642652));
#57707=CARTESIAN_POINT('Ctrl Pts',(6.98292478019547,2.19847774250294,-4.59427105146045));
#57708=CARTESIAN_POINT('Ctrl Pts',(7.17183922530641,1.72805491187895,-4.56045614438878));
#57709=CARTESIAN_POINT('Ctrl Pts',(7.30689245432738,1.27398448333209,-4.52727771659216));
#57710=CARTESIAN_POINT('Ctrl Pts',(6.86708441383604,2.78750039614421,-4.5528422221999));
#57711=CARTESIAN_POINT('Ctrl Pts',(7.12690336090777,2.26604683222127,-4.51668118679778));
#57712=CARTESIAN_POINT('Ctrl Pts',(7.32168752831071,1.78842121972871,-4.48421789930582));
#57713=CARTESIAN_POINT('Ctrl Pts',(7.46165237939758,1.32461816282306,-4.45185198378456));
#57714=CARTESIAN_POINT('',(6.94805436450009,2.62196828737462,-4.54138228956796));
#57715=CARTESIAN_POINT('Ctrl Pts',(6.68133955674308,2.68986975199342,-4.65899107619524));
#57716=CARTESIAN_POINT('Ctrl Pts',(6.76807298446522,2.66766517619599,-4.62053162275364));
#57717=CARTESIAN_POINT('Ctrl Pts',(6.85888718065092,2.64454493763045,-4.58048619487531));
#57718=CARTESIAN_POINT('Ctrl Pts',(6.94805436450009,2.62196828737462,-4.54138228956796));
#57719=CARTESIAN_POINT('',(7.46165237939758,1.32461816282306,-4.45185198378456));
#57720=CARTESIAN_POINT('Ctrl Pts',(6.94809164225473,2.62194359089516,-4.54138208596012));
#57721=CARTESIAN_POINT('Ctrl Pts',(7.16787076968256,2.16421694982277,-4.50975040784356));
#57722=CARTESIAN_POINT('Ctrl Pts',(7.33663088231394,1.73890326423272,-4.4807623507912));
#57723=CARTESIAN_POINT('Ctrl Pts',(7.46165237939758,1.32461816282306,-4.45185198378456));
#57724=CARTESIAN_POINT('',(7.17384635845204,1.23045504008019,-4.59212072600841));
#57725=CARTESIAN_POINT('Ctrl Pts',(7.46165237939758,1.32461816282306,-4.45185198378456));
#57726=CARTESIAN_POINT('Ctrl Pts',(7.36571703908244,1.29323045524197,-4.4986082311925));
#57727=CARTESIAN_POINT('Ctrl Pts',(7.26978169876729,1.26184274766089,-4.54536447860044));
#57728=CARTESIAN_POINT('Ctrl Pts',(7.17384635845215,1.2304550400798,-4.59212072600838));
#57729=CARTESIAN_POINT('Ctrl Pts',(6.97302668796278,1.25527236889283,-4.68474025804403));
#57730=CARTESIAN_POINT('Ctrl Pts',(7.04027818843189,1.24693497884552,-4.65362469478567));
#57731=CARTESIAN_POINT('Ctrl Pts',(7.10373004606705,1.23909393123521,-4.62436150671982));
#57732=CARTESIAN_POINT('Ctrl Pts',(7.17384635845204,1.23045504008019,-4.5921207260084));
#57733=CARTESIAN_POINT('Ctrl Pts',(6.99737260418672,3.46502015180142,-3.35466741224479));
#57734=CARTESIAN_POINT('Ctrl Pts',(6.872142618999,3.27785823931047,-3.74844825878233));
#57735=CARTESIAN_POINT('Ctrl Pts',(6.69496761793157,3.08147524771389,-4.16162987061385));
#57736=CARTESIAN_POINT('Ctrl Pts',(6.45213506509495,2.86354298002157,-4.6201502592847));
#57737=CARTESIAN_POINT('Ctrl Pts',(7.15213252925707,3.37438271134571,-3.3608045985668));
#57738=CARTESIAN_POINT('Ctrl Pts',(7.02199092199136,3.18165082839044,-3.76260789239011));
#57739=CARTESIAN_POINT('Ctrl Pts',(6.83894619861566,2.98049590895782,-4.18135148651518));
#57740=CARTESIAN_POINT('Ctrl Pts',(6.59045151405566,2.75873759472565,-4.64358926304999));
#57741=CARTESIAN_POINT('Ctrl Pts',(7.30689245432741,3.28374527089,-3.3669417848888));
#57742=CARTESIAN_POINT('Ctrl Pts',(7.17183922498372,3.08544341747041,-3.77676752599789));
#57743=CARTESIAN_POINT('Ctrl Pts',(6.98292477929974,2.87951657020175,-4.20107310241652));
#57744=CARTESIAN_POINT('Ctrl Pts',(6.72876796301637,2.65393220942972,-4.66702826681527));
#57745=CARTESIAN_POINT('Ctrl Pts',(7.46165237939775,3.1931078304343,-3.37307897121081));
#57746=CARTESIAN_POINT('Ctrl Pts',(7.32168752797609,2.98923600655038,-3.79092715960567));
#57747=CARTESIAN_POINT('Ctrl Pts',(7.12690335998383,2.77853723144567,-4.22079471831786));
#57748=CARTESIAN_POINT('Ctrl Pts',(6.86708441197709,2.54912682413379,-4.69046727058056));
#57749=CARTESIAN_POINT('',(6.9730266888256,3.42946788921854,-3.42946788853432));
#57750=CARTESIAN_POINT('Ctrl Pts',(6.49649612061063,2.9037852073991,-4.53548229371214));
#57751=CARTESIAN_POINT('Ctrl Pts',(6.70189613387517,3.09217363913432,-4.13912090191365));
#57752=CARTESIAN_POINT('Ctrl Pts',(6.85768162696566,3.26464932591708,-3.77623926085462));
#57753=CARTESIAN_POINT('Ctrl Pts',(6.97303770582829,3.42947009812916,-3.42946324032328));
#57754=CARTESIAN_POINT('',(7.17384635845203,3.36166568592825,-3.36166568592823));
#57755=CARTESIAN_POINT('Ctrl Pts',(6.9730266882762,3.42946788904572,-3.42946788904523));
#57756=CARTESIAN_POINT('Ctrl Pts',(7.04024193630111,3.40670199458592,-3.40670199458569));
#57757=CARTESIAN_POINT('Ctrl Pts',(7.10380439458312,3.38524254899082,-3.38524254899074));
#57758=CARTESIAN_POINT('Ctrl Pts',(7.17384635845204,3.36166568592824,-3.36166568592822));
#57759=CARTESIAN_POINT('',(7.46165237939775,3.1931078304343,-3.37307897121081));
#57760=CARTESIAN_POINT('Ctrl Pts',(7.46165237939775,3.1931078304343,-3.37307897121081));
#57761=CARTESIAN_POINT('Ctrl Pts',(7.36571703908251,3.24929378226561,-3.36927454278328));
#57762=CARTESIAN_POINT('Ctrl Pts',(7.26978169876727,3.30547973409693,-3.36547011435575));
#57763=CARTESIAN_POINT('Ctrl Pts',(7.17384635845203,3.36166568592825,-3.36166568592823));
#57764=CARTESIAN_POINT('Ctrl Pts',(7.46165237939775,3.1931078304343,-3.37307897121081));
#57765=CARTESIAN_POINT('Ctrl Pts',(7.33663088231331,3.01100239198735,-3.74631557694812));
#57766=CARTESIAN_POINT('Ctrl Pts',(7.16787076968672,2.82344994300742,-4.12914206176923));
#57767=CARTESIAN_POINT('Ctrl Pts',(6.94809164225641,2.62198045928535,-4.54136079998446));
#57768=CARTESIAN_POINT('Origin',(1.5,4.65899107620573,-2.68986975199945));
#57769=CARTESIAN_POINT('',(6.68133955674308,4.65899107620051,-2.6898697519964));
#57770=CARTESIAN_POINT('',(6.4964847157299,4.53548868402102,-2.90378217011975));
#57771=CARTESIAN_POINT('Ctrl Pts',(6.68133955674087,4.65899107619759,-2.68986975199284));
#57772=CARTESIAN_POINT('Ctrl Pts',(6.67492308098284,4.65464288223185,-2.69740104160513));
#57773=CARTESIAN_POINT('Ctrl Pts',(6.6685005684247,4.65029698975985,-2.7049283150624));
#57774=CARTESIAN_POINT('Ctrl Pts',(6.6620720344556,4.64595341827232,-2.71245153100584));
#57775=CARTESIAN_POINT('Ctrl Pts',(6.6073292890926,4.60896535395617,-2.77651613682146));
#57776=CARTESIAN_POINT('Ctrl Pts',(6.55213434648291,4.57213538836561,-2.84030444318645));
#57777=CARTESIAN_POINT('Ctrl Pts',(6.49649612060902,4.53548229371255,-2.90378520739891));
#57778=CARTESIAN_POINT('',(1.6,4.53548868402095,-2.90378217011979));
#57779=CARTESIAN_POINT('',(1.5,4.53548868402095,-2.90378217011979));
#57780=CARTESIAN_POINT('',(1.6,4.78249346839052,-2.47595733387911));
#57781=CARTESIAN_POINT('',(1.6,5.10274107620574,-1.92127220614076));
#57782=CARTESIAN_POINT('',(6.49648471573067,4.78249346839052,-2.47595733387919));
#57783=CARTESIAN_POINT('',(1.5,4.78249346839052,-2.47595733387911));
#57784=CARTESIAN_POINT('Ctrl Pts',(6.49648471573075,4.78249346839052,-2.4759573338791));
#57785=CARTESIAN_POINT('Ctrl Pts',(6.55337396234637,4.74502364539329,-2.54085697106091));
#57786=CARTESIAN_POINT('Ctrl Pts',(6.60979834671129,4.70736801271776,-2.60607844004609));
#57787=CARTESIAN_POINT('Ctrl Pts',(6.67094806990306,4.66602874684939,-2.6776801488777));
#57788=CARTESIAN_POINT('Ctrl Pts',(6.67614580655144,4.66251067410802,-2.68377362961048));
#57789=CARTESIAN_POINT('Ctrl Pts',(6.68133955672777,4.6589910762001,-2.6898697520092));
#57790=CARTESIAN_POINT('Origin',(1.5,3.42946788875475,-3.42946788875476));
#57791=CARTESIAN_POINT('Ctrl Pts',(6.97303770557678,3.42946324107831,-3.4294700977703));
#57792=CARTESIAN_POINT('Ctrl Pts',(6.85768162673857,3.77623926137783,-3.26464932566841));
#57793=CARTESIAN_POINT('Ctrl Pts',(6.70189613372097,4.13912090220029,-3.09217363899809));
#57794=CARTESIAN_POINT('Ctrl Pts',(6.49649612060898,4.53548229371264,-2.90378520739886));
#57795=CARTESIAN_POINT('',(1.6,3.42946788875475,-3.42946788875476));
#57796=CARTESIAN_POINT('',(1.5,3.42946788875475,-3.42946788875476));
#57797=CARTESIAN_POINT('',(1.6,4.14344644123463,-3.09011773362498));
#57798=CARTESIAN_POINT('Ctrl Pts',(6.45213506683141,4.62015025600519,-2.86354298158031));
#57799=CARTESIAN_POINT('Ctrl Pts',(6.69496761877087,4.1616298686418,-3.0814752486512));
#57800=CARTESIAN_POINT('Ctrl Pts',(6.87214261929781,3.74844825783789,-3.27785823975936));
#57801=CARTESIAN_POINT('Ctrl Pts',(6.99737260418699,3.35466741224394,-3.46502015180182));
#57802=CARTESIAN_POINT('Ctrl Pts',(6.59045151583295,4.64358925974348,-2.758737596312));
#57803=CARTESIAN_POINT('Ctrl Pts',(6.83894619948317,4.18135148451713,-2.98049590991796));
#57804=CARTESIAN_POINT('Ctrl Pts',(7.02199092230211,3.76260789142697,-3.1816508288527));
#57805=CARTESIAN_POINT('Ctrl Pts',(7.15213252925719,3.3608045985664,-3.3743827113459));
#57806=CARTESIAN_POINT('Ctrl Pts',(6.72876796483449,4.66702826348176,-2.6539322110437));
#57807=CARTESIAN_POINT('Ctrl Pts',(6.98292478019547,4.20107310039245,-2.87951657118472));
#57808=CARTESIAN_POINT('Ctrl Pts',(7.17183922530641,3.77676752501605,-3.08544341794604));
#57809=CARTESIAN_POINT('Ctrl Pts',(7.30689245432738,3.36694178488886,-3.28374527088997));
#57810=CARTESIAN_POINT('Ctrl Pts',(6.86708441383603,4.69046726722004,-2.5491268257754));
#57811=CARTESIAN_POINT('Ctrl Pts',(7.12690336090776,4.22079471626778,-2.77853723245148));
#57812=CARTESIAN_POINT('Ctrl Pts',(7.32168752831071,3.79092715860513,-2.98923600703938));
#57813=CARTESIAN_POINT('Ctrl Pts',(7.46165237939758,3.37307897121132,-3.19310783043405));
#57814=CARTESIAN_POINT('',(6.94805436450009,4.54138228956758,-2.62196828737528));
#57815=CARTESIAN_POINT('Ctrl Pts',(6.68133955674308,4.65899107619527,-2.68986975199337));
#57816=CARTESIAN_POINT('Ctrl Pts',(6.76807293638616,4.62053164407291,-2.66766518850469));
#57817=CARTESIAN_POINT('Ctrl Pts',(6.8588871155266,4.58048622343516,-2.64454495411985));
#57818=CARTESIAN_POINT('Ctrl Pts',(6.94805436450009,4.54138228956758,-2.62196828737528));
#57819=CARTESIAN_POINT('',(7.46165237939758,3.37307897121132,-3.19310783043405));
#57820=CARTESIAN_POINT('Ctrl Pts',(6.94809164225473,4.54136079998506,-2.62198045928545));
#57821=CARTESIAN_POINT('Ctrl Pts',(7.16787076968256,4.12914206176917,-2.82344994300837));
#57822=CARTESIAN_POINT('Ctrl Pts',(7.33663088231394,3.74631557694482,-3.0110023919897));
#57823=CARTESIAN_POINT('Ctrl Pts',(7.46165237939758,3.37307897121132,-3.19310783043405));
#57824=CARTESIAN_POINT('Ctrl Pts',(7.46165237939758,3.37307897121132,-3.19310783043405));
#57825=CARTESIAN_POINT('Ctrl Pts',(7.36571703908244,3.36927454278351,-3.2492937822655));
#57826=CARTESIAN_POINT('Ctrl Pts',(7.26978169876729,3.3654701143557,-3.30547973409695));
#57827=CARTESIAN_POINT('Ctrl Pts',(7.17384635845215,3.36166568592789,-3.36166568592839));
#57828=CARTESIAN_POINT('Ctrl Pts',(6.99737260418672,4.67812918220743,-1.17271712435108));
#57829=CARTESIAN_POINT('Ctrl Pts',(6.872142618999,4.71293263463817,-1.60732229722181));
#57830=CARTESIAN_POINT('Ctrl Pts',(6.69496761793157,4.7494507809601,-2.06333956524279));
#57831=CARTESIAN_POINT('Ctrl Pts',(6.45213506509495,4.78997609516963,-2.56939600383103));
#57832=CARTESIAN_POINT('Ctrl Pts',(7.15213252925707,4.6027034493998,-1.22335080384155));
#57833=CARTESIAN_POINT('Ctrl Pts',(7.02199092199136,4.63669438955298,-1.66768860509444));
#57834=CARTESIAN_POINT('Ctrl Pts',(6.83894619861566,4.67186091629066,-2.13090865499507));
#57835=CARTESIAN_POINT('Ctrl Pts',(6.59045151405566,4.71093147093258,-2.64209746917913));
#57836=CARTESIAN_POINT('Ctrl Pts',(7.30689245432741,4.52727771659216,-1.27398448333202));
#57837=CARTESIAN_POINT('Ctrl Pts',(7.17183922498372,4.56045614446779,-1.72805491296707));
#57838=CARTESIAN_POINT('Ctrl Pts',(6.98292477929974,4.59427105162121,-2.19847774474734));
#57839=CARTESIAN_POINT('Ctrl Pts',(6.72876796301638,4.63188684669553,-2.71479893452723));
#57840=CARTESIAN_POINT('Ctrl Pts',(7.46165237939775,4.45185198378452,-1.32461816282249));
#57841=CARTESIAN_POINT('Ctrl Pts',(7.32168752797609,4.48421789938261,-1.7884212208397));
#57842=CARTESIAN_POINT('Ctrl Pts',(7.12690335998383,4.51668118695177,-2.26604683449962));
#57843=CARTESIAN_POINT('Ctrl Pts',(6.86708441197709,4.55284222245849,-2.78750039987533));
#57844=CARTESIAN_POINT('',(6.9730266888256,4.68474025779341,-1.25527236832443));
#57845=CARTESIAN_POINT('Ctrl Pts',(6.49649612061063,4.78249290359715,-2.47595028106968));
#57846=CARTESIAN_POINT('Ctrl Pts',(6.70189613387517,4.74746137535973,-2.03849703082522));
#57847=CARTESIAN_POINT('Ctrl Pts',(6.85768162696566,4.71538888111925,-1.63799446770973));
#57848=CARTESIAN_POINT('Ctrl Pts',(6.97303770582829,4.68473984666061,-1.25526723840028));
#57849=CARTESIAN_POINT('',(7.17384635845204,4.59212072600841,-1.23045504008016));
#57850=CARTESIAN_POINT('Ctrl Pts',(6.9730266882762,4.6847402578992,-1.2552723688533));
#57851=CARTESIAN_POINT('Ctrl Pts',(7.04024207626693,4.65364140296873,-1.24693945578933));
#57852=CARTESIAN_POINT('Ctrl Pts',(7.10380410094938,4.62432745491165,-1.23908480708058));
#57853=CARTESIAN_POINT('Ctrl Pts',(7.17384635845203,4.59212072600842,-1.23045504008016));
#57854=CARTESIAN_POINT('',(7.46165237939775,4.45185198378452,-1.32461816282249));
#57855=CARTESIAN_POINT('Ctrl Pts',(7.46165237939775,4.45185198378452,-1.32461816282249));
#57856=CARTESIAN_POINT('Ctrl Pts',(7.36571703908251,4.49860823119249,-1.29323045524171));
#57857=CARTESIAN_POINT('Ctrl Pts',(7.26978169876728,4.54536447860045,-1.26184274766094));
#57858=CARTESIAN_POINT('Ctrl Pts',(7.17384635845204,4.59212072600841,-1.23045504008016));
#57859=CARTESIAN_POINT('Ctrl Pts',(7.46165237939775,4.45185198378452,-1.32461816282249));
#57860=CARTESIAN_POINT('Ctrl Pts',(7.33663088231331,4.48076235079081,-1.73890326423675));
#57861=CARTESIAN_POINT('Ctrl Pts',(7.16787076968672,4.50975040784277,-2.1642169498233));
#57862=CARTESIAN_POINT('Ctrl Pts',(6.94809164225642,4.54138208595974,-2.62194359089469));
#57863=CARTESIAN_POINT('Origin',(1.5,5.37973950399889,-3.46944695195361E-17));
#57864=CARTESIAN_POINT('',(6.68133955674308,5.37973950399284,2.68350805758692E-14));
#57865=CARTESIAN_POINT('',(6.4964847157299,5.37973950399894,-0.2470047843695));
#57866=CARTESIAN_POINT('Ctrl Pts',(6.68133955674087,5.37973950398853,1.65381597305725E-12));
#57867=CARTESIAN_POINT('Ctrl Pts',(6.67492308098284,5.37973950235977,-0.00869638510872296));
#57868=CARTESIAN_POINT('Ctrl Pts',(6.6685005684247,5.37973948580553,-0.0173881413799512));
#57869=CARTESIAN_POINT('Ctrl Pts',(6.6620720344556,5.3797394505259,-0.0260752232488909));
#57870=CARTESIAN_POINT('Ctrl Pts',(6.6073292890922,5.37973915009911,-0.100050831527283));
#57871=CARTESIAN_POINT('Ctrl Pts',(6.55213434648271,5.37973761745967,-0.173708108098733));
#57872=CARTESIAN_POINT('Ctrl Pts',(6.49649612060902,5.37973548846904,-0.247010609884637));
#57873=CARTESIAN_POINT('',(1.6,5.37973950399889,-0.247004784369567));
#57874=CARTESIAN_POINT('',(1.5,5.37973950399889,-0.247004784369567));
#57875=CARTESIAN_POINT('',(1.6,5.37973950399889,0.247004784369567));
#57876=CARTESIAN_POINT('',(1.6,5.37973950399889,-1.73472347597681E-17));
#57877=CARTESIAN_POINT('',(6.49648471573067,5.37973950399894,0.247004784369499));
#57878=CARTESIAN_POINT('',(1.5,5.37973950399889,0.247004784369567));
#57879=CARTESIAN_POINT('Ctrl Pts',(6.49648471573075,5.37973950399889,0.247004784369566));
#57880=CARTESIAN_POINT('Ctrl Pts',(6.55337396234643,5.37973950399889,0.172065138375048));
#57881=CARTESIAN_POINT('Ctrl Pts',(6.60979834671138,5.37973950399889,0.0967538730239298));
#57882=CARTESIAN_POINT('Ctrl Pts',(6.67094806990306,5.37973950399889,0.0140753412873033));
#57883=CARTESIAN_POINT('Ctrl Pts',(6.67614580655144,5.37973950399889,0.00703919580456445));
#57884=CARTESIAN_POINT('Ctrl Pts',(6.68133955672778,5.37973950399889,-1.12624232856406E-11));
#57885=CARTESIAN_POINT('Origin',(1.5,4.68474025750198,-1.25527236874722));
#57886=CARTESIAN_POINT('Ctrl Pts',(6.97303770557678,4.68473733700388,-1.25527660564903));
#57887=CARTESIAN_POINT('Ctrl Pts',(6.85768162673858,4.90264379395559,-0.939149619787658));
#57888=CARTESIAN_POINT('Ctrl Pts',(6.70189613372098,5.13067067013966,-0.608340473184774));
#57889=CARTESIAN_POINT('Ctrl Pts',(6.49649612060898,5.37973548846909,-0.24701060988456));
#57890=CARTESIAN_POINT('',(1.6,4.68474025750198,-1.25527236874722));
#57891=CARTESIAN_POINT('',(1.5,4.68474025750198,-1.25527236874722));
#57892=CARTESIAN_POINT('',(1.6,4.79527416765606,-1.09491570772261));
#57893=CARTESIAN_POINT('Ctrl Pts',(6.45213506683129,5.43293898179196,-0.169825838874389));
#57894=CARTESIAN_POINT('Ctrl Pts',(6.69496761877082,5.14481481171758,-0.587820912143886));
#57895=CARTESIAN_POINT('Ctrl Pts',(6.8721426192978,4.88518053593885,-0.964484376716747));
#57896=CARTESIAN_POINT('Ctrl Pts',(6.99737260418699,4.63773727615197,-1.32346176996341));
#57897=CARTESIAN_POINT('Ctrl Pts',(6.59045151583283,5.40083506183456,-0.0673422109094779));
#57898=CARTESIAN_POINT('Ctrl Pts',(6.83894619948311,5.11140456270267,-0.490509431605882));
#57899=CARTESIAN_POINT('Ctrl Pts',(7.02199092230209,4.84933943288195,-0.874086498044709));
#57900=CARTESIAN_POINT('Ctrl Pts',(7.15213252925719,4.59773351518701,-1.24189885083336));
#57901=CARTESIAN_POINT('Ctrl Pts',(6.72876796483437,5.36873114187716,0.0351414170554329));
#57902=CARTESIAN_POINT('Ctrl Pts',(6.98292478019541,5.07799431368776,-0.393197951067879));
#57903=CARTESIAN_POINT('Ctrl Pts',(7.17183922530639,4.81349832982504,-0.783688619372671));
#57904=CARTESIAN_POINT('Ctrl Pts',(7.30689245432738,4.55772975422206,-1.1603359317033));
#57905=CARTESIAN_POINT('Ctrl Pts',(6.86708441383591,5.33662722191976,0.137625045020344));
#57906=CARTESIAN_POINT('Ctrl Pts',(7.12690336090771,5.04458406467285,-0.295886470529875));
#57907=CARTESIAN_POINT('Ctrl Pts',(7.32168752831068,4.77765722676813,-0.693290740700633));
#57908=CARTESIAN_POINT('Ctrl Pts',(7.46165237939758,4.51772599325711,-1.07877301257324));
#57909=CARTESIAN_POINT('',(6.94805436450009,5.2439365747499,-3.78100328823905E-13));
#57910=CARTESIAN_POINT('Ctrl Pts',(6.94805436450009,5.2439365747499,-3.77996245415346E-13));
#57911=CARTESIAN_POINT('Ctrl Pts',(6.85888652980287,5.2890902048436,-1.56816092780279E-13));
#57912=CARTESIAN_POINT('Ctrl Pts',(6.76807250396892,5.33533059841515,-3.28976807639418E-15));
#57913=CARTESIAN_POINT('Ctrl Pts',(6.68133955674308,5.37973950398679,2.77382283808691E-14));
#57914=CARTESIAN_POINT('',(7.46165237939758,4.51772599325711,-1.07877301257324));
#57915=CARTESIAN_POINT('Ctrl Pts',(6.94809164225473,5.24392405018061,-2.1285975059784E-5));
#57916=CARTESIAN_POINT('Ctrl Pts',(7.16787076968256,4.98766689283114,-0.380608346074386));
#57917=CARTESIAN_POINT('Ctrl Pts',(7.33663088231394,4.74990565622242,-0.734446773846379));
#57918=CARTESIAN_POINT('Ctrl Pts',(7.46165237939758,4.51772599325711,-1.07877301257324));
#57919=CARTESIAN_POINT('Ctrl Pts',(7.46165237939758,4.51772599325711,-1.07877301257324));
#57920=CARTESIAN_POINT('Ctrl Pts',(7.36571703908244,4.54252423750747,-1.12933368840899));
#57921=CARTESIAN_POINT('Ctrl Pts',(7.26978169876729,4.56732248175783,-1.17989436424473));
#57922=CARTESIAN_POINT('Ctrl Pts',(7.17384635845215,4.59212072600819,-1.23045504008048));
#57923=CARTESIAN_POINT('Origin',(1.5,-5.37973950399889,6.24500451351651E-16));
#57924=CARTESIAN_POINT('',(6.68133955603507,-5.3797395041741,-2.68543263356575E-14));
#57925=CARTESIAN_POINT('',(6.49648471572948,-5.37973950399919,0.247004784369128));
#57926=CARTESIAN_POINT('Ctrl Pts',(6.68133955609892,-5.37973950429881,4.70876809766096E-11));
#57927=CARTESIAN_POINT('Ctrl Pts',(6.67484047849818,-5.37973950253171,0.00880833749040602));
#57928=CARTESIAN_POINT('Ctrl Pts',(6.66833520149437,-5.37973948712148,0.0176119236098385));
#57929=CARTESIAN_POINT('Ctrl Pts',(6.66182374103212,-5.37973945439155,0.0264107107560584));
#57930=CARTESIAN_POINT('Ctrl Pts',(6.60716230063611,-5.3797391796352,0.100273461200274));
#57931=CARTESIAN_POINT('Ctrl Pts',(6.55204961798885,-5.3797377938976,0.173818622858807));
#57932=CARTESIAN_POINT('Ctrl Pts',(6.49649473556378,-5.37973586027059,0.247010070494919));
#57933=CARTESIAN_POINT('',(1.6,-5.37973950399889,0.247004784369568));
#57934=CARTESIAN_POINT('',(1.5,-5.37973950399889,0.247004784369567));
#57935=CARTESIAN_POINT('',(1.6,-5.37973950399889,-0.247004784369566));
#57936=CARTESIAN_POINT('',(1.6,-5.37973950399889,3.12250225675825E-16));
#57937=CARTESIAN_POINT('',(6.49648471573068,-5.37973950399894,-0.247004784369499));
#57938=CARTESIAN_POINT('',(1.5,-5.37973950399889,-0.247004784369566));
#57939=CARTESIAN_POINT('Ctrl Pts',(6.49648471573075,-5.37973950399889,-0.247004784369566));
#57940=CARTESIAN_POINT('Ctrl Pts',(6.55337396234644,-5.37973950399889,-0.172065138375028));
#57941=CARTESIAN_POINT('Ctrl Pts',(6.60979834671144,-5.37973950399889,-0.0967538730238504));
#57942=CARTESIAN_POINT('Ctrl Pts',(6.67094806981975,-5.37973950399889,-0.0140753413999544));
#57943=CARTESIAN_POINT('Ctrl Pts',(6.67614580638494,-5.37973950399889,-0.00703919602996617));
#57944=CARTESIAN_POINT('Ctrl Pts',(6.6813395564782,-5.37973950399889,-3.26986319965084E-10));
#57945=CARTESIAN_POINT('Origin',(1.5,-4.68474025750198,1.25527236874723));
#57946=CARTESIAN_POINT('',(6.97302668913438,-4.68474025750198,1.25527236874723));
#57947=CARTESIAN_POINT('Ctrl Pts',(6.97302668913438,-4.68474025750198,1.25527236874723));
#57948=CARTESIAN_POINT('Ctrl Pts',(6.85757546768185,-4.90267228949946,0.939108279982866));
#57949=CARTESIAN_POINT('Ctrl Pts',(6.70188214814575,-5.1306744242805,0.608335026878845));
#57950=CARTESIAN_POINT('Ctrl Pts',(6.49649473556348,-5.37973586027094,0.247010070494401));
#57951=CARTESIAN_POINT('',(1.6,-4.68474025750198,1.25527236874723));
#57952=CARTESIAN_POINT('',(1.5,-4.68474025750198,1.25527236874723));
#57953=CARTESIAN_POINT('',(1.6,-3.65183350576906,2.75375801561154));
#57954=CARTESIAN_POINT('Ctrl Pts',(6.45213506859891,-5.43293897969466,0.169825841917048));
#57955=CARTESIAN_POINT('Ctrl Pts',(6.67964185096999,-5.16299904623435,0.561440201226003));
#57956=CARTESIAN_POINT('Ctrl Pts',(6.84940428693712,-4.91809665661411,0.916731436483211));
#57957=CARTESIAN_POINT('Ctrl Pts',(6.97302668913438,-4.68474025750198,1.25527236874723));
#57958=CARTESIAN_POINT('Ctrl Pts',(6.59045151764167,-5.40083505972775,0.0673422139897861));
#57959=CARTESIAN_POINT('Ctrl Pts',(6.82326308044043,-5.12967124289664,0.463802293582382));
#57960=CARTESIAN_POINT('Ctrl Pts',(6.99850389520073,-4.88256196744721,0.825458102897624));
#57961=CARTESIAN_POINT('Ctrl Pts',(7.12684466416208,-4.64550450560471,1.17205861623332));
#57962=CARTESIAN_POINT('Ctrl Pts',(6.72876796668442,-5.36873113976084,-0.0351414139374756));
#57963=CARTESIAN_POINT('Ctrl Pts',(6.96688430991087,-5.09634343955894,0.366164385938763));
#57964=CARTESIAN_POINT('Ctrl Pts',(7.14760350346434,-4.84702727828031,0.734184769312034));
#57965=CARTESIAN_POINT('Ctrl Pts',(7.28066263918978,-4.60626875370745,1.08884486371941));
#57966=CARTESIAN_POINT('Ctrl Pts',(6.86708441572717,-5.33662721979393,-0.137625041864737));
#57967=CARTESIAN_POINT('Ctrl Pts',(7.11050553938132,-5.06301563622124,0.268526478295141));
#57968=CARTESIAN_POINT('Ctrl Pts',(7.29670311172796,-4.81149258911341,0.642911435726447));
#57969=CARTESIAN_POINT('Ctrl Pts',(7.43448061421748,-4.56703300181018,1.0056311112055));
#57970=CARTESIAN_POINT('Ctrl Pts',(6.68133955603507,-5.3797395043493,-2.62984078958084E-14));
#57971=CARTESIAN_POINT('Ctrl Pts',(6.77016782808452,-5.33425770985245,1.14024814220434E-7));
#57972=CARTESIAN_POINT('Ctrl Pts',(6.85900408935791,-5.28903269339668,7.30333645709156E-6));
#57973=CARTESIAN_POINT('Ctrl Pts',(6.94808683301108,-5.24392552271845,1.87509820665649E-5));
#57974=CARTESIAN_POINT('Ctrl Pts',(6.97302668913438,-4.68474025750198,1.25527236874723));
#57975=CARTESIAN_POINT('Ctrl Pts',(7.04204931539975,-4.67972462592243,1.1926400929975));
#57976=CARTESIAN_POINT('Ctrl Pts',(7.11079264180597,-4.67468173820311,1.12966745850414));
#57977=CARTESIAN_POINT('Ctrl Pts',(7.24755133540632,-4.66455755467053,1.00324257168837));
#57978=CARTESIAN_POINT('Ctrl Pts',(7.31560085004917,-4.6594738889069,0.939760724810945));
#57979=CARTESIAN_POINT('Ctrl Pts',(7.38335469474695,-4.65436776006777,0.875998372175109));
#57980=CARTESIAN_POINT('Ctrl Pts',(6.99737260418672,-4.6377372761525,-1.32346176996264));
#57981=CARTESIAN_POINT('Ctrl Pts',(6.87214261900943,-4.88518053651166,-0.964484375885747));
#57982=CARTESIAN_POINT('Ctrl Pts',(6.69496761796091,-5.14481481291349,-0.58782091040892));
#57983=CARTESIAN_POINT('Ctrl Pts',(6.45213506515565,-5.43293898378058,-0.169825835989406));
#57984=CARTESIAN_POINT('Ctrl Pts',(7.15213252925706,-4.59773351518726,-1.241898850833));
#57985=CARTESIAN_POINT('Ctrl Pts',(7.0219909220022,-4.84933943346392,-0.874086497193518));
#57986=CARTESIAN_POINT('Ctrl Pts',(6.83894619864596,-5.11140456390929,-0.490509429839278));
#57987=CARTESIAN_POINT('Ctrl Pts',(6.59045151411778,-5.40083506383243,-0.0673422079883656));
#57988=CARTESIAN_POINT('Ctrl Pts',(7.30689245432741,-4.55772975422203,-1.16033593170336));
#57989=CARTESIAN_POINT('Ctrl Pts',(7.17183922499498,-4.81349833041617,-0.783688618501289));
#57990=CARTESIAN_POINT('Ctrl Pts',(6.98292477933101,-5.07799431490509,-0.393197949269635));
#57991=CARTESIAN_POINT('Ctrl Pts',(6.7287679630799,-5.36873114388427,0.035141420012675));
#57992=CARTESIAN_POINT('Ctrl Pts',(7.46165237939775,-4.51772599325679,-1.07877301257371));
#57993=CARTESIAN_POINT('Ctrl Pts',(7.32168752798775,-4.77765722736842,-0.693290739809061));
#57994=CARTESIAN_POINT('Ctrl Pts',(7.12690336001606,-5.04458406590089,-0.295886468699992));
#57995=CARTESIAN_POINT('Ctrl Pts',(6.86708441204203,-5.33662722393612,0.137625048013716));
#57996=CARTESIAN_POINT('',(6.9730266888256,-4.68474025754297,-1.25527236925909));
#57997=CARTESIAN_POINT('Ctrl Pts',(6.49649612061061,-5.37973548846879,-0.247010609885));
#57998=CARTESIAN_POINT('Ctrl Pts',(6.70189613387502,-5.1306706699596,-0.608340473445991));
#57999=CARTESIAN_POINT('Ctrl Pts',(6.85768162696565,-4.90264379362682,-0.939149620264615));
#58000=CARTESIAN_POINT('Ctrl Pts',(6.97303770582828,-4.68473733652944,-1.25527660633732));
#58001=CARTESIAN_POINT('',(7.17384635845204,-4.5921207260084,-1.23045504008019));
#58002=CARTESIAN_POINT('Ctrl Pts',(6.97302668796278,-4.68474025804403,-1.25527236889283));
#58003=CARTESIAN_POINT('Ctrl Pts',(7.04027818843198,-4.65362469478563,-1.24693497884551));
#58004=CARTESIAN_POINT('Ctrl Pts',(7.10373004606737,-4.62436150671968,-1.23909393123517));
#58005=CARTESIAN_POINT('Ctrl Pts',(7.17384635845204,-4.5921207260084,-1.23045504008019));
#58006=CARTESIAN_POINT('Ctrl Pts',(7.46165237939775,-4.51772599325679,-1.07877301257371));
#58007=CARTESIAN_POINT('Ctrl Pts',(7.36571703908252,-4.54252423750733,-1.1293336884092));
#58008=CARTESIAN_POINT('Ctrl Pts',(7.26978169876728,-4.56732248175787,-1.17989436424469));
#58009=CARTESIAN_POINT('Ctrl Pts',(7.17384635845204,-4.5921207260084,-1.23045504008019));
#58010=CARTESIAN_POINT('Origin',(1.5,-4.65899107620574,-2.68986975199945));
#58011=CARTESIAN_POINT('',(6.68133955674308,-4.65899107620048,-2.68986975199644));
#58012=CARTESIAN_POINT('',(6.4964847157299,-4.78249346839053,-2.47595733387918));
#58013=CARTESIAN_POINT('Ctrl Pts',(6.68133955674087,-4.65899107619594,-2.6898697519957));
#58014=CARTESIAN_POINT('Ctrl Pts',(6.67492308098284,-4.66333926734057,-2.68233846075464));
#58015=CARTESIAN_POINT('Ctrl Pts',(6.6685005684247,-4.6676851311398,-2.67481117074314));
#58016=CARTESIAN_POINT('Ctrl Pts',(6.6620720344556,-4.67202864152121,-2.66728791952006));
#58017=CARTESIAN_POINT('Ctrl Pts',(6.60732928909247,-4.70901618548299,-2.60322301327749));
#58018=CARTESIAN_POINT('Ctrl Pts',(6.55213434648284,-4.74584349646412,-2.53943317427315));
#58019=CARTESIAN_POINT('Ctrl Pts',(6.49649612060902,-4.78249290359719,-2.47595028107014));
#58020=CARTESIAN_POINT('',(1.6,-4.78249346839052,-2.4759573338791));
#58021=CARTESIAN_POINT('',(1.5,-4.78249346839052,-2.4759573338791));
#58022=CARTESIAN_POINT('',(1.6,-4.53548868402095,-2.90378217011979));
#58023=CARTESIAN_POINT('',(1.6,-4.21524107620573,-3.45846729785814));
#58024=CARTESIAN_POINT('',(6.49648471573068,-4.53548868402103,-2.90378217011975));
#58025=CARTESIAN_POINT('',(1.5,-4.53548868402095,-2.90378217011979));
#58026=CARTESIAN_POINT('Ctrl Pts',(6.49648471573075,-4.53548868402095,-2.90378217011979));
#58027=CARTESIAN_POINT('Ctrl Pts',(6.55337396234641,-4.5729585070182,-2.83888253293794));
#58028=CARTESIAN_POINT('Ctrl Pts',(6.60979834671136,-4.61061413969376,-2.77366106395272));
#58029=CARTESIAN_POINT('Ctrl Pts',(6.67094806990306,-4.65195340556208,-2.70205935512119));
#58030=CARTESIAN_POINT('Ctrl Pts',(6.67614580655144,-4.65547147830345,-2.69596587438841));
#58031=CARTESIAN_POINT('Ctrl Pts',(6.68133955672777,-4.65899107621137,-2.68986975198969));
#58032=CARTESIAN_POINT('Origin',(1.5,-4.68474025750198,-1.25527236874723));
#58033=CARTESIAN_POINT('Ctrl Pts',(6.97303770557678,-4.68473984672734,-1.25526723923358));
#58034=CARTESIAN_POINT('Ctrl Pts',(6.85768162673857,-4.71538888116549,-1.63799446828719));
#58035=CARTESIAN_POINT('Ctrl Pts',(6.70189613372097,-4.74746137538506,-2.03849703114157));
#58036=CARTESIAN_POINT('Ctrl Pts',(6.49649612060898,-4.7824929035972,-2.47595028107023));
#58037=CARTESIAN_POINT('',(1.6,-4.68474025750198,-1.25527236874723));
#58038=CARTESIAN_POINT('',(1.5,-4.68474025750198,-1.25527236874723));
#58039=CARTESIAN_POINT('',(1.6,-4.6085629719582,-0.304014949143111));
#58040=CARTESIAN_POINT('Ctrl Pts',(6.45213506683142,-4.78997609487978,-2.5693960002115));
#58041=CARTESIAN_POINT('Ctrl Pts',(6.69496761877088,-4.74945078078581,-2.06333956306629));
#58042=CARTESIAN_POINT('Ctrl Pts',(6.87214261929782,-4.71293263455469,-1.60732229617945));
#58043=CARTESIAN_POINT('Ctrl Pts',(6.99737260418699,-4.67812918220736,-1.17271712435015));
#58044=CARTESIAN_POINT('Ctrl Pts',(6.59045151583296,-4.71093147065315,-2.6420974655224));
#58045=CARTESIAN_POINT('Ctrl Pts',(6.83894619948317,-4.67186091612313,-2.13090865278462));
#58046=CARTESIAN_POINT('Ctrl Pts',(7.02199092230211,-4.63669438947174,-1.6676886040292));
#58047=CARTESIAN_POINT('Ctrl Pts',(7.15213252925719,-4.60270344939976,-1.22335080384112));
#58048=CARTESIAN_POINT('Ctrl Pts',(6.7287679648345,-4.63188684642652,-2.7147989308333));
#58049=CARTESIAN_POINT('Ctrl Pts',(6.98292478019547,-4.59427105146045,-2.19847774250294));
#58050=CARTESIAN_POINT('Ctrl Pts',(7.17183922530641,-4.56045614438878,-1.72805491187896));
#58051=CARTESIAN_POINT('Ctrl Pts',(7.30689245432738,-4.52727771659216,-1.27398448333209));
#58052=CARTESIAN_POINT('Ctrl Pts',(6.86708441383604,-4.5528422221999,-2.78750039614421));
#58053=CARTESIAN_POINT('Ctrl Pts',(7.12690336090777,-4.51668118679778,-2.26604683222127));
#58054=CARTESIAN_POINT('Ctrl Pts',(7.32168752831071,-4.48421789930582,-1.78842121972871));
#58055=CARTESIAN_POINT('Ctrl Pts',(7.46165237939758,-4.45185198378456,-1.32461816282306));
#58056=CARTESIAN_POINT('',(6.94805436450009,-4.54138228956795,-2.62196828737462));
#58057=CARTESIAN_POINT('Ctrl Pts',(6.68133955674307,-4.65899107619524,-2.68986975199342));
#58058=CARTESIAN_POINT('Ctrl Pts',(6.76807298446519,-4.62053162275365,-2.66766517619599));
#58059=CARTESIAN_POINT('Ctrl Pts',(6.85888718065087,-4.58048619487533,-2.64454493763046));
#58060=CARTESIAN_POINT('Ctrl Pts',(6.94805436450009,-4.54138228956796,-2.62196828737462));
#58061=CARTESIAN_POINT('',(7.46165237939758,-4.45185198378456,-1.32461816282306));
#58062=CARTESIAN_POINT('Ctrl Pts',(6.94809164225473,-4.54138208596012,-2.62194359089516));
#58063=CARTESIAN_POINT('Ctrl Pts',(7.16787076968256,-4.50975040784356,-2.16421694982278));
#58064=CARTESIAN_POINT('Ctrl Pts',(7.33663088231394,-4.4807623507912,-1.73890326423272));
#58065=CARTESIAN_POINT('Ctrl Pts',(7.46165237939758,-4.45185198378456,-1.32461816282306));
#58066=CARTESIAN_POINT('Ctrl Pts',(7.46165237939758,-4.45185198378456,-1.32461816282306));
#58067=CARTESIAN_POINT('Ctrl Pts',(7.36571703908244,-4.4986082311925,-1.29323045524197));
#58068=CARTESIAN_POINT('Ctrl Pts',(7.2697816987673,-4.54536447860044,-1.26184274766089));
#58069=CARTESIAN_POINT('Ctrl Pts',(7.17384635845216,-4.59212072600837,-1.2304550400798));
#58070=CARTESIAN_POINT('Ctrl Pts',(6.99737260418672,-3.35466741224479,-3.46502015180142));
#58071=CARTESIAN_POINT('Ctrl Pts',(6.872142618999,-3.74844825878233,-3.27785823931047));
#58072=CARTESIAN_POINT('Ctrl Pts',(6.69496761793157,-4.16162987061385,-3.08147524771389));
#58073=CARTESIAN_POINT('Ctrl Pts',(6.45213506509495,-4.6201502592847,-2.86354298002157));
#58074=CARTESIAN_POINT('Ctrl Pts',(7.15213252925707,-3.3608045985668,-3.37438271134571));
#58075=CARTESIAN_POINT('Ctrl Pts',(7.02199092199136,-3.76260789239011,-3.18165082839044));
#58076=CARTESIAN_POINT('Ctrl Pts',(6.83894619861565,-4.18135148651518,-2.98049590895782));
#58077=CARTESIAN_POINT('Ctrl Pts',(6.59045151405566,-4.64358926304999,-2.75873759472565));
#58078=CARTESIAN_POINT('Ctrl Pts',(7.30689245432741,-3.3669417848888,-3.28374527089));
#58079=CARTESIAN_POINT('Ctrl Pts',(7.17183922498372,-3.77676752599789,-3.08544341747041));
#58080=CARTESIAN_POINT('Ctrl Pts',(6.98292477929974,-4.20107310241652,-2.87951657020175));
#58081=CARTESIAN_POINT('Ctrl Pts',(6.72876796301637,-4.66702826681527,-2.65393220942972));
#58082=CARTESIAN_POINT('Ctrl Pts',(7.46165237939775,-3.37307897121081,-3.1931078304343));
#58083=CARTESIAN_POINT('Ctrl Pts',(7.32168752797609,-3.79092715960566,-2.98923600655038));
#58084=CARTESIAN_POINT('Ctrl Pts',(7.12690335998383,-4.22079471831786,-2.77853723144567));
#58085=CARTESIAN_POINT('Ctrl Pts',(6.86708441197709,-4.69046727058056,-2.54912682413379));
#58086=CARTESIAN_POINT('',(6.9730266888256,-3.42946788853432,-3.42946788921854));
#58087=CARTESIAN_POINT('Ctrl Pts',(6.49649612061063,-4.53548229371214,-2.9037852073991));
#58088=CARTESIAN_POINT('Ctrl Pts',(6.70189613387517,-4.13912090191365,-3.09217363913432));
#58089=CARTESIAN_POINT('Ctrl Pts',(6.85768162696566,-3.77623926085462,-3.26464932591708));
#58090=CARTESIAN_POINT('Ctrl Pts',(6.97303770582829,-3.42946324032328,-3.42947009812916));
#58091=CARTESIAN_POINT('',(7.17384635845204,-3.36166568592822,-3.36166568592824));
#58092=CARTESIAN_POINT('Ctrl Pts',(6.9730266882762,-3.42946788904522,-3.42946788904572));
#58093=CARTESIAN_POINT('Ctrl Pts',(7.04024193630125,-3.40670199458563,-3.40670199458587));
#58094=CARTESIAN_POINT('Ctrl Pts',(7.10380439458351,-3.3852425489906,-3.38524254899069));
#58095=CARTESIAN_POINT('Ctrl Pts',(7.17384635845203,-3.36166568592823,-3.36166568592825));
#58096=CARTESIAN_POINT('',(7.46165237939775,-3.37307897121081,-3.1931078304343));
#58097=CARTESIAN_POINT('Ctrl Pts',(7.46165237939775,-3.37307897121081,-3.1931078304343));
#58098=CARTESIAN_POINT('Ctrl Pts',(7.36571703908251,-3.36927454278328,-3.24929378226561));
#58099=CARTESIAN_POINT('Ctrl Pts',(7.26978169876727,-3.36547011435575,-3.30547973409693));
#58100=CARTESIAN_POINT('Ctrl Pts',(7.17384635845203,-3.36166568592822,-3.36166568592824));
#58101=CARTESIAN_POINT('Ctrl Pts',(7.46165237939775,-3.37307897121081,-3.1931078304343));
#58102=CARTESIAN_POINT('Ctrl Pts',(7.33663088231331,-3.74631557694812,-3.01100239198735));
#58103=CARTESIAN_POINT('Ctrl Pts',(7.16787076968672,-4.12914206176923,-2.82344994300742));
#58104=CARTESIAN_POINT('Ctrl Pts',(6.94809164225641,-4.54136079998446,-2.62198045928535));
#58105=CARTESIAN_POINT('Origin',(1.5,-2.68986975199945,-4.65899107620573));
#58106=CARTESIAN_POINT('',(6.68133955674308,-2.6898697519964,-4.65899107620051));
#58107=CARTESIAN_POINT('',(6.4964847157299,-2.90378217011975,-4.53548868402102));
#58108=CARTESIAN_POINT('Ctrl Pts',(6.68133955674087,-2.68986975199284,-4.65899107619759));
#58109=CARTESIAN_POINT('Ctrl Pts',(6.67492308098284,-2.69740104160513,-4.65464288223185));
#58110=CARTESIAN_POINT('Ctrl Pts',(6.6685005684247,-2.7049283150624,-4.65029698975985));
#58111=CARTESIAN_POINT('Ctrl Pts',(6.6620720344556,-2.71245153100584,-4.64595341827232));
#58112=CARTESIAN_POINT('Ctrl Pts',(6.6073292890925,-2.77651613682158,-4.6089653539561));
#58113=CARTESIAN_POINT('Ctrl Pts',(6.55213434648286,-2.8403044431865,-4.57213538836558));
#58114=CARTESIAN_POINT('Ctrl Pts',(6.49649612060902,-2.9037852073989,-4.53548229371255));
#58115=CARTESIAN_POINT('',(1.6,-2.90378217011979,-4.53548868402095));
#58116=CARTESIAN_POINT('',(1.5,-2.90378217011979,-4.53548868402095));
#58117=CARTESIAN_POINT('',(1.6,-2.47595733387911,-4.78249346839052));
#58118=CARTESIAN_POINT('',(1.6,-1.35861975199945,-5.42758862206442));
#58119=CARTESIAN_POINT('',(6.49648471573067,-2.47595733387919,-4.78249346839052));
#58120=CARTESIAN_POINT('',(1.5,-2.47595733387911,-4.78249346839052));
#58121=CARTESIAN_POINT('Ctrl Pts',(6.49648471573075,-2.4759573338791,-4.78249346839052));
#58122=CARTESIAN_POINT('Ctrl Pts',(6.55337396234636,-2.5408569710609,-4.7450236453933));
#58123=CARTESIAN_POINT('Ctrl Pts',(6.60979834671127,-2.60607844004607,-4.70736801271777));
#58124=CARTESIAN_POINT('Ctrl Pts',(6.67094806990306,-2.6776801488777,-4.66602874684939));
#58125=CARTESIAN_POINT('Ctrl Pts',(6.67614580655144,-2.68377362961048,-4.66251067410802));
#58126=CARTESIAN_POINT('Ctrl Pts',(6.68133955672777,-2.6898697520092,-4.6589910762001));
#58127=CARTESIAN_POINT('Origin',(1.5,-3.42946788875476,-3.42946788875475));
#58128=CARTESIAN_POINT('Ctrl Pts',(6.97303770557678,-3.4294700977703,-3.42946324107831));
#58129=CARTESIAN_POINT('Ctrl Pts',(6.85768162673857,-3.26464932566841,-3.77623926137783));
#58130=CARTESIAN_POINT('Ctrl Pts',(6.70189613372097,-3.09217363899809,-4.13912090220029));
#58131=CARTESIAN_POINT('Ctrl Pts',(6.49649612060898,-2.90378520739886,-4.53548229371264));
#58132=CARTESIAN_POINT('',(1.6,-3.42946788875476,-3.42946788875475));
#58133=CARTESIAN_POINT('',(1.5,-3.42946788875476,-3.42946788875475));
#58134=CARTESIAN_POINT('',(1.6,-3.45121148122265,-3.38372027838457));
#58135=CARTESIAN_POINT('Ctrl Pts',(6.4521350668314,-2.86354298158031,-4.62015025600519));
#58136=CARTESIAN_POINT('Ctrl Pts',(6.69496761877087,-3.0814752486512,-4.1616298686418));
#58137=CARTESIAN_POINT('Ctrl Pts',(6.87214261929781,-3.27785823975936,-3.74844825783789));
#58138=CARTESIAN_POINT('Ctrl Pts',(6.99737260418699,-3.46502015180182,-3.35466741224394));
#58139=CARTESIAN_POINT('Ctrl Pts',(6.59045151583295,-2.758737596312,-4.64358925974348));
#58140=CARTESIAN_POINT('Ctrl Pts',(6.83894619948317,-2.98049590991796,-4.18135148451713));
#58141=CARTESIAN_POINT('Ctrl Pts',(7.02199092230211,-3.1816508288527,-3.76260789142697));
#58142=CARTESIAN_POINT('Ctrl Pts',(7.15213252925719,-3.3743827113459,-3.3608045985664));
#58143=CARTESIAN_POINT('Ctrl Pts',(6.72876796483449,-2.6539322110437,-4.66702826348176));
#58144=CARTESIAN_POINT('Ctrl Pts',(6.98292478019547,-2.87951657118472,-4.20107310039245));
#58145=CARTESIAN_POINT('Ctrl Pts',(7.17183922530641,-3.08544341794604,-3.77676752501605));
#58146=CARTESIAN_POINT('Ctrl Pts',(7.30689245432738,-3.28374527088997,-3.36694178488886));
#58147=CARTESIAN_POINT('Ctrl Pts',(6.86708441383603,-2.54912682577539,-4.69046726722004));
#58148=CARTESIAN_POINT('Ctrl Pts',(7.12690336090776,-2.77853723245148,-4.22079471626778));
#58149=CARTESIAN_POINT('Ctrl Pts',(7.3216875283107,-2.98923600703938,-3.79092715860513));
#58150=CARTESIAN_POINT('Ctrl Pts',(7.46165237939758,-3.19310783043405,-3.37307897121132));
#58151=CARTESIAN_POINT('',(6.94805436450009,-2.62196828737528,-4.54138228956758));
#58152=CARTESIAN_POINT('Ctrl Pts',(6.68133955674308,-2.68986975199337,-4.65899107619527));
#58153=CARTESIAN_POINT('Ctrl Pts',(6.76807293638611,-2.6676651885047,-4.62053164407294));
#58154=CARTESIAN_POINT('Ctrl Pts',(6.85888711552652,-2.64454495411987,-4.5804862234352));
#58155=CARTESIAN_POINT('Ctrl Pts',(6.94805436450009,-2.62196828737528,-4.54138228956758));
#58156=CARTESIAN_POINT('',(7.46165237939758,-3.19310783043405,-3.37307897121132));
#58157=CARTESIAN_POINT('Ctrl Pts',(6.94809164225473,-2.62198045928545,-4.54136079998506));
#58158=CARTESIAN_POINT('Ctrl Pts',(7.16787076968256,-2.82344994300837,-4.12914206176917));
#58159=CARTESIAN_POINT('Ctrl Pts',(7.33663088231394,-3.0110023919897,-3.74631557694482));
#58160=CARTESIAN_POINT('Ctrl Pts',(7.46165237939758,-3.19310783043405,-3.37307897121132));
#58161=CARTESIAN_POINT('Ctrl Pts',(7.46165237939758,-3.19310783043405,-3.37307897121132));
#58162=CARTESIAN_POINT('Ctrl Pts',(7.36571703908244,-3.2492937822655,-3.36927454278351));
#58163=CARTESIAN_POINT('Ctrl Pts',(7.26978169876729,-3.30547973409695,-3.3654701143557));
#58164=CARTESIAN_POINT('Ctrl Pts',(7.17384635845215,-3.36166568592839,-3.36166568592789));
#58165=CARTESIAN_POINT('Ctrl Pts',(6.99737260418672,-1.17271712435108,-4.67812918220743));
#58166=CARTESIAN_POINT('Ctrl Pts',(6.872142618999,-1.60732229722181,-4.71293263463817));
#58167=CARTESIAN_POINT('Ctrl Pts',(6.69496761793157,-2.06333956524279,-4.7494507809601));
#58168=CARTESIAN_POINT('Ctrl Pts',(6.45213506509495,-2.56939600383103,-4.78997609516963));
#58169=CARTESIAN_POINT('Ctrl Pts',(7.15213252925706,-1.22335080384155,-4.6027034493998));
#58170=CARTESIAN_POINT('Ctrl Pts',(7.02199092199136,-1.66768860509444,-4.63669438955298));
#58171=CARTESIAN_POINT('Ctrl Pts',(6.83894619861566,-2.13090865499507,-4.67186091629066));
#58172=CARTESIAN_POINT('Ctrl Pts',(6.59045151405566,-2.64209746917913,-4.71093147093258));
#58173=CARTESIAN_POINT('Ctrl Pts',(7.30689245432741,-1.27398448333202,-4.52727771659216));
#58174=CARTESIAN_POINT('Ctrl Pts',(7.17183922498372,-1.72805491296707,-4.56045614446779));
#58175=CARTESIAN_POINT('Ctrl Pts',(6.98292477929975,-2.19847774474734,-4.59427105162121));
#58176=CARTESIAN_POINT('Ctrl Pts',(6.72876796301638,-2.71479893452723,-4.63188684669553));
#58177=CARTESIAN_POINT('Ctrl Pts',(7.46165237939775,-1.32461816282249,-4.45185198378452));
#58178=CARTESIAN_POINT('Ctrl Pts',(7.32168752797609,-1.7884212208397,-4.48421789938261));
#58179=CARTESIAN_POINT('Ctrl Pts',(7.12690335998383,-2.26604683449962,-4.51668118695177));
#58180=CARTESIAN_POINT('Ctrl Pts',(6.86708441197709,-2.78750039987533,-4.55284222245849));
#58181=CARTESIAN_POINT('',(6.9730266888256,-1.25527236832443,-4.68474025779341));
#58182=CARTESIAN_POINT('Ctrl Pts',(6.49649612061064,-2.47595028106968,-4.78249290359715));
#58183=CARTESIAN_POINT('Ctrl Pts',(6.70189613387518,-2.03849703082522,-4.74746137535973));
#58184=CARTESIAN_POINT('Ctrl Pts',(6.85768162696566,-1.63799446770973,-4.71538888111925));
#58185=CARTESIAN_POINT('Ctrl Pts',(6.97303770582829,-1.25526723840028,-4.68473984666061));
#58186=CARTESIAN_POINT('',(7.17384635845203,-1.23045504008016,-4.59212072600842));
#58187=CARTESIAN_POINT('Ctrl Pts',(6.9730266882762,-1.2552723688533,-4.6847402578992));
#58188=CARTESIAN_POINT('Ctrl Pts',(7.04024207626698,-1.24693945578933,-4.65364140296871));
#58189=CARTESIAN_POINT('Ctrl Pts',(7.10380410094959,-1.23908480708055,-4.62432745491155));
#58190=CARTESIAN_POINT('Ctrl Pts',(7.17384635845203,-1.23045504008016,-4.59212072600842));
#58191=CARTESIAN_POINT('',(7.46165237939775,-1.32461816282249,-4.45185198378452));
#58192=CARTESIAN_POINT('Ctrl Pts',(7.46165237939775,-1.32461816282249,-4.45185198378452));
#58193=CARTESIAN_POINT('Ctrl Pts',(7.36571703908251,-1.29323045524171,-4.49860823119249));
#58194=CARTESIAN_POINT('Ctrl Pts',(7.26978169876727,-1.26184274766094,-4.54536447860045));
#58195=CARTESIAN_POINT('Ctrl Pts',(7.17384635845203,-1.23045504008016,-4.59212072600842));
#58196=CARTESIAN_POINT('Ctrl Pts',(7.46165237939775,-1.32461816282249,-4.45185198378452));
#58197=CARTESIAN_POINT('Ctrl Pts',(7.33663088231331,-1.73890326423675,-4.48076235079082));
#58198=CARTESIAN_POINT('Ctrl Pts',(7.16787076968672,-2.1642169498233,-4.50975040784277));
#58199=CARTESIAN_POINT('Ctrl Pts',(6.94809164225641,-2.62194359089469,-4.54138208595974));
#58200=CARTESIAN_POINT('Origin',(1.5,-4.33680868994202E-16,-5.37973950399889));
#58201=CARTESIAN_POINT('',(6.68133955674307,2.69770838383767E-14,-5.37973950399284));
#58202=CARTESIAN_POINT('',(6.4964847157299,-0.247004784369499,-5.37973950399894));
#58203=CARTESIAN_POINT('Ctrl Pts',(6.68133955674087,1.65339963942301E-12,
-5.37973950398854));
#58204=CARTESIAN_POINT('Ctrl Pts',(6.67492308098284,-0.00869638510872275,
-5.37973950235977));
#58205=CARTESIAN_POINT('Ctrl Pts',(6.6685005684247,-0.0173881413799495,
-5.37973948580553));
#58206=CARTESIAN_POINT('Ctrl Pts',(6.6620720344556,-0.026075223248889,-5.3797394505259));
#58207=CARTESIAN_POINT('Ctrl Pts',(6.6073292890925,-0.100050831526873,-5.37973915009911));
#58208=CARTESIAN_POINT('Ctrl Pts',(6.55213434648286,-0.173708108098531,
-5.37973761745967));
#58209=CARTESIAN_POINT('Ctrl Pts',(6.49649612060902,-0.247010609884638,
-5.37973548846904));
#58210=CARTESIAN_POINT('',(1.6,-0.247004784369567,-5.37973950399889));
#58211=CARTESIAN_POINT('',(1.5,-0.247004784369567,-5.37973950399889));
#58212=CARTESIAN_POINT('',(1.6,0.247004784369567,-5.37973950399889));
#58213=CARTESIAN_POINT('',(1.6,1.77500000000001,-5.37973950399889));
#58214=CARTESIAN_POINT('',(6.49648471573067,0.2470047843695,-5.37973950399894));
#58215=CARTESIAN_POINT('',(1.5,0.247004784369566,-5.37973950399889));
#58216=CARTESIAN_POINT('Ctrl Pts',(6.49648471573075,0.247004784369566,-5.37973950399889));
#58217=CARTESIAN_POINT('Ctrl Pts',(6.55337396234641,0.17206513837507,-5.37973950399889));
#58218=CARTESIAN_POINT('Ctrl Pts',(6.60979834671137,0.096753873023939,-5.37973950399889));
#58219=CARTESIAN_POINT('Ctrl Pts',(6.67094806990306,0.014075341287303,-5.37973950399889));
#58220=CARTESIAN_POINT('Ctrl Pts',(6.67614580655144,0.00703919580456425,
-5.37973950399889));
#58221=CARTESIAN_POINT('Ctrl Pts',(6.68133955672777,-1.12616947017807E-11,
-5.37973950399889));
#58222=CARTESIAN_POINT('Origin',(1.5,-1.25527236874722,-4.68474025750198));
#58223=CARTESIAN_POINT('Ctrl Pts',(6.97303770557678,-1.25527660564903,-4.68473733700388));
#58224=CARTESIAN_POINT('Ctrl Pts',(6.85768162673857,-0.939149619787657,
-4.90264379395559));
#58225=CARTESIAN_POINT('Ctrl Pts',(6.70189613372097,-0.608340473184771,
-5.13067067013966));
#58226=CARTESIAN_POINT('Ctrl Pts',(6.49649612060898,-0.247010609884559,
-5.37973548846909));
#58227=CARTESIAN_POINT('',(1.6,-1.25527236874722,-4.68474025750198));
#58228=CARTESIAN_POINT('',(1.5,-1.25527236874722,-4.68474025750198));
#58229=CARTESIAN_POINT('',(1.6,-0.721057192610576,-5.05297499065702));
#58230=CARTESIAN_POINT('Ctrl Pts',(6.45213506683129,-0.169825838874386,
-5.43293898179197));
#58231=CARTESIAN_POINT('Ctrl Pts',(6.69496761877081,-0.587820912143882,
-5.14481481171758));
#58232=CARTESIAN_POINT('Ctrl Pts',(6.87214261929779,-0.964484376716746,
-4.88518053593886));
#58233=CARTESIAN_POINT('Ctrl Pts',(6.99737260418699,-1.32346176996341,-4.63773727615197));
#58234=CARTESIAN_POINT('Ctrl Pts',(6.59045151583283,-0.0673422109094755,
-5.40083506183456));
#58235=CARTESIAN_POINT('Ctrl Pts',(6.83894619948311,-0.490509431605879,
-5.11140456270267));
#58236=CARTESIAN_POINT('Ctrl Pts',(7.02199092230209,-0.874086498044708,
-4.84933943288195));
#58237=CARTESIAN_POINT('Ctrl Pts',(7.15213252925719,-1.24189885083336,-4.59773351518701));
#58238=CARTESIAN_POINT('Ctrl Pts',(6.72876796483437,0.0351414170554353,
-5.36873114187716));
#58239=CARTESIAN_POINT('Ctrl Pts',(6.98292478019541,-0.393197951067876,
-5.07799431368776));
#58240=CARTESIAN_POINT('Ctrl Pts',(7.17183922530639,-0.783688619372669,
-4.81349832982504));
#58241=CARTESIAN_POINT('Ctrl Pts',(7.30689245432738,-1.1603359317033,-4.55772975422206));
#58242=CARTESIAN_POINT('Ctrl Pts',(6.86708441383591,0.137625045020346,-5.33662722191976));
#58243=CARTESIAN_POINT('Ctrl Pts',(7.1269033609077,-0.295886470529872,-5.04458406467285));
#58244=CARTESIAN_POINT('Ctrl Pts',(7.32168752831068,-0.693290740700631,
-4.77765722676813));
#58245=CARTESIAN_POINT('Ctrl Pts',(7.46165237939758,-1.07877301257324,-4.51772599325711));
#58246=CARTESIAN_POINT('',(6.94805436450009,-3.784472735191E-13,-5.2439365747499));
#58247=CARTESIAN_POINT('Ctrl Pts',(6.68133955674307,2.77425651895591E-14,
-5.37973950398679));
#58248=CARTESIAN_POINT('Ctrl Pts',(6.76807250396894,-2.90644853604443E-15,
-5.33533059841514));
#58249=CARTESIAN_POINT('Ctrl Pts',(6.85888652980292,-1.57039519055847E-13,
-5.28909020484357));
#58250=CARTESIAN_POINT('Ctrl Pts',(6.94805436450009,-3.78239106701983E-13,
-5.2439365747499));
#58251=CARTESIAN_POINT('',(7.46165237939758,-1.07877301257324,-4.51772599325711));
#58252=CARTESIAN_POINT('Ctrl Pts',(6.94809164225473,-2.12859750598534E-5,
-5.24392405018061));
#58253=CARTESIAN_POINT('Ctrl Pts',(7.16787076968256,-0.380608346074385,
-4.98766689283114));
#58254=CARTESIAN_POINT('Ctrl Pts',(7.33663088231394,-0.734446773846379,
-4.74990565622242));
#58255=CARTESIAN_POINT('Ctrl Pts',(7.46165237939758,-1.07877301257324,-4.51772599325711));
#58256=CARTESIAN_POINT('Ctrl Pts',(7.46165237939758,-1.07877301257324,-4.51772599325711));
#58257=CARTESIAN_POINT('Ctrl Pts',(7.36571703908244,-1.12933368840899,-4.54252423750747));
#58258=CARTESIAN_POINT('Ctrl Pts',(7.26978169876729,-1.17989436424473,-4.56732248175783));
#58259=CARTESIAN_POINT('Ctrl Pts',(7.17384635845214,-1.23045504008048,-4.5921207260082));
#58260=CARTESIAN_POINT('Ctrl Pts',(6.99737260418672,1.32346176996264,-4.6377372761525));
#58261=CARTESIAN_POINT('Ctrl Pts',(6.872142618999,0.964484375855836,-4.88518053653228));
#58262=CARTESIAN_POINT('Ctrl Pts',(6.69496761793157,0.587820910346253,-5.14481481295668));
#58263=CARTESIAN_POINT('Ctrl Pts',(6.45213506509495,0.169825835884926,-5.4329389838526));
#58264=CARTESIAN_POINT('Ctrl Pts',(7.15213252925707,1.241898850833,-4.59773351518726));
#58265=CARTESIAN_POINT('Ctrl Pts',(7.02199092199136,0.874086497162872,-4.84933943348488));
#58266=CARTESIAN_POINT('Ctrl Pts',(6.83894619861566,0.49050942977547,-5.11140456395288));
#58267=CARTESIAN_POINT('Ctrl Pts',(6.59045151405566,0.067342207882593,-5.40083506390477));
#58268=CARTESIAN_POINT('Ctrl Pts',(7.30689245432741,1.16033593170335,-4.55772975422203));
#58269=CARTESIAN_POINT('Ctrl Pts',(7.17183922498372,0.783688618469905,-4.81349833043748));
#58270=CARTESIAN_POINT('Ctrl Pts',(6.98292477929975,0.393197949204688,-5.07799431494909));
#58271=CARTESIAN_POINT('Ctrl Pts',(6.72876796301638,-0.0351414201197403,
-5.36873114395694));
#58272=CARTESIAN_POINT('Ctrl Pts',(7.46165237939775,1.07877301257371,-4.51772599325679));
#58273=CARTESIAN_POINT('Ctrl Pts',(7.32168752797609,0.693290739776941,-4.77765722739008));
#58274=CARTESIAN_POINT('Ctrl Pts',(7.12690335998383,0.295886468633904,-5.04458406594529));
#58275=CARTESIAN_POINT('Ctrl Pts',(6.86708441197709,-0.137625048122074,
-5.33662722400912));
#58276=CARTESIAN_POINT('Ctrl Pts',(6.49649612061064,0.247010609885015,-5.37973548846878));
#58277=CARTESIAN_POINT('Ctrl Pts',(6.70189613387518,0.608340473446072,-5.13067066995954));
#58278=CARTESIAN_POINT('Ctrl Pts',(6.85768162696567,0.939149620264625,-4.90264379362682));
#58279=CARTESIAN_POINT('Ctrl Pts',(6.97303770582829,1.25527660633732,-4.68473733652944));
#58280=CARTESIAN_POINT('',(7.46165237939775,1.07877301257371,-4.51772599325679));
#58281=CARTESIAN_POINT('Ctrl Pts',(7.46165237939775,1.07877301257371,-4.51772599325679));
#58282=CARTESIAN_POINT('Ctrl Pts',(7.36571703908251,1.1293336884092,-4.54252423750733));
#58283=CARTESIAN_POINT('Ctrl Pts',(7.26978169876728,1.17989436424469,-4.56732248175787));
#58284=CARTESIAN_POINT('Ctrl Pts',(7.17384635845204,1.23045504008019,-4.59212072600841));
#58285=CARTESIAN_POINT('Ctrl Pts',(7.46165237939775,1.07877301257371,-4.51772599325679));
#58286=CARTESIAN_POINT('Ctrl Pts',(7.33663088231331,0.734446773842696,-4.7499056562241));
#58287=CARTESIAN_POINT('Ctrl Pts',(7.16787076968672,0.380608346073537,-4.98766689283072));
#58288=CARTESIAN_POINT('Ctrl Pts',(6.94809164225642,2.12859752740831E-5,
-5.24392405018004));
#58289=CARTESIAN_POINT('Ctrl Pts',(7.17384635845215,4.5921207260082,-1.23045504008048));
#58290=CARTESIAN_POINT('Ctrl Pts',(7.18694338462328,4.56684952841756,-1.26742353917928));
#58291=CARTESIAN_POINT('Ctrl Pts',(7.1999334636683,4.5414911822982,-1.30436927548241));
#58292=CARTESIAN_POINT('Ctrl Pts',(7.21281435373034,4.51604216132286,-1.3412906003674));
#58293=CARTESIAN_POINT('Ctrl Pts',(7.26978169876729,4.56732248175783,-1.17989436424473));
#58294=CARTESIAN_POINT('Ctrl Pts',(7.28299669995037,4.54214834917584,-1.2168886144726));
#58295=CARTESIAN_POINT('Ctrl Pts',(7.29604661499973,4.5168396920471,-1.25384772750637));
#58296=CARTESIAN_POINT('Ctrl Pts',(7.30892798333169,4.4913910670488,-1.29076915849307));
#58297=CARTESIAN_POINT('Ctrl Pts',(7.36571703908244,4.54252423750747,-1.12933368840899));
#58298=CARTESIAN_POINT('Ctrl Pts',(7.37905001527745,4.51744716993412,-1.16635368976592));
#58299=CARTESIAN_POINT('Ctrl Pts',(7.39215976633117,4.49218820179599,-1.20332617953033));
#58300=CARTESIAN_POINT('Ctrl Pts',(7.40504161293303,4.46673997277473,-1.24024771661874));
#58301=CARTESIAN_POINT('Ctrl Pts',(7.46165237939758,4.51772599325711,-1.07877301257324));
#58302=CARTESIAN_POINT('Ctrl Pts',(7.47510333060454,4.49274599069239,-1.11581876505924));
#58303=CARTESIAN_POINT('Ctrl Pts',(7.4882729176626,4.46753671154489,-1.15280463155429));
#58304=CARTESIAN_POINT('Ctrl Pts',(7.50115524253438,4.44208887850067,-1.18972627474441));
#58305=CARTESIAN_POINT('',(7.49999999999943,4.44436879421757,-1.18641730474065));
#58306=CARTESIAN_POINT('Ctrl Pts',(7.46165237939758,4.51772599325711,-1.07877301257324));
#58307=CARTESIAN_POINT('Ctrl Pts',(7.47470152024065,4.49349219992073,-1.11471212456534));
#58308=CARTESIAN_POINT('Ctrl Pts',(7.48748585582712,4.46904262342728,-1.15059487498735));
#58309=CARTESIAN_POINT('Ctrl Pts',(7.50000000105064,4.44436879327734,-1.18641730372583));
#58310=CARTESIAN_POINT('',(7.49999999999233,4.44238517355639,-1.19033351972209));
#58311=CARTESIAN_POINT('Ctrl Pts',(7.50000000105118,4.44436879327628,-1.18641730372738));
#58312=CARTESIAN_POINT('Ctrl Pts',(7.50000000037148,4.4437079306274,-1.18772277427295));
#58313=CARTESIAN_POINT('Ctrl Pts',(7.49999999647595,4.44304672983401,-1.18902817040918));
#58314=CARTESIAN_POINT('Ctrl Pts',(7.49999999999096,4.44238517355376,-1.19033351972076));
#58315=CARTESIAN_POINT('Ctrl Pts',(7.17384635845215,4.5921207260082,-1.23045504008048));
#58316=CARTESIAN_POINT('Ctrl Pts',(7.19420569065385,4.58275691773915,-1.22794601521635));
#58317=CARTESIAN_POINT('Ctrl Pts',(7.21511409889777,4.57315172570485,-1.22537230751382));
#58318=CARTESIAN_POINT('Ctrl Pts',(7.23681946879609,4.56318819945531,-1.22270258210925));
#58319=CARTESIAN_POINT('Ctrl Pts',(7.32484115407359,4.52278315794258,-1.2118760571323));
#58320=CARTESIAN_POINT('Ctrl Pts',(7.41251895869389,4.48265795751599,-1.20112457966125));
#58321=CARTESIAN_POINT('Ctrl Pts',(7.49999999999091,4.44238517355351,-1.19033351972131));
#58322=CARTESIAN_POINT('Ctrl Pts',(7.17384635845215,3.36166568592789,-3.3616656859284));
#58323=CARTESIAN_POINT('Ctrl Pts',(7.18694338462328,3.32129593728095,-3.38104574649242));
#58324=CARTESIAN_POINT('Ctrl Pts',(7.1999334636683,3.28086209719206,-3.40036251963277));
#58325=CARTESIAN_POINT('Ctrl Pts',(7.21281435373034,3.24036193608348,-3.41961281443688));
#58326=CARTESIAN_POINT('Ctrl Pts',(7.26978169876729,3.3654701143557,-3.30547973409695));
#58327=CARTESIAN_POINT('Ctrl Pts',(7.28299669995037,3.32517155090753,-3.32493062829724));
#58328=CARTESIAN_POINT('Ctrl Pts',(7.29604661499973,3.28477405438148,-3.34428383052146));
#58329=CARTESIAN_POINT('Ctrl Pts',(7.30892798333169,3.24427418314822,-3.36353441520086));
#58330=CARTESIAN_POINT('Ctrl Pts',(7.36571703908244,3.36927454278351,-3.2492937822655));
#58331=CARTESIAN_POINT('Ctrl Pts',(7.37905001527745,3.3290471645341,-3.26881551010206));
#58332=CARTESIAN_POINT('Ctrl Pts',(7.39215976633117,3.2886860115709,-3.28820514141014));
#58333=CARTESIAN_POINT('Ctrl Pts',(7.40504161293303,3.24818643021297,-3.30745601596484));
#58334=CARTESIAN_POINT('Ctrl Pts',(7.46165237939758,3.37307897121132,-3.19310783043405));
#58335=CARTESIAN_POINT('Ctrl Pts',(7.47510333060454,3.33292277816068,-3.21270039190688));
#58336=CARTESIAN_POINT('Ctrl Pts',(7.4882729176626,3.29259796876032,-3.23212645229882));
#58337=CARTESIAN_POINT('Ctrl Pts',(7.50115524253438,3.25209867727771,-3.25137761672882));
#58338=CARTESIAN_POINT('',(7.49999999999943,3.25572762720891,-3.24965192250366));
#58339=CARTESIAN_POINT('Ctrl Pts',(7.46165237939758,3.37307897121132,-3.19310783043405));
#58340=CARTESIAN_POINT('Ctrl Pts',(7.47470152024065,3.3341223345559,-3.21211511774048));
#58341=CARTESIAN_POINT('Ctrl Pts',(7.48748585582712,3.2950070049898,-3.23096570291687));
#58342=CARTESIAN_POINT('Ctrl Pts',(7.50000000105064,3.25572762690205,-3.24965192115468));
#58343=CARTESIAN_POINT('',(7.49999999999233,3.25205165383413,-3.25205165383366));
#58344=CARTESIAN_POINT('Ctrl Pts',(7.50000000105118,3.25572762690036,-3.24965192115549));
#58345=CARTESIAN_POINT('Ctrl Pts',(7.50000000037148,3.25450256807911,-3.25045206029546));
#58346=CARTESIAN_POINT('Ctrl Pts',(7.49999999647522,3.25327725332823,-3.25125196611448));
#58347=CARTESIAN_POINT('Ctrl Pts',(7.49999999999096,3.25205165383252,-3.2520516538312));
#58348=CARTESIAN_POINT('Ctrl Pts',(7.17384635845215,3.36166568592789,-3.36166568592839));
#58349=CARTESIAN_POINT('Ctrl Pts',(7.19420493717887,3.35481115621029,-3.35481115621029));
#58350=CARTESIAN_POINT('Ctrl Pts',(7.21511249441196,3.3477799556656,-3.34777994985528));
#58351=CARTESIAN_POINT('Ctrl Pts',(7.23681685935962,3.34048648878989,-3.34048647397502));
#58352=CARTESIAN_POINT('Ctrl Pts',(7.32483941486432,3.31090766469447,-3.31090761336144));
#58353=CARTESIAN_POINT('Ctrl Pts',(7.41251809600273,3.28153366858765,-3.28153366858751));
#58354=CARTESIAN_POINT('Ctrl Pts',(7.49999999999091,3.25205165383202,-3.25205165383156));
#58355=CARTESIAN_POINT('Ctrl Pts',(7.17384635845215,1.2304550400798,-4.59212072600838));
#58356=CARTESIAN_POINT('Ctrl Pts',(7.18694338462328,1.18580378192515,-4.58871947646023));
#58357=CARTESIAN_POINT('Ctrl Pts',(7.1999334636683,1.14112866266543,-4.58523137267447));
#58358=CARTESIAN_POINT('Ctrl Pts',(7.21281435373034,1.09642934688599,-4.58165253645088));
#58359=CARTESIAN_POINT('Ctrl Pts',(7.26978169876729,1.26184274766089,-4.54536447860044));
#58360=CARTESIAN_POINT('Ctrl Pts',(7.28299669995037,1.21721772087861,-4.54206016538013));
#58361=CARTESIAN_POINT('Ctrl Pts',(7.29604661499973,1.17255586152565,-4.53862178188785));
#58362=CARTESIAN_POINT('Ctrl Pts',(7.30892798333169,1.12785665184795,-4.53504334164129));
#58363=CARTESIAN_POINT('Ctrl Pts',(7.36571703908244,1.29323045524197,-4.4986082311925));
#58364=CARTESIAN_POINT('Ctrl Pts',(7.37905001527745,1.24863165983206,-4.49540085430002));
#58365=CARTESIAN_POINT('Ctrl Pts',(7.39215976633117,1.20398306038586,-4.49201219110123));
#58366=CARTESIAN_POINT('Ctrl Pts',(7.40504161293303,1.15928395680991,-4.4884341468317));
#58367=CARTESIAN_POINT('Ctrl Pts',(7.46165237939758,1.32461816282306,-4.45185198378456));
#58368=CARTESIAN_POINT('Ctrl Pts',(7.47510333060454,1.28004559878552,-4.44874154321992));
#58369=CARTESIAN_POINT('Ctrl Pts',(7.4882729176626,1.23541025924608,-4.44540260031461));
#58370=CARTESIAN_POINT('Ctrl Pts',(7.50115524253438,1.19071126177187,-4.44182495202211));
#58371=CARTESIAN_POINT('',(7.49999999999943,1.19471687171392,-4.44214493194956));
#58372=CARTESIAN_POINT('Ctrl Pts',(7.46165237939758,1.32461816282306,-4.45185198378456));
#58373=CARTESIAN_POINT('Ctrl Pts',(7.47470152024064,1.28137708218025,-4.44883445912125));
#58374=CARTESIAN_POINT('Ctrl Pts',(7.48748585582712,1.23807692051041,-4.44560187997715));
#58375=CARTESIAN_POINT('Ctrl Pts',(7.50000000105064,1.19471687212266,-4.44214493062788));
#58376=CARTESIAN_POINT('',(7.49999999999226,1.19033351972273,-4.44238517355628));
#58377=CARTESIAN_POINT('Ctrl Pts',(7.50000000105118,1.19471687212079,-4.44214493062773));
#58378=CARTESIAN_POINT('Ctrl Pts',(7.50000000037148,1.19325587076909,-4.44222534202356));
#58379=CARTESIAN_POINT('Ctrl Pts',(7.49999999647456,1.19179476415888,-4.4423054234084));
#58380=CARTESIAN_POINT('Ctrl Pts',(7.49999999999088,1.19033351972257,-4.44238517355332));
#58381=CARTESIAN_POINT('Ctrl Pts',(7.17384635845215,1.2304550400798,-4.59212072600838));
#58382=CARTESIAN_POINT('Ctrl Pts',(7.1943969563607,1.22792244418713,-4.58266894946054));
#58383=CARTESIAN_POINT('Ctrl Pts',(7.21552165468888,1.22532214675418,-4.57296449112453));
#58384=CARTESIAN_POINT('Ctrl Pts',(7.23748292043925,1.22262099986246,-4.56288364865534));
#58385=CARTESIAN_POINT('Ctrl Pts',(7.32528335544088,1.21182190135913,-4.52258076429347));
#58386=CARTESIAN_POINT('Ctrl Pts',(7.41273830259814,1.20109752290511,-4.48255698032661));
#58387=CARTESIAN_POINT('Ctrl Pts',(7.49999999999083,1.19033351972196,-4.44238517355338));
#58388=CARTESIAN_POINT('Ctrl Pts',(7.17384635845214,-1.23045504008048,-4.5921207260082));
#58389=CARTESIAN_POINT('Ctrl Pts',(7.18694338462328,-1.26742353917928,-4.56684952841756));
#58390=CARTESIAN_POINT('Ctrl Pts',(7.1999334636683,-1.30436927548242,-4.5414911822982));
#58391=CARTESIAN_POINT('Ctrl Pts',(7.21281435373034,-1.3412906003674,-4.51604216132286));
#58392=CARTESIAN_POINT('Ctrl Pts',(7.26978169876729,-1.17989436424474,-4.56732248175783));
#58393=CARTESIAN_POINT('Ctrl Pts',(7.28299669995036,-1.2168886144726,-4.54214834917584));
#58394=CARTESIAN_POINT('Ctrl Pts',(7.29604661499973,-1.25384772750638,-4.5168396920471));
#58395=CARTESIAN_POINT('Ctrl Pts',(7.30892798333169,-1.29076915849307,-4.4913910670488));
#58396=CARTESIAN_POINT('Ctrl Pts',(7.36571703908244,-1.12933368840899,-4.54252423750747));
#58397=CARTESIAN_POINT('Ctrl Pts',(7.37905001527745,-1.16635368976592,-4.51744716993412));
#58398=CARTESIAN_POINT('Ctrl Pts',(7.39215976633117,-1.20332617953033,-4.49218820179599));
#58399=CARTESIAN_POINT('Ctrl Pts',(7.40504161293303,-1.24024771661874,-4.46673997277473));
#58400=CARTESIAN_POINT('Ctrl Pts',(7.46165237939758,-1.07877301257324,-4.51772599325711));
#58401=CARTESIAN_POINT('Ctrl Pts',(7.47510333060454,-1.11581876505924,-4.49274599069239));
#58402=CARTESIAN_POINT('Ctrl Pts',(7.4882729176626,-1.15280463155429,-4.46753671154489));
#58403=CARTESIAN_POINT('Ctrl Pts',(7.50115524253438,-1.18972627474441,-4.44208887850067));
#58404=CARTESIAN_POINT('',(7.49999999999943,-1.18641730474065,-4.44436879421757));
#58405=CARTESIAN_POINT('Ctrl Pts',(7.46165237939758,-1.07877301257324,-4.51772599325711));
#58406=CARTESIAN_POINT('Ctrl Pts',(7.47470152024065,-1.11471212456534,-4.49349219992073));
#58407=CARTESIAN_POINT('Ctrl Pts',(7.48748585582712,-1.15059487498735,-4.46904262342728));
#58408=CARTESIAN_POINT('Ctrl Pts',(7.50000000105064,-1.18641730372583,-4.44436879327734));
#58409=CARTESIAN_POINT('',(7.49999999999234,-1.19033351972209,-4.44238517355638));
#58410=CARTESIAN_POINT('Ctrl Pts',(7.50000000105118,-1.18641730372738,-4.44436879327628));
#58411=CARTESIAN_POINT('Ctrl Pts',(7.50000000037148,-1.18772277427295,-4.4437079306274));
#58412=CARTESIAN_POINT('Ctrl Pts',(7.49999999647595,-1.18902817040918,-4.44304672983401));
#58413=CARTESIAN_POINT('Ctrl Pts',(7.49999999999097,-1.19033351972076,-4.44238517355376));
#58414=CARTESIAN_POINT('Ctrl Pts',(7.17384635845214,-1.23045504008048,-4.5921207260082));
#58415=CARTESIAN_POINT('Ctrl Pts',(7.19420569065388,-1.22794601521634,-4.58275691773914));
#58416=CARTESIAN_POINT('Ctrl Pts',(7.2151140988978,-1.22537230751381,-4.57315172570483));
#58417=CARTESIAN_POINT('Ctrl Pts',(7.23681946879609,-1.22270258210925,-4.56318819945531));
#58418=CARTESIAN_POINT('Ctrl Pts',(7.32484115407349,-1.21187605713231,-4.52278315794262));
#58419=CARTESIAN_POINT('Ctrl Pts',(7.41251895869389,-1.20112457966125,-4.48265795751599));
#58420=CARTESIAN_POINT('Ctrl Pts',(7.49999999999091,-1.19033351972132,-4.44238517355351));
#58421=CARTESIAN_POINT('Ctrl Pts',(7.17384635845214,-3.3616656859284,-3.36166568592789));
#58422=CARTESIAN_POINT('Ctrl Pts',(7.18694338462328,-3.38104574649242,-3.32129593728095));
#58423=CARTESIAN_POINT('Ctrl Pts',(7.1999334636683,-3.40036251963277,-3.28086209719206));
#58424=CARTESIAN_POINT('Ctrl Pts',(7.21281435373034,-3.41961281443688,-3.24036193608348));
#58425=CARTESIAN_POINT('Ctrl Pts',(7.26978169876729,-3.30547973409695,-3.3654701143557));
#58426=CARTESIAN_POINT('Ctrl Pts',(7.28299669995036,-3.32493062829724,-3.32517155090753));
#58427=CARTESIAN_POINT('Ctrl Pts',(7.29604661499973,-3.34428383052145,-3.28477405438148));
#58428=CARTESIAN_POINT('Ctrl Pts',(7.30892798333169,-3.36353441520086,-3.24427418314822));
#58429=CARTESIAN_POINT('Ctrl Pts',(7.36571703908244,-3.2492937822655,-3.36927454278351));
#58430=CARTESIAN_POINT('Ctrl Pts',(7.37905001527745,-3.26881551010206,-3.3290471645341));
#58431=CARTESIAN_POINT('Ctrl Pts',(7.39215976633117,-3.28820514141014,-3.2886860115709));
#58432=CARTESIAN_POINT('Ctrl Pts',(7.40504161293303,-3.30745601596484,-3.24818643021296));
#58433=CARTESIAN_POINT('Ctrl Pts',(7.46165237939758,-3.19310783043405,-3.37307897121132));
#58434=CARTESIAN_POINT('Ctrl Pts',(7.47510333060454,-3.21270039190688,-3.33292277816068));
#58435=CARTESIAN_POINT('Ctrl Pts',(7.4882729176626,-3.23212645229882,-3.29259796876032));
#58436=CARTESIAN_POINT('Ctrl Pts',(7.50115524253438,-3.25137761672881,-3.25209867727771));
#58437=CARTESIAN_POINT('',(7.49999999999943,-3.24965192250366,-3.25572762720891));
#58438=CARTESIAN_POINT('Ctrl Pts',(7.46165237939758,-3.19310783043405,-3.37307897121132));
#58439=CARTESIAN_POINT('Ctrl Pts',(7.47470152024064,-3.21211511774048,-3.3341223345559));
#58440=CARTESIAN_POINT('Ctrl Pts',(7.48748585582712,-3.23096570291687,-3.2950070049898));
#58441=CARTESIAN_POINT('Ctrl Pts',(7.50000000105064,-3.24965192115468,-3.25572762690205));
#58442=CARTESIAN_POINT('',(7.49999999999234,-3.25205165383366,-3.25205165383413));
#58443=CARTESIAN_POINT('Ctrl Pts',(7.50000000105118,-3.24965192115548,-3.25572762690036));
#58444=CARTESIAN_POINT('Ctrl Pts',(7.50000000037147,-3.25045206029546,-3.25450256807912));
#58445=CARTESIAN_POINT('Ctrl Pts',(7.49999999647523,-3.25125196611448,-3.25327725332823));
#58446=CARTESIAN_POINT('Ctrl Pts',(7.49999999999097,-3.2520516538312,-3.25205165383252));
#58447=CARTESIAN_POINT('Ctrl Pts',(7.17384635845214,-3.3616656859284,-3.36166568592789));
#58448=CARTESIAN_POINT('Ctrl Pts',(7.19420493717891,-3.35481115621028,-3.35481115621027));
#58449=CARTESIAN_POINT('Ctrl Pts',(7.21511249441201,-3.34777994985527,-3.34777995566559));
#58450=CARTESIAN_POINT('Ctrl Pts',(7.23681685935962,-3.34048647397502,-3.34048648878989));
#58451=CARTESIAN_POINT('Ctrl Pts',(7.32483941486278,-3.31090761336196,-3.31090766469499));
#58452=CARTESIAN_POINT('Ctrl Pts',(7.41251809600317,-3.28153366858737,-3.28153366858751));
#58453=CARTESIAN_POINT('Ctrl Pts',(7.49999999999092,-3.25205165383156,-3.25205165383202));
#58454=CARTESIAN_POINT('Ctrl Pts',(7.17384635845215,-4.59212072600837,-1.2304550400798));
#58455=CARTESIAN_POINT('Ctrl Pts',(7.18694338462328,-4.58871947646023,-1.18580378192515));
#58456=CARTESIAN_POINT('Ctrl Pts',(7.19993346366831,-4.58523137267447,-1.14112866266544));
#58457=CARTESIAN_POINT('Ctrl Pts',(7.21281435373035,-4.58165253645087,-1.096429346886));
#58458=CARTESIAN_POINT('Ctrl Pts',(7.2697816987673,-4.54536447860044,-1.26184274766089));
#58459=CARTESIAN_POINT('Ctrl Pts',(7.28299669995037,-4.54206016538012,-1.21721772087861));
#58460=CARTESIAN_POINT('Ctrl Pts',(7.29604661499974,-4.53862178188785,-1.17255586152565));
#58461=CARTESIAN_POINT('Ctrl Pts',(7.30892798333169,-4.53504334164129,-1.12785665184795));
#58462=CARTESIAN_POINT('Ctrl Pts',(7.36571703908244,-4.4986082311925,-1.29323045524197));
#58463=CARTESIAN_POINT('Ctrl Pts',(7.37905001527745,-4.49540085430002,-1.24863165983206));
#58464=CARTESIAN_POINT('Ctrl Pts',(7.39215976633117,-4.49201219110123,-1.20398306038586));
#58465=CARTESIAN_POINT('Ctrl Pts',(7.40504161293303,-4.4884341468317,-1.15928395680991));
#58466=CARTESIAN_POINT('Ctrl Pts',(7.46165237939758,-4.45185198378456,-1.32461816282306));
#58467=CARTESIAN_POINT('Ctrl Pts',(7.47510333060454,-4.44874154321992,-1.28004559878552));
#58468=CARTESIAN_POINT('Ctrl Pts',(7.4882729176626,-4.44540260031461,-1.23541025924608));
#58469=CARTESIAN_POINT('Ctrl Pts',(7.50115524253438,-4.44182495202211,-1.19071126177187));
#58470=CARTESIAN_POINT('',(7.49999999999943,-4.44214493194956,-1.19471687171392));
#58471=CARTESIAN_POINT('Ctrl Pts',(7.46165237939758,-4.45185198378456,-1.32461816282306));
#58472=CARTESIAN_POINT('Ctrl Pts',(7.47470152024065,-4.44883445912125,-1.28137708218025));
#58473=CARTESIAN_POINT('Ctrl Pts',(7.48748585582712,-4.44560187997715,-1.23807692051041));
#58474=CARTESIAN_POINT('Ctrl Pts',(7.50000000105064,-4.44214493062789,-1.19471687212266));
#58475=CARTESIAN_POINT('',(7.49999999999226,-4.44238517355628,-1.19033351972274));
#58476=CARTESIAN_POINT('Ctrl Pts',(7.50000000105118,-4.44214493062774,-1.19471687212079));
#58477=CARTESIAN_POINT('Ctrl Pts',(7.50000000037148,-4.44222534202356,-1.1932558707691));
#58478=CARTESIAN_POINT('Ctrl Pts',(7.49999999647456,-4.4423054234084,-1.19179476415889));
#58479=CARTESIAN_POINT('Ctrl Pts',(7.49999999999088,-4.44238517355332,-1.19033351972258));
#58480=CARTESIAN_POINT('Ctrl Pts',(7.17384635845216,-4.59212072600837,-1.2304550400798));
#58481=CARTESIAN_POINT('Ctrl Pts',(7.19439695636075,-4.58266894946052,-1.22792244418713));
#58482=CARTESIAN_POINT('Ctrl Pts',(7.21552165468893,-4.57296449112451,-1.22532214675418));
#58483=CARTESIAN_POINT('Ctrl Pts',(7.23748292043925,-4.56288364865534,-1.22262099986246));
#58484=CARTESIAN_POINT('Ctrl Pts',(7.32528335544047,-4.52258076429365,-1.21182190135918));
#58485=CARTESIAN_POINT('Ctrl Pts',(7.41273830259824,-4.48255698032657,-1.2010975229051));
#58486=CARTESIAN_POINT('Ctrl Pts',(7.49999999999083,-4.44238517355338,-1.19033351972196));
#58487=CARTESIAN_POINT('Ctrl Pts',(6.99737260418672,4.6377372761525,1.32346176996264));
#58488=CARTESIAN_POINT('Ctrl Pts',(6.872142618999,4.88518053653228,0.964484375855836));
#58489=CARTESIAN_POINT('Ctrl Pts',(6.69496761793157,5.14481481295669,0.587820910346251));
#58490=CARTESIAN_POINT('Ctrl Pts',(6.45213506509495,5.4329389838526,0.169825835884927));
#58491=CARTESIAN_POINT('Ctrl Pts',(7.15213252925707,4.59773351518726,1.241898850833));
#58492=CARTESIAN_POINT('Ctrl Pts',(7.02199092199136,4.84933943348488,0.874086497162871));
#58493=CARTESIAN_POINT('Ctrl Pts',(6.83894619861566,5.11140456395289,0.490509429775467));
#58494=CARTESIAN_POINT('Ctrl Pts',(6.59045151405566,5.40083506390477,0.0673422078825931));
#58495=CARTESIAN_POINT('Ctrl Pts',(7.30689245432741,4.55772975422203,1.16033593170335));
#58496=CARTESIAN_POINT('Ctrl Pts',(7.17183922498372,4.81349833043748,0.783688618469907));
#58497=CARTESIAN_POINT('Ctrl Pts',(6.98292477929974,5.07799431494909,0.393197949204684));
#58498=CARTESIAN_POINT('Ctrl Pts',(6.72876796301638,5.36873114395694,-0.0351414201197404));
#58499=CARTESIAN_POINT('Ctrl Pts',(7.46165237939775,4.51772599325679,1.07877301257371));
#58500=CARTESIAN_POINT('Ctrl Pts',(7.32168752797609,4.77765722739008,0.693290739776942));
#58501=CARTESIAN_POINT('Ctrl Pts',(7.12690335998383,5.04458406594529,0.295886468633901));
#58502=CARTESIAN_POINT('Ctrl Pts',(6.86708441197709,5.33662722400912,-0.137625048122074));
#58503=CARTESIAN_POINT('Ctrl Pts',(6.49649612061064,5.37973548846878,0.247010609885015));
#58504=CARTESIAN_POINT('Ctrl Pts',(6.70189613387518,5.13067066995955,0.608340473446071));
#58505=CARTESIAN_POINT('Ctrl Pts',(6.85768162696567,4.90264379362682,0.939149620264626));
#58506=CARTESIAN_POINT('Ctrl Pts',(6.97303770582829,4.68473733652944,1.25527660633733));
#58507=CARTESIAN_POINT('',(7.46165237939775,4.51772599325679,1.07877301257371));
#58508=CARTESIAN_POINT('Ctrl Pts',(7.46165237939775,4.51772599325679,1.07877301257371));
#58509=CARTESIAN_POINT('Ctrl Pts',(7.36571703908279,4.54252423750726,1.12933368840906));
#58510=CARTESIAN_POINT('Ctrl Pts',(7.26978169876783,4.56732248175773,1.1798943642444));
#58511=CARTESIAN_POINT('Ctrl Pts',(7.17384635845286,4.59212072600819,1.23045504007975));
#58512=CARTESIAN_POINT('Ctrl Pts',(7.46165237939775,4.51772599325679,1.07877301257371));
#58513=CARTESIAN_POINT('Ctrl Pts',(7.33663088231331,4.7499056562241,0.734446773842698));
#58514=CARTESIAN_POINT('Ctrl Pts',(7.16787076968672,4.98766689283072,0.380608346073535));
#58515=CARTESIAN_POINT('Ctrl Pts',(6.94809164225642,5.24392405018004,2.12859752745428E-5));
#58516=CARTESIAN_POINT('Ctrl Pts',(7.17384635845268,4.59212072600811,1.23045504007998));
#58517=CARTESIAN_POINT('Ctrl Pts',(7.18694338462382,4.58871947645997,1.18580378192533));
#58518=CARTESIAN_POINT('Ctrl Pts',(7.19993346366884,4.58523137267421,1.14112866266561));
#58519=CARTESIAN_POINT('Ctrl Pts',(7.21281435373088,4.58165253645062,1.09642934688617));
#58520=CARTESIAN_POINT('Ctrl Pts',(7.26978169876765,4.54536447860026,1.261842747661));
#58521=CARTESIAN_POINT('Ctrl Pts',(7.28299669995072,4.54206016537995,1.21721772087872));
#58522=CARTESIAN_POINT('Ctrl Pts',(7.29604661500009,4.53862178188768,1.17255586152576));
#58523=CARTESIAN_POINT('Ctrl Pts',(7.30892798333205,4.53504334164112,1.12785665184807));
#58524=CARTESIAN_POINT('Ctrl Pts',(7.36571703908262,4.49860823119241,1.29323045524203));
#58525=CARTESIAN_POINT('Ctrl Pts',(7.37905001527763,4.49540085429993,1.24863165983212));
#58526=CARTESIAN_POINT('Ctrl Pts',(7.39215976633134,4.49201219110115,1.20398306038592));
#58527=CARTESIAN_POINT('Ctrl Pts',(7.40504161293321,4.48843414683161,1.15928395680997));
#58528=CARTESIAN_POINT('Ctrl Pts',(7.46165237939758,4.45185198378456,1.32461816282306));
#58529=CARTESIAN_POINT('Ctrl Pts',(7.47510333060454,4.44874154321992,1.28004559878552));
#58530=CARTESIAN_POINT('Ctrl Pts',(7.4882729176626,4.44540260031461,1.23541025924608));
#58531=CARTESIAN_POINT('Ctrl Pts',(7.50115524253438,4.44182495202211,1.19071126177187));
#58532=CARTESIAN_POINT('',(7.49999999999943,4.44214493194956,1.19471687171392));
#58533=CARTESIAN_POINT('Ctrl Pts',(7.46165237939758,4.45185198378456,1.32461816282306));
#58534=CARTESIAN_POINT('Ctrl Pts',(7.47470152024064,4.44883445912125,1.28137708218025));
#58535=CARTESIAN_POINT('Ctrl Pts',(7.48748585582712,4.44560187997715,1.23807692051041));
#58536=CARTESIAN_POINT('Ctrl Pts',(7.50000000105064,4.44214493062788,1.19471687212266));
#58537=CARTESIAN_POINT('',(7.49999999999226,4.44238517355628,1.19033351972274));
#58538=CARTESIAN_POINT('Ctrl Pts',(7.50000000105118,4.44214493062774,1.19471687212079));
#58539=CARTESIAN_POINT('Ctrl Pts',(7.50000000037147,4.44222534202356,1.1932558707691));
#58540=CARTESIAN_POINT('Ctrl Pts',(7.49999999647456,4.4423054234084,1.19179476415888));
#58541=CARTESIAN_POINT('Ctrl Pts',(7.49999999999088,4.44238517355332,1.19033351972257));
#58542=CARTESIAN_POINT('Ctrl Pts',(7.49999999999083,4.44238517355338,1.19033351972196));
#58543=CARTESIAN_POINT('Ctrl Pts',(7.41273830259822,4.48255698032658,1.2010975229051));
#58544=CARTESIAN_POINT('Ctrl Pts',(7.32528335544063,4.52258076429358,1.21182190135916));
#58545=CARTESIAN_POINT('Ctrl Pts',(7.23748292043925,4.56288364865534,1.22262099986247));
#58546=CARTESIAN_POINT('Ctrl Pts',(7.21552165468913,4.57296449112441,1.22532214675415));
#58547=CARTESIAN_POINT('Ctrl Pts',(7.19439695636114,4.58266894946034,1.22792244418708));
#58548=CARTESIAN_POINT('Ctrl Pts',(7.17384635845268,4.59212072600811,1.23045504007998));
#58549=CARTESIAN_POINT('Ctrl Pts',(6.99737260418672,3.35466741224479,3.46502015180142));
#58550=CARTESIAN_POINT('Ctrl Pts',(6.872142618999,3.74844825878233,3.27785823931047));
#58551=CARTESIAN_POINT('Ctrl Pts',(6.69496761793157,4.16162987061384,3.08147524771389));
#58552=CARTESIAN_POINT('Ctrl Pts',(6.45213506509495,4.6201502592847,2.86354298002157));
#58553=CARTESIAN_POINT('Ctrl Pts',(7.15213252925707,3.3608045985668,3.37438271134571));
#58554=CARTESIAN_POINT('Ctrl Pts',(7.02199092199136,3.76260789239011,3.18165082839044));
#58555=CARTESIAN_POINT('Ctrl Pts',(6.83894619861566,4.18135148651518,2.98049590895782));
#58556=CARTESIAN_POINT('Ctrl Pts',(6.59045151405566,4.64358926304999,2.75873759472565));
#58557=CARTESIAN_POINT('Ctrl Pts',(7.30689245432741,3.3669417848888,3.28374527089));
#58558=CARTESIAN_POINT('Ctrl Pts',(7.17183922498373,3.77676752599789,3.08544341747041));
#58559=CARTESIAN_POINT('Ctrl Pts',(6.98292477929975,4.20107310241652,2.87951657020175));
#58560=CARTESIAN_POINT('Ctrl Pts',(6.72876796301638,4.66702826681527,2.65393220942972));
#58561=CARTESIAN_POINT('Ctrl Pts',(7.46165237939775,3.37307897121081,3.1931078304343));
#58562=CARTESIAN_POINT('Ctrl Pts',(7.32168752797609,3.79092715960566,2.98923600655038));
#58563=CARTESIAN_POINT('Ctrl Pts',(7.12690335998383,4.22079471831786,2.77853723144567));
#58564=CARTESIAN_POINT('Ctrl Pts',(6.86708441197709,4.69046727058056,2.54912682413379));
#58565=CARTESIAN_POINT('Ctrl Pts',(6.49649612061064,4.53548229371214,2.9037852073991));
#58566=CARTESIAN_POINT('Ctrl Pts',(6.70189613387518,4.13912090191365,3.09217363913432));
#58567=CARTESIAN_POINT('Ctrl Pts',(6.85768162696566,3.77623926085462,3.26464932591708));
#58568=CARTESIAN_POINT('Ctrl Pts',(6.97303770582829,3.42946324032328,3.42947009812916));
#58569=CARTESIAN_POINT('',(7.46165237939775,3.37307897121081,3.1931078304343));
#58570=CARTESIAN_POINT('Ctrl Pts',(7.46165237939775,3.37307897121081,3.1931078304343));
#58571=CARTESIAN_POINT('Ctrl Pts',(7.36571703908279,3.36927454278329,3.24929378226545));
#58572=CARTESIAN_POINT('Ctrl Pts',(7.26978169876783,3.36547011435578,3.3054797340966));
#58573=CARTESIAN_POINT('Ctrl Pts',(7.17384635845287,3.36166568592826,3.36166568592776));
#58574=CARTESIAN_POINT('Ctrl Pts',(7.46165237939775,3.37307897121081,3.1931078304343));
#58575=CARTESIAN_POINT('Ctrl Pts',(7.33663088231331,3.74631557694812,3.01100239198735));
#58576=CARTESIAN_POINT('Ctrl Pts',(7.16787076968672,4.12914206176923,2.82344994300742));
#58577=CARTESIAN_POINT('Ctrl Pts',(6.94809164225641,4.54136079998446,2.62198045928535));
#58578=CARTESIAN_POINT('Ctrl Pts',(7.17384635845274,3.36166568592805,3.36166568592792));
#58579=CARTESIAN_POINT('Ctrl Pts',(7.18694338462388,3.38104574649207,3.32129593728098));
#58580=CARTESIAN_POINT('Ctrl Pts',(7.1999334636689,3.40036251963242,3.28086209719208));
#58581=CARTESIAN_POINT('Ctrl Pts',(7.21281435373094,3.41961281443653,3.2403619360835));
#58582=CARTESIAN_POINT('Ctrl Pts',(7.26978169876769,3.30547973409671,3.36547011435572));
#58583=CARTESIAN_POINT('Ctrl Pts',(7.28299669995076,3.324930628297,3.32517155090754));
#58584=CARTESIAN_POINT('Ctrl Pts',(7.29604661500013,3.34428383052122,3.28477405438149));
#58585=CARTESIAN_POINT('Ctrl Pts',(7.30892798333209,3.36353441520062,3.24427418314824));
#58586=CARTESIAN_POINT('Ctrl Pts',(7.36571703908264,3.24929378226538,3.36927454278352));
#58587=CARTESIAN_POINT('Ctrl Pts',(7.37905001527765,3.26881551010194,3.32904716453411));
#58588=CARTESIAN_POINT('Ctrl Pts',(7.39215976633137,3.28820514141002,3.28868601157091));
#58589=CARTESIAN_POINT('Ctrl Pts',(7.40504161293323,3.30745601596472,3.24818643021297));
#58590=CARTESIAN_POINT('Ctrl Pts',(7.46165237939758,3.19310783043405,3.37307897121132));
#58591=CARTESIAN_POINT('Ctrl Pts',(7.47510333060454,3.21270039190688,3.33292277816068));
#58592=CARTESIAN_POINT('Ctrl Pts',(7.4882729176626,3.23212645229882,3.29259796876032));
#58593=CARTESIAN_POINT('Ctrl Pts',(7.50115524253438,3.25137761672882,3.25209867727771));
#58594=CARTESIAN_POINT('',(7.49999999999943,3.24965192250365,3.25572762720891));
#58595=CARTESIAN_POINT('Ctrl Pts',(7.46165237939758,3.19310783043405,3.37307897121132));
#58596=CARTESIAN_POINT('Ctrl Pts',(7.47470152024065,3.21211511774048,3.3341223345559));
#58597=CARTESIAN_POINT('Ctrl Pts',(7.48748585582712,3.23096570291687,3.2950070049898));
#58598=CARTESIAN_POINT('Ctrl Pts',(7.50000000105064,3.24965192115468,3.25572762690205));
#58599=CARTESIAN_POINT('',(7.49999999999234,3.25205165383366,3.25205165383413));
#58600=CARTESIAN_POINT('Ctrl Pts',(7.50000000105118,3.24965192115549,3.25572762690036));
#58601=CARTESIAN_POINT('Ctrl Pts',(7.50000000037148,3.25045206029546,3.25450256807911));
#58602=CARTESIAN_POINT('Ctrl Pts',(7.49999999647522,3.25125196611448,3.25327725332823));
#58603=CARTESIAN_POINT('Ctrl Pts',(7.49999999999097,3.25205165383121,3.25205165383252));
#58604=CARTESIAN_POINT('Ctrl Pts',(7.49999999999092,3.25205165383156,3.25205165383202));
#58605=CARTESIAN_POINT('Ctrl Pts',(7.41251809600285,3.28153366858747,3.28153366858761));
#58606=CARTESIAN_POINT('Ctrl Pts',(7.32483941486394,3.31090761336157,3.3109076646946));
#58607=CARTESIAN_POINT('Ctrl Pts',(7.23681685935962,3.34048647397502,3.34048648878989));
#58608=CARTESIAN_POINT('Ctrl Pts',(7.21511249441227,3.34777994985518,3.3477799556655));
#58609=CARTESIAN_POINT('Ctrl Pts',(7.19420493717939,3.35481115621011,3.35481115621012));
#58610=CARTESIAN_POINT('Ctrl Pts',(7.17384635845274,3.36166568592805,3.36166568592792));
#58611=CARTESIAN_POINT('Ctrl Pts',(6.99737260418672,1.17271712435108,4.67812918220743));
#58612=CARTESIAN_POINT('Ctrl Pts',(6.872142618999,1.60732229722181,4.71293263463817));
#58613=CARTESIAN_POINT('Ctrl Pts',(6.69496761793157,2.06333956524279,4.7494507809601));
#58614=CARTESIAN_POINT('Ctrl Pts',(6.45213506509495,2.56939600383103,4.78997609516963));
#58615=CARTESIAN_POINT('Ctrl Pts',(7.15213252925707,1.22335080384155,4.6027034493998));
#58616=CARTESIAN_POINT('Ctrl Pts',(7.02199092199136,1.66768860509444,4.63669438955298));
#58617=CARTESIAN_POINT('Ctrl Pts',(6.83894619861566,2.13090865499507,4.67186091629066));
#58618=CARTESIAN_POINT('Ctrl Pts',(6.59045151405566,2.64209746917913,4.71093147093258));
#58619=CARTESIAN_POINT('Ctrl Pts',(7.30689245432741,1.27398448333202,4.52727771659216));
#58620=CARTESIAN_POINT('Ctrl Pts',(7.17183922498372,1.72805491296707,4.56045614446779));
#58621=CARTESIAN_POINT('Ctrl Pts',(6.98292477929974,2.19847774474734,4.59427105162121));
#58622=CARTESIAN_POINT('Ctrl Pts',(6.72876796301637,2.71479893452723,4.63188684669553));
#58623=CARTESIAN_POINT('Ctrl Pts',(7.46165237939775,1.32461816282249,4.45185198378452));
#58624=CARTESIAN_POINT('Ctrl Pts',(7.32168752797609,1.7884212208397,4.48421789938261));
#58625=CARTESIAN_POINT('Ctrl Pts',(7.12690335998383,2.26604683449962,4.51668118695177));
#58626=CARTESIAN_POINT('Ctrl Pts',(6.86708441197709,2.78750039987533,4.55284222245849));
#58627=CARTESIAN_POINT('Ctrl Pts',(6.49649612061063,2.47595028106968,4.78249290359715));
#58628=CARTESIAN_POINT('Ctrl Pts',(6.70189613387517,2.03849703082522,4.74746137535973));
#58629=CARTESIAN_POINT('Ctrl Pts',(6.85768162696566,1.63799446770973,4.71538888111925));
#58630=CARTESIAN_POINT('Ctrl Pts',(6.97303770582829,1.25526723840028,4.68473984666061));
#58631=CARTESIAN_POINT('',(7.46165237939775,1.32461816282249,4.45185198378452));
#58632=CARTESIAN_POINT('Ctrl Pts',(7.46165237939775,1.32461816282249,4.45185198378452));
#58633=CARTESIAN_POINT('Ctrl Pts',(7.36571703908279,1.29323045524181,4.49860823119235));
#58634=CARTESIAN_POINT('Ctrl Pts',(7.26978169876783,1.26184274766112,4.54536447860018));
#58635=CARTESIAN_POINT('Ctrl Pts',(7.17384635845286,1.23045504008043,4.59212072600801));
#58636=CARTESIAN_POINT('Ctrl Pts',(7.46165237939775,1.32461816282249,4.45185198378452));
#58637=CARTESIAN_POINT('Ctrl Pts',(7.33663088231331,1.73890326423675,4.48076235079082));
#58638=CARTESIAN_POINT('Ctrl Pts',(7.16787076968672,2.1642169498233,4.50975040784277));
#58639=CARTESIAN_POINT('Ctrl Pts',(6.94809164225641,2.62194359089469,4.54138208595974));
#58640=CARTESIAN_POINT('Ctrl Pts',(7.17384635845275,1.23045504008017,4.59212072600804));
#58641=CARTESIAN_POINT('Ctrl Pts',(7.18694338462388,1.26742353917896,4.56684952841741));
#58642=CARTESIAN_POINT('Ctrl Pts',(7.1999334636689,1.3043692754821,4.54149118229804));
#58643=CARTESIAN_POINT('Ctrl Pts',(7.21281435373095,1.34129060036708,4.5160421613227));
#58644=CARTESIAN_POINT('Ctrl Pts',(7.26978169876769,1.17989436424452,4.56732248175773));
#58645=CARTESIAN_POINT('Ctrl Pts',(7.28299669995077,1.21688861447239,4.54214834917574));
#58646=CARTESIAN_POINT('Ctrl Pts',(7.29604661500014,1.25384772750616,4.51683969204699));
#58647=CARTESIAN_POINT('Ctrl Pts',(7.30892798333209,1.29076915849286,4.49139106704869));
#58648=CARTESIAN_POINT('Ctrl Pts',(7.36571703908264,1.12933368840888,4.54252423750742));
#58649=CARTESIAN_POINT('Ctrl Pts',(7.37905001527765,1.16635368976581,4.51744716993406));
#58650=CARTESIAN_POINT('Ctrl Pts',(7.39215976633137,1.20332617953023,4.49218820179594));
#58651=CARTESIAN_POINT('Ctrl Pts',(7.40504161293324,1.24024771661863,4.46673997277468));
#58652=CARTESIAN_POINT('Ctrl Pts',(7.46165237939758,1.07877301257324,4.51772599325711));
#58653=CARTESIAN_POINT('Ctrl Pts',(7.47510333060454,1.11581876505924,4.49274599069239));
#58654=CARTESIAN_POINT('Ctrl Pts',(7.4882729176626,1.15280463155429,4.46753671154489));
#58655=CARTESIAN_POINT('Ctrl Pts',(7.50115524253438,1.18972627474441,4.44208887850067));
#58656=CARTESIAN_POINT('',(7.49999999999234,1.19033351972209,4.44238517355638));
#58657=CARTESIAN_POINT('Ctrl Pts',(7.50000000105118,1.18641730372738,4.44436879327628));
#58658=CARTESIAN_POINT('Ctrl Pts',(7.50000000037148,1.18772277427295,4.4437079306274));
#58659=CARTESIAN_POINT('Ctrl Pts',(7.49999999647595,1.18902817040918,4.44304672983401));
#58660=CARTESIAN_POINT('Ctrl Pts',(7.49999999999097,1.19033351972076,4.44238517355376));
#58661=CARTESIAN_POINT('Ctrl Pts',(7.49999999999092,1.19033351972131,4.44238517355351));
#58662=CARTESIAN_POINT('Ctrl Pts',(7.4125189586941,1.20112457966122,4.4826579575159));
#58663=CARTESIAN_POINT('Ctrl Pts',(7.32484115407291,1.21187605713238,4.52278315794289));
#58664=CARTESIAN_POINT('Ctrl Pts',(7.23681946879609,1.22270258210925,4.56318819945531));
#58665=CARTESIAN_POINT('Ctrl Pts',(7.21511409889809,1.22537230751378,4.5731517257047));
#58666=CARTESIAN_POINT('Ctrl Pts',(7.19420569065439,1.22794601521628,4.58275691773891));
#58667=CARTESIAN_POINT('Ctrl Pts',(7.17384635845275,1.23045504008016,4.59212072600804));
#58668=CARTESIAN_POINT('Ctrl Pts',(6.97302668913468,-1.25527236874723,4.68474025750198));
#58669=CARTESIAN_POINT('Ctrl Pts',(6.84940428632249,-0.916731434795263,
4.91809665777761));
#58670=CARTESIAN_POINT('Ctrl Pts',(6.67964184929033,-0.561440197692398,
5.16299904867006));
#58671=CARTESIAN_POINT('Ctrl Pts',(6.45213506520422,-0.169825836073017,
5.43293898372295));
#58672=CARTESIAN_POINT('Ctrl Pts',(7.12684466416248,-1.17205861623371,4.64550450560439));
#58673=CARTESIAN_POINT('Ctrl Pts',(6.99850389456238,-0.825458101169696,
4.8825619686287));
#58674=CARTESIAN_POINT('Ctrl Pts',(6.82326307870631,-0.463802289985809,
5.12967124535383));
#58675=CARTESIAN_POINT('Ctrl Pts',(6.59045151416748,-0.0673422080730113,
5.40083506377453));
#58676=CARTESIAN_POINT('Ctrl Pts',(7.28066263919028,-1.0888448637202,4.6062687537068));
#58677=CARTESIAN_POINT('Ctrl Pts',(7.14760350280226,-0.73418476754413,4.8470272794798));
#58678=CARTESIAN_POINT('Ctrl Pts',(6.9668843081223,-0.366164382279219,5.09634344203759));
#58679=CARTESIAN_POINT('Ctrl Pts',(6.72876796313074,0.0351414199269946,
5.36873114382612));
#58680=CARTESIAN_POINT('Ctrl Pts',(7.43448061421808,-1.00563111120669,4.56703300180921));
#58681=CARTESIAN_POINT('Ctrl Pts',(7.29670311104215,-0.642911433918564,
4.81149259033089));
#58682=CARTESIAN_POINT('Ctrl Pts',(7.11050553753828,-0.26852647457263,5.06301563872136));
#58683=CARTESIAN_POINT('Ctrl Pts',(6.867084412094,0.137625047927001,5.3366272238777));
#58684=CARTESIAN_POINT('Ctrl Pts',(6.49649473556578,-0.247010070495211,
5.37973586027038));
#58685=CARTESIAN_POINT('Ctrl Pts',(6.70188214815405,-0.608335026879687,
5.13067442427992));
#58686=CARTESIAN_POINT('Ctrl Pts',(6.85757546768223,-0.939108279979382,
4.90267228950186));
#58687=CARTESIAN_POINT('Ctrl Pts',(6.97302668913468,-1.25527236874723,4.68474025750198));
#58688=CARTESIAN_POINT('Ctrl Pts',(7.2128143537305,1.09642934688643,4.5816525364507));
#58689=CARTESIAN_POINT('Ctrl Pts',(7.19993346366857,1.14112866266591,4.58523137267427));
#58690=CARTESIAN_POINT('Ctrl Pts',(7.18694338462366,1.18580378192567,4.58871947646));
#58691=CARTESIAN_POINT('Ctrl Pts',(7.17384635845263,1.23045504008035,4.59212072600812));
#58692=CARTESIAN_POINT('Ctrl Pts',(7.30892798333179,1.12785665184803,4.53504334164122));
#58693=CARTESIAN_POINT('Ctrl Pts',(7.29604661499993,1.17255586152576,4.53862178188775));
#58694=CARTESIAN_POINT('Ctrl Pts',(7.28299669995066,1.21721772087875,4.54206016537998));
#58695=CARTESIAN_POINT('Ctrl Pts',(7.26978169876767,1.26184274766107,4.54536447860025));
#58696=CARTESIAN_POINT('Ctrl Pts',(7.40504161293309,1.15928395680962,4.48843414683175));
#58697=CARTESIAN_POINT('Ctrl Pts',(7.3921597663313,1.20398306038561,4.49201219110123));
#58698=CARTESIAN_POINT('Ctrl Pts',(7.37905001527766,1.24863165983184,4.49540085429997));
#58699=CARTESIAN_POINT('Ctrl Pts',(7.36571703908271,1.29323045524178,4.49860823119239));
#58700=CARTESIAN_POINT('Ctrl Pts',(7.50115524253438,1.19071126177122,4.44182495202228));
#58701=CARTESIAN_POINT('Ctrl Pts',(7.48827291766266,1.23541025924546,4.44540260031471));
#58702=CARTESIAN_POINT('Ctrl Pts',(7.47510333060465,1.28004559878492,4.44874154321995));
#58703=CARTESIAN_POINT('Ctrl Pts',(7.46165237939775,1.32461816282249,4.45185198378452));
#58704=CARTESIAN_POINT('',(7.49999999999943,1.19471687171331,4.44214493194972));
#58705=CARTESIAN_POINT('Ctrl Pts',(7.49999999999097,1.19033351972193,4.44238517355345));
#58706=CARTESIAN_POINT('Ctrl Pts',(7.49999999569756,1.19179469976444,4.44230542728599));
#58707=CARTESIAN_POINT('Ctrl Pts',(7.50000000037144,1.1932558035927,4.44222534572098));
#58708=CARTESIAN_POINT('Ctrl Pts',(7.50000000105118,1.19471687212018,4.4421449306279));
#58709=CARTESIAN_POINT('Ctrl Pts',(7.50000000105064,1.19471687212205,4.44214493062805));
#58710=CARTESIAN_POINT('Ctrl Pts',(7.48748585582718,1.23807692050981,4.44560187997725));
#58711=CARTESIAN_POINT('Ctrl Pts',(7.47470152024076,1.28137708217967,4.44883445912128));
#58712=CARTESIAN_POINT('Ctrl Pts',(7.46165237939775,1.32461816282249,4.45185198378452));
#58713=CARTESIAN_POINT('Ctrl Pts',(7.21281435373049,3.24036193608378,3.4196128144365));
#58714=CARTESIAN_POINT('Ctrl Pts',(7.19993346366856,3.28086209719237,3.40036251963235));
#58715=CARTESIAN_POINT('Ctrl Pts',(7.18694338462365,3.32129593728129,3.38104574649196));
#58716=CARTESIAN_POINT('Ctrl Pts',(7.17384635845263,3.36166568592825,3.3616656859279));
#58717=CARTESIAN_POINT('Ctrl Pts',(7.30892798333179,3.24427418314827,3.36353441520076));
#58718=CARTESIAN_POINT('Ctrl Pts',(7.29604661499993,3.28477405438153,3.34428383052131));
#58719=CARTESIAN_POINT('Ctrl Pts',(7.28299669995065,3.32517155090759,3.32493062829704));
#58720=CARTESIAN_POINT('Ctrl Pts',(7.26978169876767,3.36547011435577,3.3054797340967));
#58721=CARTESIAN_POINT('Ctrl Pts',(7.40504161293308,3.24818643021275,3.30745601596502));
#58722=CARTESIAN_POINT('Ctrl Pts',(7.39215976633129,3.28868601157069,3.28820514141026));
#58723=CARTESIAN_POINT('Ctrl Pts',(7.37905001527765,3.32904716453388,3.26881551010212));
#58724=CARTESIAN_POINT('Ctrl Pts',(7.36571703908271,3.36927454278329,3.2492937822655));
#58725=CARTESIAN_POINT('Ctrl Pts',(7.50115524253438,3.25209867727724,3.25137761672928));
#58726=CARTESIAN_POINT('Ctrl Pts',(7.48827291766266,3.29259796875984,3.23212645229921));
#58727=CARTESIAN_POINT('Ctrl Pts',(7.47510333060465,3.33292277816018,3.2127003919072));
#58728=CARTESIAN_POINT('Ctrl Pts',(7.46165237939775,3.37307897121081,3.1931078304343));
#58729=CARTESIAN_POINT('',(7.49999999999943,3.25572762720846,3.24965192250411));
#58730=CARTESIAN_POINT('Ctrl Pts',(7.49999999999097,3.25205165383206,3.25205165383167));
#58731=CARTESIAN_POINT('Ctrl Pts',(7.49999999570083,3.25327719982305,3.25125200145742));
#58732=CARTESIAN_POINT('Ctrl Pts',(7.50000000037144,3.25450251208352,3.25045209686877));
#58733=CARTESIAN_POINT('Ctrl Pts',(7.50000000105118,3.25572762689991,3.24965192115593));
#58734=CARTESIAN_POINT('Ctrl Pts',(7.50000000105064,3.2557276269016,3.24965192115513));
#58735=CARTESIAN_POINT('Ctrl Pts',(7.48748585582718,3.29500700498933,3.23096570291725));
#58736=CARTESIAN_POINT('Ctrl Pts',(7.47470152024076,3.33412233455541,3.21211511774079));
#58737=CARTESIAN_POINT('Ctrl Pts',(7.46165237939775,3.37307897121081,3.1931078304343));
#58738=CARTESIAN_POINT('Ctrl Pts',(7.21281435373043,4.51604216132295,1.34129060036694));
#58739=CARTESIAN_POINT('Ctrl Pts',(7.1999334636685,4.54149118229828,1.30436927548192));
#58740=CARTESIAN_POINT('Ctrl Pts',(7.18694338462359,4.56684952841764,1.26742353917874));
#58741=CARTESIAN_POINT('Ctrl Pts',(7.17384635845257,4.59212072600827,1.23045504007991));
#58742=CARTESIAN_POINT('Ctrl Pts',(7.30892798333175,4.4913910670488,1.29076915849297));
#58743=CARTESIAN_POINT('Ctrl Pts',(7.29604661499989,4.51683969204708,1.25384772750623));
#58744=CARTESIAN_POINT('Ctrl Pts',(7.28299669995061,4.5421483491758,1.21688861447241));
#58745=CARTESIAN_POINT('Ctrl Pts',(7.26978169876763,4.56732248175777,1.17989436424451));
#58746=CARTESIAN_POINT('Ctrl Pts',(7.40504161293306,4.46673997277466,1.240247716619));
#58747=CARTESIAN_POINT('Ctrl Pts',(7.39215976633127,4.49218820179588,1.20332617953055));
#58748=CARTESIAN_POINT('Ctrl Pts',(7.37905001527763,4.51744716993396,1.16635368976609));
#58749=CARTESIAN_POINT('Ctrl Pts',(7.36571703908269,4.54252423750728,1.12933368840911));
#58750=CARTESIAN_POINT('Ctrl Pts',(7.50115524253438,4.44208887850051,1.18972627474503));
#58751=CARTESIAN_POINT('Ctrl Pts',(7.48827291766266,4.46753671154468,1.15280463155486));
#58752=CARTESIAN_POINT('Ctrl Pts',(7.47510333060465,4.49274599069213,1.11581876505976));
#58753=CARTESIAN_POINT('Ctrl Pts',(7.46165237939775,4.51772599325679,1.07877301257371));
#58754=CARTESIAN_POINT('',(7.49999999999943,4.44436879421741,1.18641730474127));
#58755=CARTESIAN_POINT('Ctrl Pts',(7.49999999999088,4.44238517355364,1.1903335197214));
#58756=CARTESIAN_POINT('Ctrl Pts',(7.49999999570487,4.44304670138692,1.18902822733552));
#58757=CARTESIAN_POINT('Ctrl Pts',(7.50000000037144,4.4437079006456,1.1877228334994));
#58758=CARTESIAN_POINT('Ctrl Pts',(7.50000000105118,4.44436879327611,1.18641730372799));
#58759=CARTESIAN_POINT('Ctrl Pts',(7.50000000105064,4.44436879327717,1.18641730372645));
#58760=CARTESIAN_POINT('Ctrl Pts',(7.48748585582718,4.46904262342706,1.15059487498792));
#58761=CARTESIAN_POINT('Ctrl Pts',(7.47470152024076,4.49349219992046,1.11471212456586));
#58762=CARTESIAN_POINT('Ctrl Pts',(7.46165237939775,4.51772599325679,1.07877301257371));
#58763=CARTESIAN_POINT('Ctrl Pts',(7.2128143537299,-4.51604216132309,-1.34129060036722));
#58764=CARTESIAN_POINT('Ctrl Pts',(7.19993346366797,-4.54149118229842,-1.3043692754822));
#58765=CARTESIAN_POINT('Ctrl Pts',(7.18694338462306,-4.56684952841778,-1.26742353917902));
#58766=CARTESIAN_POINT('Ctrl Pts',(7.17384635845204,-4.5921207260084,-1.23045504008019));
#58767=CARTESIAN_POINT('Ctrl Pts',(7.30892798333139,-4.49139106704889,-1.29076915849316));
#58768=CARTESIAN_POINT('Ctrl Pts',(7.29604661499953,-4.51683969204717,-1.25384772750642));
#58769=CARTESIAN_POINT('Ctrl Pts',(7.28299669995026,-4.54214834917589,-1.2168886144726));
#58770=CARTESIAN_POINT('Ctrl Pts',(7.26978169876728,-4.56732248175787,-1.17989436424469));
#58771=CARTESIAN_POINT('Ctrl Pts',(7.40504161293288,-4.4667399727747,-1.24024771661909));
#58772=CARTESIAN_POINT('Ctrl Pts',(7.39215976633109,-4.49218820179592,-1.20332617953064));
#58773=CARTESIAN_POINT('Ctrl Pts',(7.37905001527746,-4.51744716993401,-1.16635368976618));
#58774=CARTESIAN_POINT('Ctrl Pts',(7.36571703908252,-4.54252423750733,-1.1293336884092));
#58775=CARTESIAN_POINT('Ctrl Pts',(7.50115524253438,-4.44208887850051,-1.18972627474503));
#58776=CARTESIAN_POINT('Ctrl Pts',(7.48827291766266,-4.46753671154468,-1.15280463155487));
#58777=CARTESIAN_POINT('Ctrl Pts',(7.47510333060465,-4.49274599069213,-1.11581876505976));
#58778=CARTESIAN_POINT('Ctrl Pts',(7.46165237939775,-4.51772599325679,-1.07877301257371));
#58779=CARTESIAN_POINT('Ctrl Pts',(7.49999999999088,-4.44238517355363,-1.1903335197214));
#58780=CARTESIAN_POINT('Ctrl Pts',(7.49999999570487,-4.44304670138692,-1.18902822733552));
#58781=CARTESIAN_POINT('Ctrl Pts',(7.50000000037144,-4.4437079006456,-1.1877228334994));
#58782=CARTESIAN_POINT('Ctrl Pts',(7.50000000105118,-4.44436879327611,-1.18641730372799));
#58783=CARTESIAN_POINT('Ctrl Pts',(7.2128143537299,-3.24036193608375,-3.41961281443685));
#58784=CARTESIAN_POINT('Ctrl Pts',(7.19993346366797,-3.28086209719235,-3.4003625196327));
#58785=CARTESIAN_POINT('Ctrl Pts',(7.18694338462306,-3.32129593728126,-3.38104574649231));
#58786=CARTESIAN_POINT('Ctrl Pts',(7.17384635845203,-3.36166568592822,-3.36166568592825));
#58787=CARTESIAN_POINT('Ctrl Pts',(7.30892798333139,-3.24427418314825,-3.36353441520099));
#58788=CARTESIAN_POINT('Ctrl Pts',(7.29604661499953,-3.28477405438151,-3.34428383052154));
#58789=CARTESIAN_POINT('Ctrl Pts',(7.28299669995025,-3.32517155090757,-3.32493062829727));
#58790=CARTESIAN_POINT('Ctrl Pts',(7.26978169876727,-3.36547011435575,-3.30547973409693));
#58791=CARTESIAN_POINT('Ctrl Pts',(7.40504161293289,-3.24818643021274,-3.30745601596514));
#58792=CARTESIAN_POINT('Ctrl Pts',(7.3921597663311,-3.28868601157068,-3.28820514141038));
#58793=CARTESIAN_POINT('Ctrl Pts',(7.37905001527746,-3.32904716453387,-3.26881551010224));
#58794=CARTESIAN_POINT('Ctrl Pts',(7.36571703908251,-3.36927454278328,-3.24929378226561));
#58795=CARTESIAN_POINT('Ctrl Pts',(7.50115524253438,-3.25209867727724,-3.25137761672928));
#58796=CARTESIAN_POINT('Ctrl Pts',(7.48827291766266,-3.29259796875984,-3.23212645229922));
#58797=CARTESIAN_POINT('Ctrl Pts',(7.47510333060465,-3.33292277816018,-3.2127003919072));
#58798=CARTESIAN_POINT('Ctrl Pts',(7.46165237939775,-3.37307897121081,-3.1931078304343));
#58799=CARTESIAN_POINT('',(7.49999999999943,-3.25572762720846,-3.2496519225041));
#58800=CARTESIAN_POINT('Ctrl Pts',(7.49999999999097,-3.25205165383206,-3.25205165383167));
#58801=CARTESIAN_POINT('Ctrl Pts',(7.49999999570083,-3.25327719982305,-3.25125200145742));
#58802=CARTESIAN_POINT('Ctrl Pts',(7.50000000037144,-3.25450251208352,-3.25045209686877));
#58803=CARTESIAN_POINT('Ctrl Pts',(7.50000000105118,-3.25572762689991,-3.24965192115593));
#58804=CARTESIAN_POINT('Ctrl Pts',(7.50000000105064,-3.2557276269016,-3.24965192115513));
#58805=CARTESIAN_POINT('Ctrl Pts',(7.48748585582718,-3.29500700498933,-3.23096570291725));
#58806=CARTESIAN_POINT('Ctrl Pts',(7.47470152024076,-3.33412233455541,-3.21211511774079));
#58807=CARTESIAN_POINT('Ctrl Pts',(7.46165237939775,-3.37307897121081,-3.1931078304343));
#58808=CARTESIAN_POINT('Ctrl Pts',(7.21281435372989,-1.09642934688624,-4.58165253645099));
#58809=CARTESIAN_POINT('Ctrl Pts',(7.19993346366796,-1.14112866266571,-4.58523137267456));
#58810=CARTESIAN_POINT('Ctrl Pts',(7.18694338462305,-1.18580378192547,-4.5887194764603));
#58811=CARTESIAN_POINT('Ctrl Pts',(7.17384635845202,-1.23045504008016,-4.59212072600842));
#58812=CARTESIAN_POINT('Ctrl Pts',(7.30892798333139,-1.1278566518479,-4.53504334164142));
#58813=CARTESIAN_POINT('Ctrl Pts',(7.29604661499952,-1.17255586152563,-4.53862178188795));
#58814=CARTESIAN_POINT('Ctrl Pts',(7.28299669995025,-1.21721772087862,-4.54206016538018));
#58815=CARTESIAN_POINT('Ctrl Pts',(7.26978169876727,-1.26184274766094,-4.54536447860045));
#58816=CARTESIAN_POINT('Ctrl Pts',(7.40504161293288,-1.15928395680956,-4.48843414683185));
#58817=CARTESIAN_POINT('Ctrl Pts',(7.39215976633109,-1.20398306038554,-4.49201219110133));
#58818=CARTESIAN_POINT('Ctrl Pts',(7.37905001527745,-1.24863165983177,-4.49540085430006));
#58819=CARTESIAN_POINT('Ctrl Pts',(7.36571703908251,-1.29323045524171,-4.49860823119249));
#58820=CARTESIAN_POINT('Ctrl Pts',(7.50115524253438,-1.19071126177122,-4.44182495202228));
#58821=CARTESIAN_POINT('Ctrl Pts',(7.48827291766266,-1.23541025924546,-4.44540260031471));
#58822=CARTESIAN_POINT('Ctrl Pts',(7.47510333060465,-1.28004559878492,-4.44874154321995));
#58823=CARTESIAN_POINT('Ctrl Pts',(7.46165237939775,-1.32461816282249,-4.45185198378452));
#58824=CARTESIAN_POINT('',(7.49999999999943,-1.1947168717133,-4.44214493194972));
#58825=CARTESIAN_POINT('Ctrl Pts',(7.49999999999097,-1.19033351972193,-4.44238517355345));
#58826=CARTESIAN_POINT('Ctrl Pts',(7.49999999569755,-1.19179469976444,-4.44230542728599));
#58827=CARTESIAN_POINT('Ctrl Pts',(7.50000000037144,-1.1932558035927,-4.44222534572098));
#58828=CARTESIAN_POINT('Ctrl Pts',(7.50000000105118,-1.19471687212018,-4.4421449306279));
#58829=CARTESIAN_POINT('Ctrl Pts',(7.50000000105064,-1.19471687212205,-4.44214493062805));
#58830=CARTESIAN_POINT('Ctrl Pts',(7.48748585582718,-1.23807692050981,-4.44560187997725));
#58831=CARTESIAN_POINT('Ctrl Pts',(7.47470152024076,-1.28137708217967,-4.44883445912128));
#58832=CARTESIAN_POINT('Ctrl Pts',(7.46165237939775,-1.32461816282249,-4.45185198378452));
#58833=CARTESIAN_POINT('Ctrl Pts',(7.21281435372989,1.34129060036722,-4.51604216132309));
#58834=CARTESIAN_POINT('Ctrl Pts',(7.19993346366796,1.3043692754822,-4.54149118229842));
#58835=CARTESIAN_POINT('Ctrl Pts',(7.18694338462305,1.26742353917902,-4.56684952841778));
#58836=CARTESIAN_POINT('Ctrl Pts',(7.17384635845203,1.23045504008019,-4.59212072600841));
#58837=CARTESIAN_POINT('Ctrl Pts',(7.30892798333139,1.29076915849316,-4.4913910670489));
#58838=CARTESIAN_POINT('Ctrl Pts',(7.29604661499953,1.25384772750642,-4.51683969204717));
#58839=CARTESIAN_POINT('Ctrl Pts',(7.28299669995025,1.2168886144726,-4.5421483491759));
#58840=CARTESIAN_POINT('Ctrl Pts',(7.26978169876727,1.17989436424469,-4.56732248175787));
#58841=CARTESIAN_POINT('Ctrl Pts',(7.40504161293288,1.24024771661909,-4.4667399727747));
#58842=CARTESIAN_POINT('Ctrl Pts',(7.39215976633109,1.20332617953064,-4.49218820179592));
#58843=CARTESIAN_POINT('Ctrl Pts',(7.37905001527745,1.16635368976618,-4.51744716993401));
#58844=CARTESIAN_POINT('Ctrl Pts',(7.36571703908251,1.1293336884092,-4.54252423750733));
#58845=CARTESIAN_POINT('Ctrl Pts',(7.50115524253438,1.18972627474503,-4.44208887850051));
#58846=CARTESIAN_POINT('Ctrl Pts',(7.48827291766266,1.15280463155486,-4.46753671154468));
#58847=CARTESIAN_POINT('Ctrl Pts',(7.47510333060465,1.11581876505976,-4.49274599069213));
#58848=CARTESIAN_POINT('Ctrl Pts',(7.46165237939775,1.07877301257371,-4.51772599325679));
#58849=CARTESIAN_POINT('',(7.49999999999943,1.18641730474126,-4.44436879421741));
#58850=CARTESIAN_POINT('Ctrl Pts',(7.49999999999088,1.19033351972139,-4.44238517355364));
#58851=CARTESIAN_POINT('Ctrl Pts',(7.49999999570486,1.18902822733552,-4.44304670138692));
#58852=CARTESIAN_POINT('Ctrl Pts',(7.50000000037144,1.1877228334994,-4.4437079006456));
#58853=CARTESIAN_POINT('Ctrl Pts',(7.50000000105118,1.18641730372799,-4.44436879327611));
#58854=CARTESIAN_POINT('Ctrl Pts',(7.50000000105064,1.18641730372645,-4.44436879327718));
#58855=CARTESIAN_POINT('Ctrl Pts',(7.48748585582718,1.15059487498792,-4.46904262342707));
#58856=CARTESIAN_POINT('Ctrl Pts',(7.47470152024076,1.11471212456586,-4.49349219992046));
#58857=CARTESIAN_POINT('Ctrl Pts',(7.46165237939775,1.07877301257371,-4.51772599325679));
#58858=CARTESIAN_POINT('Ctrl Pts',(7.21281435372989,3.41961281443685,-3.24036193608376));
#58859=CARTESIAN_POINT('Ctrl Pts',(7.19993346366796,3.4003625196327,-3.28086209719235));
#58860=CARTESIAN_POINT('Ctrl Pts',(7.18694338462305,3.38104574649231,-3.32129593728127));
#58861=CARTESIAN_POINT('Ctrl Pts',(7.17384635845203,3.36166568592825,-3.36166568592822));
#58862=CARTESIAN_POINT('Ctrl Pts',(7.30892798333139,3.36353441520099,-3.24427418314825));
#58863=CARTESIAN_POINT('Ctrl Pts',(7.29604661499953,3.34428383052154,-3.28477405438151));
#58864=CARTESIAN_POINT('Ctrl Pts',(7.28299669995025,3.32493062829727,-3.32517155090757));
#58865=CARTESIAN_POINT('Ctrl Pts',(7.26978169876727,3.30547973409693,-3.36547011435575));
#58866=CARTESIAN_POINT('Ctrl Pts',(7.40504161293288,3.30745601596514,-3.24818643021275));
#58867=CARTESIAN_POINT('Ctrl Pts',(7.39215976633109,3.28820514141038,-3.28868601157068));
#58868=CARTESIAN_POINT('Ctrl Pts',(7.37905001527745,3.26881551010224,-3.32904716453388));
#58869=CARTESIAN_POINT('Ctrl Pts',(7.36571703908251,3.24929378226561,-3.36927454278328));
#58870=CARTESIAN_POINT('Ctrl Pts',(7.50115524253438,3.25137761672928,-3.25209867727724));
#58871=CARTESIAN_POINT('Ctrl Pts',(7.48827291766266,3.23212645229921,-3.29259796875984));
#58872=CARTESIAN_POINT('Ctrl Pts',(7.47510333060465,3.2127003919072,-3.33292277816018));
#58873=CARTESIAN_POINT('Ctrl Pts',(7.46165237939775,3.1931078304343,-3.37307897121081));
#58874=CARTESIAN_POINT('',(7.49999999999943,3.2496519225041,-3.25572762720846));
#58875=CARTESIAN_POINT('Ctrl Pts',(7.49999999999096,3.25205165383167,-3.25205165383206));
#58876=CARTESIAN_POINT('Ctrl Pts',(7.49999999570083,3.25125200145742,-3.25327719982305));
#58877=CARTESIAN_POINT('Ctrl Pts',(7.50000000037144,3.25045209686877,-3.25450251208352));
#58878=CARTESIAN_POINT('Ctrl Pts',(7.50000000105118,3.24965192115593,-3.25572762689991));
#58879=CARTESIAN_POINT('Ctrl Pts',(7.50000000105064,3.24965192115513,-3.2557276269016));
#58880=CARTESIAN_POINT('Ctrl Pts',(7.48748585582718,3.23096570291725,-3.29500700498933));
#58881=CARTESIAN_POINT('Ctrl Pts',(7.47470152024076,3.21211511774079,-3.33412233455541));
#58882=CARTESIAN_POINT('Ctrl Pts',(7.46165237939775,3.1931078304343,-3.37307897121081));
#58883=CARTESIAN_POINT('Ctrl Pts',(7.21281435372989,4.58165253645099,-1.09642934688623));
#58884=CARTESIAN_POINT('Ctrl Pts',(7.19993346366796,4.58523137267456,-1.14112866266571));
#58885=CARTESIAN_POINT('Ctrl Pts',(7.18694338462305,4.58871947646029,-1.18580378192547));
#58886=CARTESIAN_POINT('Ctrl Pts',(7.17384635845203,4.59212072600842,-1.23045504008016));
#58887=CARTESIAN_POINT('Ctrl Pts',(7.30892798333139,4.53504334164142,-1.1278566518479));
#58888=CARTESIAN_POINT('Ctrl Pts',(7.29604661499953,4.53862178188794,-1.17255586152563));
#58889=CARTESIAN_POINT('Ctrl Pts',(7.28299669995025,4.54206016538018,-1.21721772087862));
#58890=CARTESIAN_POINT('Ctrl Pts',(7.26978169876727,4.54536447860045,-1.26184274766094));
#58891=CARTESIAN_POINT('Ctrl Pts',(7.40504161293289,4.48843414683185,-1.15928395680956));
#58892=CARTESIAN_POINT('Ctrl Pts',(7.39215976633109,4.49201219110133,-1.20398306038554));
#58893=CARTESIAN_POINT('Ctrl Pts',(7.37905001527745,4.49540085430006,-1.24863165983177));
#58894=CARTESIAN_POINT('Ctrl Pts',(7.36571703908251,4.49860823119249,-1.29323045524171));
#58895=CARTESIAN_POINT('Ctrl Pts',(7.50115524253438,4.44182495202228,-1.19071126177122));
#58896=CARTESIAN_POINT('Ctrl Pts',(7.48827291766266,4.44540260031471,-1.23541025924545));
#58897=CARTESIAN_POINT('Ctrl Pts',(7.47510333060465,4.44874154321995,-1.28004559878492));
#58898=CARTESIAN_POINT('Ctrl Pts',(7.46165237939775,4.45185198378452,-1.32461816282249));
#58899=CARTESIAN_POINT('',(7.49999999999943,4.44214493194972,-1.19471687171331));
#58900=CARTESIAN_POINT('Ctrl Pts',(7.49999999999096,4.44238517355345,-1.19033351972193));
#58901=CARTESIAN_POINT('Ctrl Pts',(7.49999999569755,4.44230542728599,-1.19179469976444));
#58902=CARTESIAN_POINT('Ctrl Pts',(7.50000000037144,4.44222534572098,-1.1932558035927));
#58903=CARTESIAN_POINT('Ctrl Pts',(7.50000000105118,4.4421449306279,-1.19471687212018));
#58904=CARTESIAN_POINT('Ctrl Pts',(7.50000000105064,4.44214493062805,-1.19471687212205));
#58905=CARTESIAN_POINT('Ctrl Pts',(7.48748585582718,4.44560187997725,-1.23807692050981));
#58906=CARTESIAN_POINT('Ctrl Pts',(7.47470152024076,4.44883445912128,-1.28137708217967));
#58907=CARTESIAN_POINT('Ctrl Pts',(7.46165237939775,4.45185198378452,-1.32461816282249));
#58908=CARTESIAN_POINT('Origin',(1.5,-1.01951846029017E-15,-5.55));
#58909=CARTESIAN_POINT('',(1.6,2.49998034634996,-3.8267625540171));
#58910=CARTESIAN_POINT('Origin',(1.5,-2.775,-4.80644099100363));
#58911=CARTESIAN_POINT('',(1.6,0.558573497940197,-4.53948635285801));
#58912=CARTESIAN_POINT('Origin',(1.5,-4.80644099100363,-2.775));
#58913=CARTESIAN_POINT('',(1.6,-1.93611308191135,-4.13925137399521));
#58914=CARTESIAN_POINT('Origin',(1.5,-5.55,6.79678973526781E-16));
#58915=CARTESIAN_POINT('',(1.6,-4.08446337701807,-2.12612183123792));
#58916=CARTESIAN_POINT('Origin',(7.5,0.,0.));
#58917=CARTESIAN_POINT('Origin',(7.5,0.,0.));
#58918=CARTESIAN_POINT('Origin',(7.5,0.,0.));
#58919=CARTESIAN_POINT('Origin',(7.5,0.,0.));
#58920=CARTESIAN_POINT('Origin',(7.5,0.,0.));
#58921=CARTESIAN_POINT('Origin',(7.5,0.,0.));
#58922=CARTESIAN_POINT('Origin',(7.5,0.,0.));
#58923=CARTESIAN_POINT('Origin',(7.5,0.,0.));
#58924=CARTESIAN_POINT('Origin',(7.5,0.,0.));
#58925=CARTESIAN_POINT('',(7.5,-3.95,4.83735485663205E-16));
#58926=CARTESIAN_POINT('Origin',(7.5,0.,0.));
#58927=CARTESIAN_POINT('Origin',(6.9,0.,0.));
#58928=CARTESIAN_POINT('Origin',(6.9,0.,0.));
#58929=CARTESIAN_POINT('Origin',(6.9,0.,0.));
#58930=CARTESIAN_POINT('Origin',(6.9,0.,0.));
#58931=CARTESIAN_POINT('Origin',(6.9,0.,0.));
#58932=CARTESIAN_POINT('Origin',(6.9,0.,0.));
#58933=CARTESIAN_POINT('Origin',(6.9,0.,0.));
#58934=CARTESIAN_POINT('Origin',(6.9,0.,0.));
#58935=CARTESIAN_POINT('Origin',(7.35,0.,0.));
#58936=CARTESIAN_POINT('',(7.1,-3.55,-4.3474961369731E-16));
#58937=CARTESIAN_POINT('Origin',(7.1,0.,0.));
#58938=CARTESIAN_POINT('',(7.35,-3.8,-4.65365783675994E-16));
#58939=CARTESIAN_POINT('Origin',(0.15,0.,0.));
#58940=CARTESIAN_POINT('',(0.,-3.95,-4.83735485663205E-16));
#58941=CARTESIAN_POINT('Origin',(0.,0.,0.));
#58942=CARTESIAN_POINT('',(0.400000000000001,-3.55,-4.3474961369731E-16));
#58943=CARTESIAN_POINT('',(0.15,-3.8,-4.65365783675994E-16));
#58944=CARTESIAN_POINT('Origin',(0.4,0.,0.));
#58945=CARTESIAN_POINT('Origin',(1.5,4.80644099100363,-2.775));
#58946=CARTESIAN_POINT('',(1.6,4.69203409014831,-1.34635348791082));
#58947=CARTESIAN_POINT('Origin',(1.5,2.775,-4.80644099100363));
#58948=CARTESIAN_POINT('',(1.6,3.77815762639755,-2.69583924476141));
#58949=CARTESIAN_POINT('Origin',(1.5,-4.80644099100363,2.775));
#58950=CARTESIAN_POINT('',(1.6,-4.66941333870903,1.06387876476949));
#58951=CARTESIAN_POINT('Origin',(1.5,-2.775,4.80644099100363));
#58952=CARTESIAN_POINT('',(1.6,-3.12397753684527,4.07220682950901));
#58953=CARTESIAN_POINT('Origin',(1.5,3.3983948676339E-16,5.55));
#58954=CARTESIAN_POINT('',(1.6,-0.0934210082369602,5.48560486190603));
#58955=CARTESIAN_POINT('Origin',(1.5,2.775,4.80644099100363));
#58956=CARTESIAN_POINT('',(1.6,2.96880575062052,4.82196107599933));
#58957=CARTESIAN_POINT('Origin',(1.5,4.80644099100363,2.775));
#58958=CARTESIAN_POINT('',(1.6,4.83193299235907,2.76288378924761));
#58959=CARTESIAN_POINT('Origin',(1.5,5.55,0.));
#58960=CARTESIAN_POINT('',(1.6,5.22790403890507,0.467279523348994));
#58961=CARTESIAN_POINT('Origin',(0.8,0.,0.));
#58962=CARTESIAN_POINT('',(0.8,-3.55,-4.3474961369731E-16));
#58963=CARTESIAN_POINT('Origin',(0.,6.2,0.));
#58964=CARTESIAN_POINT('',(-3.46944695195361E-17,-6.2,-7.59281015471359E-16));
#58965=CARTESIAN_POINT('Origin',(0.,0.,0.));
#58966=CARTESIAN_POINT('Origin',(0.15,0.,0.));
#58967=CARTESIAN_POINT('',(0.3,-6.5,-7.9602041944578E-16));
#58968=CARTESIAN_POINT('Origin',(0.3,0.,0.));
#58969=CARTESIAN_POINT('',(0.15,-6.35,-7.77650717458569E-16));
#58970=CARTESIAN_POINT('Origin',(0.85,0.,0.));
#58971=CARTESIAN_POINT('',(1.4,-6.5,-7.9602041944578E-16));
#58972=CARTESIAN_POINT('Origin',(1.4,0.,0.));
#58973=CARTESIAN_POINT('',(0.85,-6.5,-7.9602041944578E-16));
#58974=CARTESIAN_POINT('Origin',(1.5,0.,0.));
#58975=CARTESIAN_POINT('',(1.6,-6.,-7.34788079488412E-16));
#58976=CARTESIAN_POINT('Origin',(1.6,0.,0.));
#58977=CARTESIAN_POINT('',(1.5,-6.25,-7.65404249467096E-16));
#58978=CARTESIAN_POINT('Origin',(1.6,3.55,0.));
#58979=CARTESIAN_POINT('',(0.,0.,0.));
#58980=CARTESIAN_POINT('Origin',(0.8,3.90322943214974,-3.90322943214974));
#58981=CARTESIAN_POINT('',(0.8,3.45653456843748,-4.3038086362194));
#58982=CARTESIAN_POINT('',(0.8,4.3038086362194,-3.45653456843748));
#58983=CARTESIAN_POINT('Origin',(0.8,0.,0.));
#58984=CARTESIAN_POINT('Origin',(0.8,3.90322943214974,-3.90322943214974));
#58985=CARTESIAN_POINT('Origin',(0.8,3.90322943214974,-3.90322943214974));
#58986=CARTESIAN_POINT('',(9.7,3.45653456843748,-4.3038086362194));
#58987=CARTESIAN_POINT('',(0.8,3.45653456843748,-4.3038086362194));
#58988=CARTESIAN_POINT('',(9.7,4.3038086362194,-3.45653456843748));
#58989=CARTESIAN_POINT('Origin',(9.7,3.90322943214974,-3.90322943214974));
#58990=CARTESIAN_POINT('',(0.8,4.3038086362194,-3.45653456843748));
#58991=CARTESIAN_POINT('Origin',(9.7,3.90322943214974,-3.90322943214974));
#58992=CARTESIAN_POINT('Origin',(9.7,0.,0.));
#58993=CARTESIAN_POINT('Origin',(0.8,-3.90322943214974,-3.90322943214974));
#58994=CARTESIAN_POINT('',(0.8,-4.3038086362194,-3.45653456843748));
#58995=CARTESIAN_POINT('',(0.8,-3.45653456843748,-4.3038086362194));
#58996=CARTESIAN_POINT('Origin',(0.8,0.,0.));
#58997=CARTESIAN_POINT('Origin',(0.8,-3.90322943214974,-3.90322943214974));
#58998=CARTESIAN_POINT('Origin',(0.8,-3.90322943214974,-3.90322943214974));
#58999=CARTESIAN_POINT('',(9.7,-4.3038086362194,-3.45653456843748));
#59000=CARTESIAN_POINT('',(0.8,-4.3038086362194,-3.45653456843748));
#59001=CARTESIAN_POINT('',(9.7,-3.45653456843748,-4.3038086362194));
#59002=CARTESIAN_POINT('Origin',(9.7,-3.90322943214974,-3.90322943214974));
#59003=CARTESIAN_POINT('',(0.8,-3.45653456843748,-4.3038086362194));
#59004=CARTESIAN_POINT('Origin',(9.7,-3.90322943214974,-3.90322943214974));
#59005=CARTESIAN_POINT('Origin',(9.7,0.,0.));
#59006=CARTESIAN_POINT('Origin',(0.8,-3.90322943214974,3.90322943214974));
#59007=CARTESIAN_POINT('',(0.8,-3.45653456843748,4.3038086362194));
#59008=CARTESIAN_POINT('',(0.8,-4.3038086362194,3.45653456843748));
#59009=CARTESIAN_POINT('Origin',(0.8,0.,0.));
#59010=CARTESIAN_POINT('Origin',(0.8,-3.90322943214974,3.90322943214974));
#59011=CARTESIAN_POINT('Origin',(0.8,-3.90322943214974,3.90322943214974));
#59012=CARTESIAN_POINT('',(9.7,-3.45653456843748,4.3038086362194));
#59013=CARTESIAN_POINT('',(0.8,-3.45653456843748,4.3038086362194));
#59014=CARTESIAN_POINT('',(9.7,-4.3038086362194,3.45653456843748));
#59015=CARTESIAN_POINT('Origin',(9.7,-3.90322943214974,3.90322943214974));
#59016=CARTESIAN_POINT('',(0.8,-4.3038086362194,3.45653456843748));
#59017=CARTESIAN_POINT('Origin',(9.7,-3.90322943214974,3.90322943214974));
#59018=CARTESIAN_POINT('Origin',(9.7,0.,0.));
#59019=CARTESIAN_POINT('Origin',(0.8,3.90322943214974,3.90322943214974));
#59020=CARTESIAN_POINT('',(0.8,4.3038086362194,3.45653456843748));
#59021=CARTESIAN_POINT('',(0.8,3.45653456843748,4.3038086362194));
#59022=CARTESIAN_POINT('Origin',(0.8,0.,0.));
#59023=CARTESIAN_POINT('Origin',(0.8,3.90322943214974,3.90322943214974));
#59024=CARTESIAN_POINT('Origin',(0.8,3.90322943214974,3.90322943214974));
#59025=CARTESIAN_POINT('',(9.7,4.3038086362194,3.45653456843748));
#59026=CARTESIAN_POINT('',(0.8,4.3038086362194,3.45653456843748));
#59027=CARTESIAN_POINT('',(9.7,3.45653456843748,4.3038086362194));
#59028=CARTESIAN_POINT('Origin',(9.7,3.90322943214974,3.90322943214974));
#59029=CARTESIAN_POINT('',(0.8,3.45653456843748,4.3038086362194));
#59030=CARTESIAN_POINT('Origin',(9.7,3.90322943214974,3.90322943214974));
#59031=CARTESIAN_POINT('Origin',(9.7,0.,0.));
#59032=CARTESIAN_POINT('Origin',(5.25,8.45,-1.55223981791927E-15));
#59033=CARTESIAN_POINT('',(6.35,8.45,-1.55223981791927E-15));
#59034=CARTESIAN_POINT('',(4.15,8.45,-1.41752867001306E-15));
#59035=CARTESIAN_POINT('Ctrl Pts',(6.35,8.45,-1.70002900645727E-15));
#59036=CARTESIAN_POINT('Ctrl Pts',(6.35,8.45,0.138286410729708));
#59037=CARTESIAN_POINT('Ctrl Pts',(6.32233132681,8.44625875235353,0.285683724538777));
#59038=CARTESIAN_POINT('Ctrl Pts',(6.21002324830763,8.4327360375918,0.556655210212817));
#59039=CARTESIAN_POINT('Ctrl Pts',(6.12539248344495,8.42314504656407,0.680242435165457));
#59040=CARTESIAN_POINT('Ctrl Pts',(5.93024147512979,8.40510492225533,0.875393443480616));
#59041=CARTESIAN_POINT('Ctrl Pts',(5.80665466688422,8.39547821560232,0.96002345589192));
#59042=CARTESIAN_POINT('Ctrl Pts',(5.53568459489851,8.381873644329,1.07233098368286));
#59043=CARTESIAN_POINT('Ctrl Pts',(5.38828777132263,8.37809644251008,1.1));
#59044=CARTESIAN_POINT('Ctrl Pts',(5.11171222867737,8.37809644251008,1.1));
#59045=CARTESIAN_POINT('Ctrl Pts',(4.96431540510149,8.381873644329,1.07233098368286));
#59046=CARTESIAN_POINT('Ctrl Pts',(4.69334533311577,8.39547821560232,0.960023455891919));
#59047=CARTESIAN_POINT('Ctrl Pts',(4.56975852487021,8.40510492225533,0.875393443480615));
#59048=CARTESIAN_POINT('Ctrl Pts',(4.37460751655505,8.42314504656407,0.680242435165457));
#59049=CARTESIAN_POINT('Ctrl Pts',(4.28997675169238,8.4327360375918,0.556655210212818));
#59050=CARTESIAN_POINT('Ctrl Pts',(4.17766867319,8.44625875235353,0.285683724538777));
#59051=CARTESIAN_POINT('Ctrl Pts',(4.15,8.45,0.138286410729708));
#59052=CARTESIAN_POINT('Ctrl Pts',(4.15,8.45,-1.42247325030098E-15));
#59053=CARTESIAN_POINT('Ctrl Pts',(4.15,8.45,-1.45716771982052E-15));
#59054=CARTESIAN_POINT('Ctrl Pts',(4.15,8.45,-0.138286410729711));
#59055=CARTESIAN_POINT('Ctrl Pts',(4.17766867319,8.44625875235353,-0.28568372453878));
#59056=CARTESIAN_POINT('Ctrl Pts',(4.28997675169238,8.4327360375918,-0.556655210212821));
#59057=CARTESIAN_POINT('Ctrl Pts',(4.37460751655505,8.42314504656407,-0.68024243516546));
#59058=CARTESIAN_POINT('Ctrl Pts',(4.56975852487021,8.40510492225533,-0.875393443480618));
#59059=CARTESIAN_POINT('Ctrl Pts',(4.69334533311577,8.39547821560232,-0.960023455891922));
#59060=CARTESIAN_POINT('Ctrl Pts',(4.96431540510148,8.381873644329,-1.07233098368286));
#59061=CARTESIAN_POINT('Ctrl Pts',(5.11171222867737,8.37809644251008,-1.1));
#59062=CARTESIAN_POINT('Ctrl Pts',(5.25,8.37809644251008,-1.1));
#59063=CARTESIAN_POINT('Ctrl Pts',(5.38828777132263,8.37809644251008,-1.1));
#59064=CARTESIAN_POINT('Ctrl Pts',(5.53568459489851,8.381873644329,-1.07233098368286));
#59065=CARTESIAN_POINT('Ctrl Pts',(5.80665466688422,8.39547821560232,-0.960023455891923));
#59066=CARTESIAN_POINT('Ctrl Pts',(5.93024147512979,8.40510492225533,-0.875393443480619));
#59067=CARTESIAN_POINT('Ctrl Pts',(6.12539248344495,8.42314504656407,-0.68024243516546));
#59068=CARTESIAN_POINT('Ctrl Pts',(6.21002324830763,8.4327360375918,-0.556655210212821));
#59069=CARTESIAN_POINT('Ctrl Pts',(6.32233132681,8.44625875235353,-0.285683724538781));
#59070=CARTESIAN_POINT('Ctrl Pts',(6.35,8.45,-0.138286410729711));
#59071=CARTESIAN_POINT('Ctrl Pts',(6.35,8.45,-1.59594559789866E-15));
#59072=CARTESIAN_POINT('',(4.15,5.52,-1.14681809587245E-15));
#59073=CARTESIAN_POINT('',(4.15,8.45,-1.68695096582548E-15));
#59074=CARTESIAN_POINT('',(5.25,5.40928830808638,-1.1));
#59075=CARTESIAN_POINT('Ctrl Pts',(5.25,5.40928830808638,-1.1));
#59076=CARTESIAN_POINT('Ctrl Pts',(5.11147809944016,5.40928830808638,-1.1));
#59077=CARTESIAN_POINT('Ctrl Pts',(4.9639846961023,5.41516098360831,-1.07224024467438));
#59078=CARTESIAN_POINT('Ctrl Pts',(4.69308215533071,5.43620465823388,-0.959867948076927));
#59079=CARTESIAN_POINT('Ctrl Pts',(4.569639996971,5.45105349297774,-0.875274915581407));
#59080=CARTESIAN_POINT('Ctrl Pts',(4.37473046520206,5.47879477947926,-0.68036538381247));
#59081=CARTESIAN_POINT('Ctrl Pts',(4.29013321807171,5.4935138828468,-0.556920939780125));
#59082=CARTESIAN_POINT('Ctrl Pts',(4.17775786268853,5.51425912806026,-0.286010457396549));
#59083=CARTESIAN_POINT('Ctrl Pts',(4.15,5.52,-0.138514252542119));
#59084=CARTESIAN_POINT('Ctrl Pts',(4.15,5.52,-1.17961196366423E-15));
#59085=CARTESIAN_POINT('Ctrl Pts',(4.15,5.52,-1.21430643318376E-15));
#59086=CARTESIAN_POINT('Ctrl Pts',(4.15,5.52,0.138514252542116));
#59087=CARTESIAN_POINT('Ctrl Pts',(4.17775786268853,5.51425912806026,0.286010457396547));
#59088=CARTESIAN_POINT('Ctrl Pts',(4.29013321807171,5.4935138828468,0.556920939780123));
#59089=CARTESIAN_POINT('Ctrl Pts',(4.37473046520206,5.47879477947926,0.680365383812468));
#59090=CARTESIAN_POINT('Ctrl Pts',(4.569639996971,5.45105349297774,0.875274915581405));
#59091=CARTESIAN_POINT('Ctrl Pts',(4.69308215533071,5.43620465823388,0.959867948076925));
#59092=CARTESIAN_POINT('Ctrl Pts',(4.9639846961023,5.41516098360831,1.07224024467438));
#59093=CARTESIAN_POINT('Ctrl Pts',(5.11147809944016,5.40928830808638,1.1));
#59094=CARTESIAN_POINT('Ctrl Pts',(5.38852190055984,5.40928830808638,1.1));
#59095=CARTESIAN_POINT('Ctrl Pts',(5.5360153038977,5.41516098360831,1.07224024467438));
#59096=CARTESIAN_POINT('Ctrl Pts',(5.80691784466929,5.43620465823388,0.959867948076925));
#59097=CARTESIAN_POINT('Ctrl Pts',(5.930360003029,5.45105349297774,0.875274915581405));
#59098=CARTESIAN_POINT('Ctrl Pts',(6.12526953479794,5.47879477947926,0.680365383812468));
#59099=CARTESIAN_POINT('Ctrl Pts',(6.20986678192829,5.4935138828468,0.556920939780123));
#59100=CARTESIAN_POINT('Ctrl Pts',(6.32224213731147,5.51425912806026,0.286010457396547));
#59101=CARTESIAN_POINT('Ctrl Pts',(6.35,5.52,0.138514252542117));
#59102=CARTESIAN_POINT('Ctrl Pts',(6.35,5.52,-0.138514252542118));
#59103=CARTESIAN_POINT('Ctrl Pts',(6.32224213731147,5.51425912806026,-0.286010457396548));
#59104=CARTESIAN_POINT('Ctrl Pts',(6.20986678192829,5.4935138828468,-0.556920939780125));
#59105=CARTESIAN_POINT('Ctrl Pts',(6.12526953479794,5.47879477947926,-0.68036538381247));
#59106=CARTESIAN_POINT('Ctrl Pts',(5.930360003029,5.45105349297774,-0.875274915581407));
#59107=CARTESIAN_POINT('Ctrl Pts',(5.80691784466929,5.43620465823388,-0.959867948076927));
#59108=CARTESIAN_POINT('Ctrl Pts',(5.5360153038977,5.41516098360831,-1.07224024467438));
#59109=CARTESIAN_POINT('Ctrl Pts',(5.38852190055984,5.40928830808638,-1.1));
#59110=CARTESIAN_POINT('Ctrl Pts',(5.25,5.40928830808638,-1.1));
#59111=CARTESIAN_POINT('Origin',(5.25,-1.03482654527951E-15,-8.45));
#59112=CARTESIAN_POINT('',(6.35,-1.03482654527951E-15,-8.45));
#59113=CARTESIAN_POINT('',(4.15,-9.00115397373305E-16,-8.45));
#59114=CARTESIAN_POINT('Ctrl Pts',(6.35,-9.71445146547012E-16,-8.45));
#59115=CARTESIAN_POINT('Ctrl Pts',(6.35,0.138286410729709,-8.45));
#59116=CARTESIAN_POINT('Ctrl Pts',(6.32233132681,0.285683724538778,-8.44625875235353));
#59117=CARTESIAN_POINT('Ctrl Pts',(6.21002324830763,0.556655210212818,-8.4327360375918));
#59118=CARTESIAN_POINT('Ctrl Pts',(6.12539248344495,0.680242435165458,-8.42314504656407));
#59119=CARTESIAN_POINT('Ctrl Pts',(5.93024147512979,0.875393443480616,-8.40510492225533));
#59120=CARTESIAN_POINT('Ctrl Pts',(5.80665466688423,0.96002345589192,-8.39547821560232));
#59121=CARTESIAN_POINT('Ctrl Pts',(5.53568459489851,1.07233098368286,-8.381873644329));
#59122=CARTESIAN_POINT('Ctrl Pts',(5.38828777132263,1.1,-8.37809644251008));
#59123=CARTESIAN_POINT('Ctrl Pts',(5.11171222867737,1.1,-8.37809644251008));
#59124=CARTESIAN_POINT('Ctrl Pts',(4.96431540510149,1.07233098368286,-8.381873644329));
#59125=CARTESIAN_POINT('Ctrl Pts',(4.69334533311577,0.960023455891919,-8.39547821560232));
#59126=CARTESIAN_POINT('Ctrl Pts',(4.56975852487021,0.875393443480616,-8.40510492225533));
#59127=CARTESIAN_POINT('Ctrl Pts',(4.37460751655505,0.680242435165458,-8.42314504656407));
#59128=CARTESIAN_POINT('Ctrl Pts',(4.28997675169238,0.556655210212818,-8.4327360375918));
#59129=CARTESIAN_POINT('Ctrl Pts',(4.17766867319,0.285683724538778,-8.44625875235353));
#59130=CARTESIAN_POINT('Ctrl Pts',(4.15,0.138286410729709,-8.45));
#59131=CARTESIAN_POINT('Ctrl Pts',(4.15,-5.55111512312578E-16,-8.45));
#59132=CARTESIAN_POINT('Ctrl Pts',(4.15,-8.32667268468867E-16,-8.45));
#59133=CARTESIAN_POINT('Ctrl Pts',(4.15,-0.13828641072971,-8.45));
#59134=CARTESIAN_POINT('Ctrl Pts',(4.17766867319,-0.28568372453878,-8.44625875235353));
#59135=CARTESIAN_POINT('Ctrl Pts',(4.28997675169238,-0.55665521021282,-8.4327360375918));
#59136=CARTESIAN_POINT('Ctrl Pts',(4.37460751655505,-0.680242435165459,
-8.42314504656407));
#59137=CARTESIAN_POINT('Ctrl Pts',(4.56975852487021,-0.875393443480618,
-8.40510492225533));
#59138=CARTESIAN_POINT('Ctrl Pts',(4.69334533311577,-0.960023455891921,
-8.39547821560232));
#59139=CARTESIAN_POINT('Ctrl Pts',(4.96431540510148,-1.07233098368286,-8.381873644329));
#59140=CARTESIAN_POINT('Ctrl Pts',(5.11171222867737,-1.1,-8.37809644251008));
#59141=CARTESIAN_POINT('Ctrl Pts',(5.25,-1.1,-8.37809644251008));
#59142=CARTESIAN_POINT('Ctrl Pts',(5.38828777132263,-1.1,-8.37809644251008));
#59143=CARTESIAN_POINT('Ctrl Pts',(5.53568459489851,-1.07233098368286,-8.381873644329));
#59144=CARTESIAN_POINT('Ctrl Pts',(5.80665466688422,-0.960023455891922,
-8.39547821560232));
#59145=CARTESIAN_POINT('Ctrl Pts',(5.93024147512979,-0.875393443480618,
-8.40510492225533));
#59146=CARTESIAN_POINT('Ctrl Pts',(6.12539248344495,-0.68024243516546,-8.42314504656407));
#59147=CARTESIAN_POINT('Ctrl Pts',(6.21002324830763,-0.55665521021282,-8.4327360375918));
#59148=CARTESIAN_POINT('Ctrl Pts',(6.32233132681,-0.28568372453878,-8.44625875235353));
#59149=CARTESIAN_POINT('Ctrl Pts',(6.35,-0.138286410729711,-8.45));
#59150=CARTESIAN_POINT('Ctrl Pts',(6.35,-1.14491749414469E-15,-8.45));
#59151=CARTESIAN_POINT('',(4.15,-7.86997255232671E-16,-5.52));
#59152=CARTESIAN_POINT('',(4.15,-1.16953769318572E-15,-8.45));
#59153=CARTESIAN_POINT('',(5.25,-1.1,-5.40928830808638));
#59154=CARTESIAN_POINT('Ctrl Pts',(5.25,-1.1,-5.40928830808638));
#59155=CARTESIAN_POINT('Ctrl Pts',(5.11147809944016,-1.1,-5.40928830808638));
#59156=CARTESIAN_POINT('Ctrl Pts',(4.9639846961023,-1.07224024467438,-5.41516098360831));
#59157=CARTESIAN_POINT('Ctrl Pts',(4.69308215533071,-0.959867948076927,
-5.43620465823388));
#59158=CARTESIAN_POINT('Ctrl Pts',(4.569639996971,-0.875274915581407,-5.45105349297774));
#59159=CARTESIAN_POINT('Ctrl Pts',(4.37473046520206,-0.68036538381247,-5.47879477947926));
#59160=CARTESIAN_POINT('Ctrl Pts',(4.29013321807171,-0.556920939780125,
-5.4935138828468));
#59161=CARTESIAN_POINT('Ctrl Pts',(4.17775786268853,-0.286010457396548,
-5.51425912806026));
#59162=CARTESIAN_POINT('Ctrl Pts',(4.15,-0.138514252542118,-5.52));
#59163=CARTESIAN_POINT('Ctrl Pts',(4.15,-8.67361737988404E-16,-5.52));
#59164=CARTESIAN_POINT('Ctrl Pts',(4.15,-7.63278329429795E-16,-5.52));
#59165=CARTESIAN_POINT('Ctrl Pts',(4.15,0.138514252542117,-5.52));
#59166=CARTESIAN_POINT('Ctrl Pts',(4.17775786268853,0.286010457396547,-5.51425912806026));
#59167=CARTESIAN_POINT('Ctrl Pts',(4.29013321807171,0.556920939780123,-5.4935138828468));
#59168=CARTESIAN_POINT('Ctrl Pts',(4.37473046520206,0.680365383812468,-5.47879477947926));
#59169=CARTESIAN_POINT('Ctrl Pts',(4.569639996971,0.875274915581405,-5.45105349297774));
#59170=CARTESIAN_POINT('Ctrl Pts',(4.69308215533071,0.959867948076925,-5.43620465823388));
#59171=CARTESIAN_POINT('Ctrl Pts',(4.9639846961023,1.07224024467438,-5.41516098360831));
#59172=CARTESIAN_POINT('Ctrl Pts',(5.11147809944016,1.1,-5.40928830808638));
#59173=CARTESIAN_POINT('Ctrl Pts',(5.38852190055984,1.1,-5.40928830808638));
#59174=CARTESIAN_POINT('Ctrl Pts',(5.5360153038977,1.07224024467438,-5.41516098360831));
#59175=CARTESIAN_POINT('Ctrl Pts',(5.80691784466929,0.959867948076925,-5.43620465823388));
#59176=CARTESIAN_POINT('Ctrl Pts',(5.930360003029,0.875274915581406,-5.45105349297774));
#59177=CARTESIAN_POINT('Ctrl Pts',(6.12526953479794,0.680365383812468,-5.47879477947926));
#59178=CARTESIAN_POINT('Ctrl Pts',(6.20986678192829,0.556920939780123,-5.4935138828468));
#59179=CARTESIAN_POINT('Ctrl Pts',(6.32224213731147,0.286010457396547,-5.51425912806026));
#59180=CARTESIAN_POINT('Ctrl Pts',(6.35,0.138514252542117,-5.52));
#59181=CARTESIAN_POINT('Ctrl Pts',(6.35,-0.138514252542118,-5.52));
#59182=CARTESIAN_POINT('Ctrl Pts',(6.32224213731147,-0.286010457396548,
-5.51425912806026));
#59183=CARTESIAN_POINT('Ctrl Pts',(6.20986678192829,-0.556920939780125,
-5.4935138828468));
#59184=CARTESIAN_POINT('Ctrl Pts',(6.12526953479794,-0.68036538381247,-5.47879477947926));
#59185=CARTESIAN_POINT('Ctrl Pts',(5.930360003029,-0.875274915581407,-5.45105349297774));
#59186=CARTESIAN_POINT('Ctrl Pts',(5.80691784466929,-0.959867948076927,
-5.43620465823388));
#59187=CARTESIAN_POINT('Ctrl Pts',(5.5360153038977,-1.07224024467438,-5.41516098360831));
#59188=CARTESIAN_POINT('Ctrl Pts',(5.38852190055984,-1.1,-5.40928830808638));
#59189=CARTESIAN_POINT('Ctrl Pts',(5.25,-1.1,-5.40928830808638));
#59190=CARTESIAN_POINT('Origin',(5.25,-8.45,5.17413272639757E-16));
#59191=CARTESIAN_POINT('',(6.35,-8.45,5.17413272639757E-16));
#59192=CARTESIAN_POINT('',(4.15,-8.45,3.82702124733548E-16));
#59193=CARTESIAN_POINT('Ctrl Pts',(6.35,-8.45,6.59194920871187E-16));
#59194=CARTESIAN_POINT('Ctrl Pts',(6.35,-8.45,-0.138286410729709));
#59195=CARTESIAN_POINT('Ctrl Pts',(6.32233132681,-8.44625875235353,-0.285683724538778));
#59196=CARTESIAN_POINT('Ctrl Pts',(6.21002324830763,-8.4327360375918,-0.556655210212818));
#59197=CARTESIAN_POINT('Ctrl Pts',(6.12539248344495,-8.42314504656407,-0.680242435165458));
#59198=CARTESIAN_POINT('Ctrl Pts',(5.93024147512979,-8.40510492225533,-0.875393443480617));
#59199=CARTESIAN_POINT('Ctrl Pts',(5.80665466688422,-8.39547821560232,-0.960023455891921));
#59200=CARTESIAN_POINT('Ctrl Pts',(5.53568459489851,-8.381873644329,-1.07233098368286));
#59201=CARTESIAN_POINT('Ctrl Pts',(5.38828777132263,-8.37809644251008,-1.1));
#59202=CARTESIAN_POINT('Ctrl Pts',(5.11171222867737,-8.37809644251008,-1.1));
#59203=CARTESIAN_POINT('Ctrl Pts',(4.96431540510149,-8.381873644329,-1.07233098368286));
#59204=CARTESIAN_POINT('Ctrl Pts',(4.69334533311577,-8.39547821560232,-0.96002345589192));
#59205=CARTESIAN_POINT('Ctrl Pts',(4.56975852487021,-8.40510492225533,-0.875393443480617));
#59206=CARTESIAN_POINT('Ctrl Pts',(4.37460751655505,-8.42314504656407,-0.680242435165458));
#59207=CARTESIAN_POINT('Ctrl Pts',(4.28997675169238,-8.4327360375918,-0.556655210212819));
#59208=CARTESIAN_POINT('Ctrl Pts',(4.17766867319,-8.44625875235353,-0.285683724538779));
#59209=CARTESIAN_POINT('Ctrl Pts',(4.15,-8.45,-0.138286410729709));
#59210=CARTESIAN_POINT('Ctrl Pts',(4.15,-8.45,3.46944695195361E-16));
#59211=CARTESIAN_POINT('Ctrl Pts',(4.15,-8.45,4.85722573273506E-16));
#59212=CARTESIAN_POINT('Ctrl Pts',(4.15,-8.45,0.13828641072971));
#59213=CARTESIAN_POINT('Ctrl Pts',(4.17766867319,-8.44625875235353,0.285683724538779));
#59214=CARTESIAN_POINT('Ctrl Pts',(4.28997675169238,-8.4327360375918,0.55665521021282));
#59215=CARTESIAN_POINT('Ctrl Pts',(4.37460751655505,-8.42314504656407,0.680242435165459));
#59216=CARTESIAN_POINT('Ctrl Pts',(4.56975852487021,-8.40510492225533,0.875393443480617));
#59217=CARTESIAN_POINT('Ctrl Pts',(4.69334533311577,-8.39547821560232,0.960023455891921));
#59218=CARTESIAN_POINT('Ctrl Pts',(4.96431540510149,-8.381873644329,1.07233098368286));
#59219=CARTESIAN_POINT('Ctrl Pts',(5.11171222867737,-8.37809644251008,1.1));
#59220=CARTESIAN_POINT('Ctrl Pts',(5.25,-8.37809644251008,1.1));
#59221=CARTESIAN_POINT('Ctrl Pts',(5.38828777132263,-8.37809644251008,1.1));
#59222=CARTESIAN_POINT('Ctrl Pts',(5.53568459489851,-8.381873644329,1.07233098368286));
#59223=CARTESIAN_POINT('Ctrl Pts',(5.80665466688422,-8.39547821560232,0.960023455891922));
#59224=CARTESIAN_POINT('Ctrl Pts',(5.93024147512979,-8.40510492225533,0.875393443480618));
#59225=CARTESIAN_POINT('Ctrl Pts',(6.12539248344495,-8.42314504656407,0.680242435165459));
#59226=CARTESIAN_POINT('Ctrl Pts',(6.21002324830763,-8.4327360375918,0.55665521021282));
#59227=CARTESIAN_POINT('Ctrl Pts',(6.32233132681,-8.44625875235353,0.28568372453878));
#59228=CARTESIAN_POINT('Ctrl Pts',(6.35,-8.45,0.13828641072971));
#59229=CARTESIAN_POINT('Ctrl Pts',(6.35,-8.45,5.20417042793042E-16));
#59230=CARTESIAN_POINT('',(4.15,-5.52,4.9656535363196E-16));
#59231=CARTESIAN_POINT('',(4.15,-8.45,6.52124420545966E-16));
#59232=CARTESIAN_POINT('',(5.25,-5.40928830808638,1.1));
#59233=CARTESIAN_POINT('Ctrl Pts',(5.25,-5.40928830808638,1.1));
#59234=CARTESIAN_POINT('Ctrl Pts',(5.11147809944016,-5.40928830808638,1.1));
#59235=CARTESIAN_POINT('Ctrl Pts',(4.9639846961023,-5.41516098360831,1.07224024467438));
#59236=CARTESIAN_POINT('Ctrl Pts',(4.69308215533071,-5.43620465823388,0.959867948076926));
#59237=CARTESIAN_POINT('Ctrl Pts',(4.569639996971,-5.45105349297774,0.875274915581407));
#59238=CARTESIAN_POINT('Ctrl Pts',(4.37473046520206,-5.47879477947926,0.680365383812469));
#59239=CARTESIAN_POINT('Ctrl Pts',(4.29013321807171,-5.4935138828468,0.556920939780125));
#59240=CARTESIAN_POINT('Ctrl Pts',(4.17775786268853,-5.51425912806026,0.286010457396548));
#59241=CARTESIAN_POINT('Ctrl Pts',(4.15,-5.52,0.138514252542118));
#59242=CARTESIAN_POINT('Ctrl Pts',(4.15,-5.52,4.85722573273506E-16));
#59243=CARTESIAN_POINT('',(6.35,-5.52,-3.03308047045133E-16));
#59244=CARTESIAN_POINT('Ctrl Pts',(6.35,-5.52,1.04083408558608E-16));
#59245=CARTESIAN_POINT('Ctrl Pts',(6.35,-5.52,0.138514252542118));
#59246=CARTESIAN_POINT('Ctrl Pts',(6.32224213731147,-5.51425912806026,0.286010457396547));
#59247=CARTESIAN_POINT('Ctrl Pts',(6.20986678192829,-5.4935138828468,0.556920939780124));
#59248=CARTESIAN_POINT('Ctrl Pts',(6.12526953479794,-5.47879477947926,0.680365383812469));
#59249=CARTESIAN_POINT('Ctrl Pts',(5.930360003029,-5.45105349297774,0.875274915581406));
#59250=CARTESIAN_POINT('Ctrl Pts',(5.80691784466929,-5.43620465823388,0.959867948076926));
#59251=CARTESIAN_POINT('Ctrl Pts',(5.5360153038977,-5.41516098360831,1.07224024467438));
#59252=CARTESIAN_POINT('Ctrl Pts',(5.38852190055984,-5.40928830808638,1.1));
#59253=CARTESIAN_POINT('Ctrl Pts',(5.25,-5.40928830808638,1.1));
#59254=CARTESIAN_POINT('Ctrl Pts',(4.15,-5.52,4.85722573273506E-16));
#59255=CARTESIAN_POINT('Ctrl Pts',(4.15,-5.52,-0.138514252542117));
#59256=CARTESIAN_POINT('Ctrl Pts',(4.17775786268853,-5.51425912806026,-0.286010457396547));
#59257=CARTESIAN_POINT('Ctrl Pts',(4.29013321807171,-5.4935138828468,-0.556920939780124));
#59258=CARTESIAN_POINT('Ctrl Pts',(4.37473046520206,-5.47879477947926,-0.680365383812469));
#59259=CARTESIAN_POINT('Ctrl Pts',(4.569639996971,-5.45105349297774,-0.875274915581406));
#59260=CARTESIAN_POINT('Ctrl Pts',(4.69308215533072,-5.43620465823388,-0.959867948076926));
#59261=CARTESIAN_POINT('Ctrl Pts',(4.9639846961023,-5.41516098360831,-1.07224024467438));
#59262=CARTESIAN_POINT('Ctrl Pts',(5.11147809944016,-5.40928830808638,-1.1));
#59263=CARTESIAN_POINT('Ctrl Pts',(5.38852190055984,-5.40928830808638,-1.1));
#59264=CARTESIAN_POINT('Ctrl Pts',(5.5360153038977,-5.41516098360831,-1.07224024467438));
#59265=CARTESIAN_POINT('Ctrl Pts',(5.80691784466929,-5.43620465823388,-0.959867948076926));
#59266=CARTESIAN_POINT('Ctrl Pts',(5.930360003029,-5.45105349297774,-0.875274915581406));
#59267=CARTESIAN_POINT('Ctrl Pts',(6.12526953479794,-5.47879477947926,-0.680365383812469));
#59268=CARTESIAN_POINT('Ctrl Pts',(6.20986678192829,-5.4935138828468,-0.556920939780124));
#59269=CARTESIAN_POINT('Ctrl Pts',(6.32224213731147,-5.51425912806026,-0.286010457396547));
#59270=CARTESIAN_POINT('Ctrl Pts',(6.35,-5.52,-0.138514252542118));
#59271=CARTESIAN_POINT('Ctrl Pts',(6.35,-5.52,1.38777878078145E-16));
#59272=CARTESIAN_POINT('Origin',(5.25,0.,8.45));
#59273=CARTESIAN_POINT('',(6.35,0.,8.45));
#59274=CARTESIAN_POINT('',(4.15,-1.34711147906209E-16,8.45));
#59275=CARTESIAN_POINT('Ctrl Pts',(6.35,-6.93889390390723E-17,8.45));
#59276=CARTESIAN_POINT('Ctrl Pts',(6.35,-0.13828641072971,8.45));
#59277=CARTESIAN_POINT('Ctrl Pts',(6.32233132681,-0.285683724538779,8.44625875235353));
#59278=CARTESIAN_POINT('Ctrl Pts',(6.21002324830763,-0.556655210212819,
8.4327360375918));
#59279=CARTESIAN_POINT('Ctrl Pts',(6.12539248344495,-0.680242435165459,
8.42314504656407));
#59280=CARTESIAN_POINT('Ctrl Pts',(5.93024147512979,-0.875393443480617,
8.40510492225533));
#59281=CARTESIAN_POINT('Ctrl Pts',(5.80665466688422,-0.960023455891921,
8.39547821560232));
#59282=CARTESIAN_POINT('Ctrl Pts',(5.53568459489851,-1.07233098368286,8.381873644329));
#59283=CARTESIAN_POINT('Ctrl Pts',(5.38828777132263,-1.1,8.37809644251008));
#59284=CARTESIAN_POINT('Ctrl Pts',(5.11171222867737,-1.1,8.37809644251008));
#59285=CARTESIAN_POINT('Ctrl Pts',(4.96431540510149,-1.07233098368286,8.381873644329));
#59286=CARTESIAN_POINT('Ctrl Pts',(4.69334533311577,-0.960023455891921,
8.39547821560232));
#59287=CARTESIAN_POINT('Ctrl Pts',(4.56975852487021,-0.875393443480617,
8.40510492225533));
#59288=CARTESIAN_POINT('Ctrl Pts',(4.37460751655505,-0.680242435165459,
8.42314504656407));
#59289=CARTESIAN_POINT('Ctrl Pts',(4.28997675169238,-0.556655210212819,
8.4327360375918));
#59290=CARTESIAN_POINT('Ctrl Pts',(4.17766867319,-0.285683724538779,8.44625875235353));
#59291=CARTESIAN_POINT('Ctrl Pts',(4.15,-0.13828641072971,8.45));
#59292=CARTESIAN_POINT('Ctrl Pts',(4.15,-6.93889390390723E-17,8.45));
#59293=CARTESIAN_POINT('Ctrl Pts',(4.15,-2.08166817117217E-16,8.45));
#59294=CARTESIAN_POINT('Ctrl Pts',(4.15,0.138286410729709,8.45));
#59295=CARTESIAN_POINT('Ctrl Pts',(4.17766867319,0.285683724538779,8.44625875235353));
#59296=CARTESIAN_POINT('Ctrl Pts',(4.28997675169238,0.556655210212819,8.4327360375918));
#59297=CARTESIAN_POINT('Ctrl Pts',(4.37460751655505,0.680242435165458,8.42314504656407));
#59298=CARTESIAN_POINT('Ctrl Pts',(4.56975852487021,0.875393443480617,8.40510492225533));
#59299=CARTESIAN_POINT('Ctrl Pts',(4.69334533311577,0.960023455891921,8.39547821560232));
#59300=CARTESIAN_POINT('Ctrl Pts',(4.96431540510149,1.07233098368286,8.381873644329));
#59301=CARTESIAN_POINT('Ctrl Pts',(5.11171222867737,1.1,8.37809644251008));
#59302=CARTESIAN_POINT('Ctrl Pts',(5.25,1.1,8.37809644251008));
#59303=CARTESIAN_POINT('Ctrl Pts',(5.38828777132263,1.1,8.37809644251008));
#59304=CARTESIAN_POINT('Ctrl Pts',(5.53568459489851,1.07233098368286,8.381873644329));
#59305=CARTESIAN_POINT('Ctrl Pts',(5.80665466688422,0.960023455891921,8.39547821560232));
#59306=CARTESIAN_POINT('Ctrl Pts',(5.93024147512979,0.875393443480617,8.40510492225533));
#59307=CARTESIAN_POINT('Ctrl Pts',(6.12539248344495,0.680242435165459,8.42314504656407));
#59308=CARTESIAN_POINT('Ctrl Pts',(6.21002324830763,0.556655210212819,8.4327360375918));
#59309=CARTESIAN_POINT('Ctrl Pts',(6.32233132681,0.285683724538779,8.44625875235353));
#59310=CARTESIAN_POINT('Ctrl Pts',(6.35,0.138286410729709,8.45));
#59311=CARTESIAN_POINT('Ctrl Pts',(6.35,0.,8.45));
#59312=CARTESIAN_POINT('',(4.15,1.54091747751945E-16,5.52));
#59313=CARTESIAN_POINT('',(4.15,1.34711147906209E-16,8.45));
#59314=CARTESIAN_POINT('',(5.25,1.1,5.40928830808638));
#59315=CARTESIAN_POINT('Ctrl Pts',(5.25,1.1,5.40928830808638));
#59316=CARTESIAN_POINT('Ctrl Pts',(5.11147809944016,1.1,5.40928830808638));
#59317=CARTESIAN_POINT('Ctrl Pts',(4.9639846961023,1.07224024467438,5.41516098360831));
#59318=CARTESIAN_POINT('Ctrl Pts',(4.69308215533071,0.959867948076926,5.43620465823388));
#59319=CARTESIAN_POINT('Ctrl Pts',(4.569639996971,0.875274915581406,5.45105349297774));
#59320=CARTESIAN_POINT('Ctrl Pts',(4.37473046520206,0.680365383812469,5.47879477947926));
#59321=CARTESIAN_POINT('Ctrl Pts',(4.29013321807171,0.556920939780124,5.4935138828468));
#59322=CARTESIAN_POINT('Ctrl Pts',(4.17775786268853,0.286010457396548,5.51425912806026));
#59323=CARTESIAN_POINT('Ctrl Pts',(4.15,0.138514252542118,5.52));
#59324=CARTESIAN_POINT('Ctrl Pts',(4.15,1.73472347597681E-16,5.52));
#59325=CARTESIAN_POINT('Ctrl Pts',(4.15,1.73472347597681E-16,5.52));
#59326=CARTESIAN_POINT('Ctrl Pts',(4.15,-0.138514252542118,5.52));
#59327=CARTESIAN_POINT('Ctrl Pts',(4.17775786268853,-0.286010457396548,
5.51425912806026));
#59328=CARTESIAN_POINT('Ctrl Pts',(4.29013321807171,-0.556920939780124,
5.4935138828468));
#59329=CARTESIAN_POINT('Ctrl Pts',(4.37473046520206,-0.680365383812469,
5.47879477947926));
#59330=CARTESIAN_POINT('Ctrl Pts',(4.569639996971,-0.875274915581406,5.45105349297774));
#59331=CARTESIAN_POINT('Ctrl Pts',(4.69308215533072,-0.959867948076927,
5.43620465823388));
#59332=CARTESIAN_POINT('Ctrl Pts',(4.9639846961023,-1.07224024467438,5.41516098360831));
#59333=CARTESIAN_POINT('Ctrl Pts',(5.11147809944016,-1.1,5.40928830808638));
#59334=CARTESIAN_POINT('Ctrl Pts',(5.38852190055984,-1.1,5.40928830808638));
#59335=CARTESIAN_POINT('Ctrl Pts',(5.53601530389771,-1.07224024467438,5.41516098360831));
#59336=CARTESIAN_POINT('Ctrl Pts',(5.80691784466929,-0.959867948076926,
5.43620465823388));
#59337=CARTESIAN_POINT('Ctrl Pts',(5.930360003029,-0.875274915581406,5.45105349297774));
#59338=CARTESIAN_POINT('Ctrl Pts',(6.12526953479794,-0.680365383812469,
5.47879477947926));
#59339=CARTESIAN_POINT('Ctrl Pts',(6.20986678192829,-0.556920939780124,
5.4935138828468));
#59340=CARTESIAN_POINT('Ctrl Pts',(6.32224213731147,-0.286010457396547,
5.51425912806026));
#59341=CARTESIAN_POINT('Ctrl Pts',(6.35,-0.138514252542118,5.52));
#59342=CARTESIAN_POINT('Ctrl Pts',(6.35,0.138514252542118,5.52));
#59343=CARTESIAN_POINT('Ctrl Pts',(6.32224213731147,0.286010457396547,5.51425912806026));
#59344=CARTESIAN_POINT('Ctrl Pts',(6.20986678192829,0.556920939780124,5.4935138828468));
#59345=CARTESIAN_POINT('Ctrl Pts',(6.12526953479794,0.680365383812469,5.47879477947926));
#59346=CARTESIAN_POINT('Ctrl Pts',(5.930360003029,0.875274915581406,5.45105349297774));
#59347=CARTESIAN_POINT('Ctrl Pts',(5.80691784466929,0.959867948076926,5.43620465823388));
#59348=CARTESIAN_POINT('Ctrl Pts',(5.5360153038977,1.07224024467438,5.41516098360831));
#59349=CARTESIAN_POINT('Ctrl Pts',(5.38852190055984,1.1,5.40928830808638));
#59350=CARTESIAN_POINT('Ctrl Pts',(5.25,1.1,5.40928830808638));
#59351=CARTESIAN_POINT('Origin',(5.25,0.,0.));
#59352=CARTESIAN_POINT('',(3.75,-8.45,-1.03482654527951E-15));
#59353=CARTESIAN_POINT('Origin',(3.75,0.,0.));
#59354=CARTESIAN_POINT('',(5.25,-8.45,-1.03482654527951E-15));
#59355=CARTESIAN_POINT('',(6.75,-8.45,-1.03482654527951E-15));
#59356=CARTESIAN_POINT('',(5.25,-8.45,-1.03482654527951E-15));
#59357=CARTESIAN_POINT('Origin',(6.75,0.,0.));
#59358=CARTESIAN_POINT('Origin',(3.75,9.,0.));
#59359=CARTESIAN_POINT('',(3.75,-8.8,1.07768918324967E-15));
#59360=CARTESIAN_POINT('Origin',(3.75,0.,0.));
#59361=CARTESIAN_POINT('Origin',(6.75,8.45,0.));
#59362=CARTESIAN_POINT('',(6.75,-8.8,-1.07768918324967E-15));
#59363=CARTESIAN_POINT('Origin',(6.75,0.,0.));
#59364=CARTESIAN_POINT('Origin',(5.25,0.,0.));
#59365=CARTESIAN_POINT('',(10.1,-8.8,-1.07768918324967E-15));
#59366=CARTESIAN_POINT('Origin',(10.1,0.,0.));
#59367=CARTESIAN_POINT('',(5.25,-8.8,-1.07768918324967E-15));
#59368=CARTESIAN_POINT('Origin',(0.2,0.,0.));
#59369=CARTESIAN_POINT('',(0.4,-8.8,-1.07768918324967E-15));
#59370=CARTESIAN_POINT('Origin',(0.4,0.,0.));
#59371=CARTESIAN_POINT('',(-1.04083408558608E-16,-8.4,-1.02870331128378E-15));
#59372=CARTESIAN_POINT('',(0.2,-8.6,-1.05319624726672E-15));
#59373=CARTESIAN_POINT('Origin',(0.,0.,0.));
#59374=CARTESIAN_POINT('Origin',(5.25,0.,0.));
#59375=CARTESIAN_POINT('',(5.25,-8.8,-1.07768918324967E-15));
#59376=CARTESIAN_POINT('Origin',(10.3,0.,0.));
#59377=CARTESIAN_POINT('',(10.5,-8.4,-1.02870331128378E-15));
#59378=CARTESIAN_POINT('Origin',(10.5,0.,0.));
#59379=CARTESIAN_POINT('',(10.3,-8.6,-1.05319624726672E-15));
#59380=CARTESIAN_POINT('Origin',(10.5,5.82,0.));
#59381=CARTESIAN_POINT('',(10.5,-5.82,-7.1274443710376E-16));
#59382=CARTESIAN_POINT('Origin',(10.5,0.,0.));
#59383=CARTESIAN_POINT('Origin',(10.35,0.,0.));
#59384=CARTESIAN_POINT('',(10.2,-5.52,-6.76005033129339E-16));
#59385=CARTESIAN_POINT('',(10.35,-5.67,-6.94374735116549E-16));
#59386=CARTESIAN_POINT('Origin',(10.2,0.,0.));
#59387=CARTESIAN_POINT('Origin',(5.25,0.,0.));
#59388=CARTESIAN_POINT('',(5.25,-5.52,-6.76005033129339E-16));
#59389=CARTESIAN_POINT('',(0.3,-5.52,-6.76005033129339E-16));
#59390=CARTESIAN_POINT('',(5.25,-5.52,-6.76005033129339E-16));
#59391=CARTESIAN_POINT('Origin',(0.3,0.,0.));
#59392=CARTESIAN_POINT('Origin',(0.15,0.,0.));
#59393=CARTESIAN_POINT('',(-3.98986399474666E-16,-5.82,-7.1274443710376E-16));
#59394=CARTESIAN_POINT('',(0.15,-5.67,-6.94374735116549E-16));
#59395=CARTESIAN_POINT('Origin',(0.,0.,0.));
#59396=CARTESIAN_POINT('Origin',(0.,8.4,0.));
#59397=CARTESIAN_POINT('',(0.,0.,0.));
#59398=CARTESIAN_POINT('Origin',(0.1,-2.88925991435643,6.97529047046021));
#59399=CARTESIAN_POINT('',(0.,-2.88925991435643,7.72529047046022));
#59400=CARTESIAN_POINT('Origin',(0.,-2.88925991435643,6.97529047046021));
#59401=CARTESIAN_POINT('',(0.2,-2.88925991435643,7.52529047046021));
#59402=CARTESIAN_POINT('',(0.1,-2.88925991435643,7.62529047046022));
#59403=CARTESIAN_POINT('Origin',(0.2,-2.88925991435643,6.97529047046021));
#59404=CARTESIAN_POINT('Origin',(0.,-2.88925991435643,6.97529047046021));
#59405=CARTESIAN_POINT('',(0.8,-2.88925991435643,7.52529047046021));
#59406=CARTESIAN_POINT('',(0.,-2.88925991435643,7.52529047046021));
#59407=CARTESIAN_POINT('Origin',(0.8,-2.88925991435643,6.97529047046021));
#59408=CARTESIAN_POINT('Origin',(0.,0.,-0.183038486691444));
#59409=CARTESIAN_POINT('',(0.,-1.84677028397389,6.44045336278674));
#59410=CARTESIAN_POINT('',(0.,-2.60477301247064,9.08392302661711));
#59411=CARTESIAN_POINT('',(0.,-1.84677028397389,6.44045336278674));
#59412=CARTESIAN_POINT('',(0.,-3.24822445565046,5.85995203783395));
#59413=CARTESIAN_POINT('',(0.,-3.24822445565046,5.85995203783395));
#59414=CARTESIAN_POINT('',(0.,-3.8784769619707,6.99695765711517));
#59415=CARTESIAN_POINT('',(0.,-3.8784769619707,6.99695765711517));
#59416=CARTESIAN_POINT('',(0.,-4.37985668768992,6.69453922202999));
#59417=CARTESIAN_POINT('',(0.,-4.37985668768992,6.69453922202999));
#59418=CARTESIAN_POINT('',(0.,-4.85777416858265,6.3562591299483));
#59419=CARTESIAN_POINT('',(0.,-4.85777416858265,6.3562591299483));
#59420=CARTESIAN_POINT('',(0.,-5.30966927135158,5.98392949731736));
#59421=CARTESIAN_POINT('',(0.,-5.30966927135158,5.98392949731736));
#59422=CARTESIAN_POINT('',(0.,-5.73312126073229,5.57954483893977));
#59423=CARTESIAN_POINT('',(0.,-5.73312126073229,5.57954483893977));
#59424=CARTESIAN_POINT('',(0.,-6.12586176701418,5.14527138365256));
#59425=CARTESIAN_POINT('',(0.,-6.12586176701418,5.14527138365256));
#59426=CARTESIAN_POINT('',(0.,-6.4857869373617,4.68343547015952));
#59427=CARTESIAN_POINT('',(0.,-6.4857869373617,4.68343547015952));
#59428=CARTESIAN_POINT('',(0.,-6.81096870584301,4.19651108517864));
#59429=CARTESIAN_POINT('',(0.,-6.81096870584301,4.19651108517864));
#59430=CARTESIAN_POINT('',(0.,-7.09966512179413,3.68710661066098));
#59431=CARTESIAN_POINT('',(0.,-7.09966512179413,3.68710661066098));
#59432=CARTESIAN_POINT('',(0.,-7.35032968119119,3.15795085107414));
#59433=CARTESIAN_POINT('',(0.,-7.35032968119119,3.15795085107414));
#59434=CARTESIAN_POINT('',(0.,-7.5616196110438,2.61187841560012));
#59435=CARTESIAN_POINT('',(0.,-7.5616196110438,2.61187841560012));
#59436=CARTESIAN_POINT('',(0.,-7.73240306243155,2.05181453355296));
#59437=CARTESIAN_POINT('',(0.,-7.73240306243155,2.05181453355296));
#59438=CARTESIAN_POINT('',(0.,-7.86176517365131,1.48075938435772));
#59439=CARTESIAN_POINT('',(0.,-7.86176517365131,1.48075938435772));
#59440=CARTESIAN_POINT('',(0.,-7.94901297099613,0.901772026032757));
#59441=CARTESIAN_POINT('',(0.,-7.94901297099613,0.901772026032757));
#59442=CARTESIAN_POINT('',(0.,-7.99367908091301,0.317954008268197));
#59443=CARTESIAN_POINT('',(0.,-7.99367908091301,0.317954008268197));
#59444=CARTESIAN_POINT('',(0.,-7.99552423365383,-0.267567242117311));
#59445=CARTESIAN_POINT('',(0.,-7.99552423365383,-0.267567242117311));
#59446=CARTESIAN_POINT('',(0.,-7.95453854500815,-0.85165517433975));
#59447=CARTESIAN_POINT('',(0.,-7.95453854500815,-0.85165517433975));
#59448=CARTESIAN_POINT('',(0.,-7.87094156925134,-1.43118091568862));
#59449=CARTESIAN_POINT('',(0.,-7.87094156925134,-1.43118091568862));
#59450=CARTESIAN_POINT('',(0.,-7.74518112302486,-2.00304003243553));
#59451=CARTESIAN_POINT('',(0.,-7.74518112302486,-2.00304003243553));
#59452=CARTESIAN_POINT('',(0.,-7.5779308864487,-2.56416915982678));
#59453=CARTESIAN_POINT('',(0.,-7.5779308864487,-2.56416915982678));
#59454=CARTESIAN_POINT('',(0.,-7.37008679431654,-3.11156241207547));
#59455=CARTESIAN_POINT('',(0.,-7.37008679431654,-3.11156241207547));
#59456=CARTESIAN_POINT('',(0.,-7.12276223670551,-3.64228748444736));
#59457=CARTESIAN_POINT('',(0.,-7.12276223670551,-3.64228748444736));
#59458=CARTESIAN_POINT('',(0.,-6.83728209471014,-4.15350136118385));
#59459=CARTESIAN_POINT('',(0.,-6.83728209471014,-4.15350136118385));
#59460=CARTESIAN_POINT('',(0.,-6.51517564325019,-4.64246554511711));
#59461=CARTESIAN_POINT('',(0.,-6.51517564325019,-4.64246554511711));
#59462=CARTESIAN_POINT('',(0.,-6.15816835897094,-5.10656072739463));
#59463=CARTESIAN_POINT('',(0.,-6.15816835897094,-5.10656072739463));
#59464=CARTESIAN_POINT('',(0.,-5.76817267711992,-5.54330081872951));
#59465=CARTESIAN_POINT('',(0.,-5.76817267711992,-5.54330081872951));
#59466=CARTESIAN_POINT('',(0.,-5.34727774691394,-5.95034626701329));
#59467=CARTESIAN_POINT('',(0.,-5.34727774691394,-5.95034626701329));
#59468=CARTESIAN_POINT('',(0.,-4.89773824027559,-6.32551658995075));
#59469=CARTESIAN_POINT('',(0.,-4.89773824027559,-6.32551658995075));
#59470=CARTESIAN_POINT('',(0.,-4.42196227388907,-6.66680205558121));
#59471=CARTESIAN_POINT('',(0.,-4.42196227388907,-6.66680205558121));
#59472=CARTESIAN_POINT('',(0.,-3.922498509275,-6.9723744481156));
#59473=CARTESIAN_POINT('',(0.,-3.922498509275,-6.9723744481156));
#59474=CARTESIAN_POINT('',(0.,-3.40202249998754,-7.24059686141816));
#59475=CARTESIAN_POINT('',(0.,-3.40202249998754,-7.24059686141816));
#59476=CARTESIAN_POINT('',(0.,-2.86332235906941,-7.47003246767062));
#59477=CARTESIAN_POINT('',(0.,-2.86332235906941,-7.47003246767062));
#59478=CARTESIAN_POINT('',(0.,-2.30928382354251,-7.65945221424645));
#59479=CARTESIAN_POINT('',(0.,-2.30928382354251,-7.65945221424645));
#59480=CARTESIAN_POINT('',(0.,-1.74287479594128,-7.80784140756411));
#59481=CARTESIAN_POINT('',(0.,-1.74287479594128,-7.80784140756411));
#59482=CARTESIAN_POINT('',(0.,-1.16712944569752,-7.91440514865052));
#59483=CARTESIAN_POINT('',(0.,-1.16712944569752,-7.91440514865052));
#59484=CARTESIAN_POINT('',(0.,-0.585131955543311,-7.9785725912974));
#59485=CARTESIAN_POINT('',(0.,-0.585131955543311,-7.9785725912974));
#59486=CARTESIAN_POINT('',(0.,-1.46957615897682E-15,-8.));
#59487=CARTESIAN_POINT('',(0.,-1.46957615897682E-15,-8.));
#59488=CARTESIAN_POINT('',(0.,0.585131955543308,-7.9785725912974));
#59489=CARTESIAN_POINT('',(0.,0.585131955543308,-7.9785725912974));
#59490=CARTESIAN_POINT('',(0.,1.16712944569752,-7.91440514865052));
#59491=CARTESIAN_POINT('',(0.,1.16712944569752,-7.91440514865052));
#59492=CARTESIAN_POINT('',(0.,1.74287479594128,-7.80784140756411));
#59493=CARTESIAN_POINT('',(0.,1.74287479594128,-7.80784140756411));
#59494=CARTESIAN_POINT('',(0.,2.30928382354251,-7.65945221424645));
#59495=CARTESIAN_POINT('',(0.,2.30928382354251,-7.65945221424645));
#59496=CARTESIAN_POINT('',(0.,2.86332235906941,-7.47003246767062));
#59497=CARTESIAN_POINT('',(0.,2.86332235906941,-7.47003246767062));
#59498=CARTESIAN_POINT('',(0.,3.40202249998754,-7.24059686141816));
#59499=CARTESIAN_POINT('',(0.,3.40202249998754,-7.24059686141816));
#59500=CARTESIAN_POINT('',(0.,3.922498509275,-6.97237444811561));
#59501=CARTESIAN_POINT('',(0.,3.922498509275,-6.97237444811561));
#59502=CARTESIAN_POINT('',(0.,4.42196227388906,-6.66680205558121));
#59503=CARTESIAN_POINT('',(0.,4.42196227388906,-6.66680205558121));
#59504=CARTESIAN_POINT('',(0.,4.89773824027559,-6.32551658995075));
#59505=CARTESIAN_POINT('',(0.,4.89773824027559,-6.32551658995075));
#59506=CARTESIAN_POINT('',(0.,5.34727774691393,-5.95034626701329));
#59507=CARTESIAN_POINT('',(0.,5.34727774691393,-5.95034626701329));
#59508=CARTESIAN_POINT('',(0.,5.76817267711992,-5.54330081872951));
#59509=CARTESIAN_POINT('',(0.,5.76817267711992,-5.54330081872951));
#59510=CARTESIAN_POINT('',(0.,6.15816835897094,-5.10656072739463));
#59511=CARTESIAN_POINT('',(0.,6.15816835897094,-5.10656072739463));
#59512=CARTESIAN_POINT('',(0.,6.51517564325019,-4.64246554511711));
#59513=CARTESIAN_POINT('',(0.,6.51517564325019,-4.64246554511711));
#59514=CARTESIAN_POINT('',(0.,6.83728209471014,-4.15350136118385));
#59515=CARTESIAN_POINT('',(0.,6.83728209471014,-4.15350136118385));
#59516=CARTESIAN_POINT('',(0.,7.12276223670551,-3.64228748444737));
#59517=CARTESIAN_POINT('',(0.,7.12276223670551,-3.64228748444737));
#59518=CARTESIAN_POINT('',(0.,7.37008679431654,-3.11156241207547));
#59519=CARTESIAN_POINT('',(0.,7.37008679431654,-3.11156241207547));
#59520=CARTESIAN_POINT('',(0.,7.5779308864487,-2.56416915982678));
#59521=CARTESIAN_POINT('',(0.,7.5779308864487,-2.56416915982678));
#59522=CARTESIAN_POINT('',(0.,7.74518112302486,-2.00304003243554));
#59523=CARTESIAN_POINT('',(0.,7.74518112302486,-2.00304003243554));
#59524=CARTESIAN_POINT('',(0.,7.87094156925134,-1.43118091568862));
#59525=CARTESIAN_POINT('',(0.,7.87094156925134,-1.43118091568862));
#59526=CARTESIAN_POINT('',(0.,7.95453854500815,-0.851655174339752));
#59527=CARTESIAN_POINT('',(0.,7.95453854500815,-0.851655174339752));
#59528=CARTESIAN_POINT('',(0.,7.99552423365383,-0.267567242117314));
#59529=CARTESIAN_POINT('',(0.,7.99552423365383,-0.267567242117314));
#59530=CARTESIAN_POINT('',(0.,7.99367908091301,0.317954008268194));
#59531=CARTESIAN_POINT('',(0.,7.99367908091301,0.317954008268194));
#59532=CARTESIAN_POINT('',(0.,7.94901297099613,0.901772026032747));
#59533=CARTESIAN_POINT('',(0.,7.94901297099613,0.901772026032747));
#59534=CARTESIAN_POINT('',(0.,7.86176517365131,1.48075938435771));
#59535=CARTESIAN_POINT('',(0.,7.86176517365131,1.48075938435771));
#59536=CARTESIAN_POINT('',(0.,7.73240306243155,2.05181453355297));
#59537=CARTESIAN_POINT('',(0.,7.73240306243155,2.05181453355297));
#59538=CARTESIAN_POINT('',(0.,7.5616196110438,2.61187841560012));
#59539=CARTESIAN_POINT('',(0.,7.5616196110438,2.61187841560012));
#59540=CARTESIAN_POINT('',(0.,7.35032968119119,3.15795085107413));
#59541=CARTESIAN_POINT('',(0.,7.35032968119119,3.15795085107413));
#59542=CARTESIAN_POINT('',(0.,7.09966512179414,3.68710661066097));
#59543=CARTESIAN_POINT('',(0.,7.09966512179414,3.68710661066097));
#59544=CARTESIAN_POINT('',(0.,6.81096870584301,4.19651108517863));
#59545=CARTESIAN_POINT('',(0.,6.81096870584301,4.19651108517863));
#59546=CARTESIAN_POINT('',(0.,6.4857869373617,4.68343547015952));
#59547=CARTESIAN_POINT('',(0.,6.4857869373617,4.68343547015952));
#59548=CARTESIAN_POINT('',(0.,6.12586176701418,5.14527138365256));
#59549=CARTESIAN_POINT('',(0.,6.12586176701418,5.14527138365256));
#59550=CARTESIAN_POINT('',(0.,5.73312126073229,5.57954483893976));
#59551=CARTESIAN_POINT('',(0.,5.73312126073229,5.57954483893976));
#59552=CARTESIAN_POINT('',(0.,5.30966927135158,5.98392949731736));
#59553=CARTESIAN_POINT('',(0.,5.30966927135158,5.98392949731736));
#59554=CARTESIAN_POINT('',(0.,4.85777416858264,6.35625912994831));
#59555=CARTESIAN_POINT('',(0.,4.85777416858264,6.35625912994831));
#59556=CARTESIAN_POINT('',(0.,4.37985668768992,6.69453922202999));
#59557=CARTESIAN_POINT('',(0.,4.37985668768992,6.69453922202999));
#59558=CARTESIAN_POINT('',(0.,3.8784769619707,6.99695765711516));
#59559=CARTESIAN_POINT('',(0.,3.8784769619707,6.99695765711516));
#59560=CARTESIAN_POINT('',(0.,3.24822445565046,5.85995203783395));
#59561=CARTESIAN_POINT('',(0.,3.24822445565046,5.85995203783395));
#59562=CARTESIAN_POINT('',(0.,1.8467702839739,6.44045336278674));
#59563=CARTESIAN_POINT('',(0.,1.8467702839739,6.44045336278674));
#59564=CARTESIAN_POINT('',(0.,2.60477301247065,9.08392302661711));
#59565=CARTESIAN_POINT('',(0.,2.60477301247065,9.08392302661711));
#59566=CARTESIAN_POINT('',(0.,3.31804090301786,8.84833908515606));
#59567=CARTESIAN_POINT('',(0.,3.31804090301786,8.84833908515606));
#59568=CARTESIAN_POINT('',(0.,4.0103440110564,8.5568476037022));
#59569=CARTESIAN_POINT('',(0.,4.0103440110564,8.5568476037022));
#59570=CARTESIAN_POINT('',(0.,4.67730807342487,8.21129034843334));
#59571=CARTESIAN_POINT('',(0.,4.67730807342487,8.21129034843334));
#59572=CARTESIAN_POINT('',(0.,5.31471892974448,7.81385069589992));
#59573=CARTESIAN_POINT('',(0.,5.31471892974448,7.81385069589992));
#59574=CARTESIAN_POINT('',(0.,5.91854914926258,7.36703983753062));
#59575=CARTESIAN_POINT('',(0.,5.91854914926258,7.36703983753062));
#59576=CARTESIAN_POINT('',(0.,6.48498347785954,6.87368091286531));
#59577=CARTESIAN_POINT('',(0.,6.48498347785954,6.87368091286531));
#59578=CARTESIAN_POINT('',(0.,7.01044294443415,6.33689117176818));
#59579=CARTESIAN_POINT('',(0.,7.01044294443415,6.33689117176818));
#59580=CARTESIAN_POINT('',(0.,7.49160747435326,5.76006227832775));
#59581=CARTESIAN_POINT('',(0.,7.49160747435326,5.76006227832775));
#59582=CARTESIAN_POINT('',(0.,7.92543686708426,5.146838880892));
#59583=CARTESIAN_POINT('',(0.,7.92543686708426,5.146838880892));
#59584=CARTESIAN_POINT('',(0.,8.30919000546483,4.5010955836422));
#59585=CARTESIAN_POINT('',(0.,8.30919000546483,4.5010955836422));
#59586=CARTESIAN_POINT('',(0.,8.6404421752379,3.82691246520876));
#59587=CARTESIAN_POINT('',(0.,8.6404421752379,3.82691246520876));
#59588=CARTESIAN_POINT('',(0.,8.91710038541937,3.12854929901285));
#59589=CARTESIAN_POINT('',(0.,8.91710038541937,3.12854929901285));
#59590=CARTESIAN_POINT('',(0.,9.13741659269838,2.41041863822041));
#59591=CARTESIAN_POINT('',(0.,9.13741659269838,2.41041863822041));
#59592=CARTESIAN_POINT('',(0.,9.29999874631253,1.67705793536937));
#59593=CARTESIAN_POINT('',(0.,9.29999874631253,1.67705793536937));
#59594=CARTESIAN_POINT('',(0.,9.40381958361198,0.933100872829846));
#59595=CARTESIAN_POINT('',(0.,9.40381958361198,0.933100872829846));
#59596=CARTESIAN_POINT('',(0.,9.44822312073834,0.183248085243736));
#59597=CARTESIAN_POINT('',(0.,9.44822312073834,0.183248085243736));
#59598=CARTESIAN_POINT('',(0.,9.43292879740749,-0.567762541068464));
#59599=CARTESIAN_POINT('',(0.,9.43292879740749,-0.567762541068464));
#59600=CARTESIAN_POINT('',(0.,9.35803324960784,-1.31518580407262));
#59601=CARTESIAN_POINT('',(0.,9.35803324960784,-1.31518580407262));
#59602=CARTESIAN_POINT('',(0.,9.22400969901338,-2.05429916820971));
#59603=CARTESIAN_POINT('',(0.,9.22400969901338,-2.05429916820971));
#59604=CARTESIAN_POINT('',(0.,9.03170496296946,-2.7804326033682));
#59605=CARTESIAN_POINT('',(0.,9.03170496296946,-2.7804326033682));
#59606=CARTESIAN_POINT('',(0.,8.78233410394347,-3.48899809210487));
#59607=CARTESIAN_POINT('',(0.,8.78233410394347,-3.48899809210487));
#59608=CARTESIAN_POINT('',(0.,8.47747275224749,-4.17551861867497));
#59609=CARTESIAN_POINT('',(0.,8.47747275224749,-4.17551861867497));
#59610=CARTESIAN_POINT('',(0.,8.11904715054109,-4.83565645670685));
#59611=CARTESIAN_POINT('',(0.,8.11904715054109,-4.83565645670685));
#59612=CARTESIAN_POINT('',(0.,7.70932198301742,-5.46524057678747));
#59613=CARTESIAN_POINT('',(0.,7.70932198301742,-5.46524057678747));
#59614=CARTESIAN_POINT('',(0.,7.25088606617289,-6.06029300078633));
#59615=CARTESIAN_POINT('',(0.,7.25088606617289,-6.06029300078633));
#59616=CARTESIAN_POINT('',(0.,6.74663599157214,-6.61705393639975));
#59617=CARTESIAN_POINT('',(0.,6.74663599157214,-6.61705393639975));
#59618=CARTESIAN_POINT('',(0.,6.19975782396029,-7.1320055331052));
#59619=CARTESIAN_POINT('',(0.,6.19975782396029,-7.1320055331052));
#59620=CARTESIAN_POINT('',(0.,5.61370697036149,-7.60189410942528));
#59621=CARTESIAN_POINT('',(0.,5.61370697036149,-7.60189410942528));
#59622=CARTESIAN_POINT('',(0.,4.99218634735931,-8.02375071106021));
#59623=CARTESIAN_POINT('',(0.,4.99218634735931,-8.02375071106021));
#59624=CARTESIAN_POINT('',(0.,4.33912298450726,-8.39490986999389));
#59625=CARTESIAN_POINT('',(0.,4.33912298450726,-8.39490986999389));
#59626=CARTESIAN_POINT('',(0.,3.658643211699,-8.71302644604553));
#59627=CARTESIAN_POINT('',(0.,3.658643211699,-8.71302644604553));
#59628=CARTESIAN_POINT('',(0.,2.95504658727499,-8.97609044445489));
#59629=CARTESIAN_POINT('',(0.,2.95504658727499,-8.97609044445489));
#59630=CARTESIAN_POINT('',(0.,2.23277873159856,-9.18243971587732));
#59631=CARTESIAN_POINT('',(0.,2.23277873159856,-9.18243971587732));
#59632=CARTESIAN_POINT('',(0.,1.49640323775065,-9.33077045854464));
#59633=CARTESIAN_POINT('',(0.,1.49640323775065,-9.33077045854464));
#59634=CARTESIAN_POINT('',(0.,0.750572836823028,-9.42014545623492));
#59635=CARTESIAN_POINT('',(0.,0.750572836823028,-9.42014545623492));
#59636=CARTESIAN_POINT('',(0.,-1.73593683779137E-15,-9.45));
#59637=CARTESIAN_POINT('',(0.,-1.73593683779137E-15,-9.45));
#59638=CARTESIAN_POINT('',(0.,-0.750572836823032,-9.42014545623492));
#59639=CARTESIAN_POINT('',(0.,-0.750572836823032,-9.42014545623492));
#59640=CARTESIAN_POINT('',(0.,-1.49640323775065,-9.33077045854464));
#59641=CARTESIAN_POINT('',(0.,-1.49640323775065,-9.33077045854464));
#59642=CARTESIAN_POINT('',(0.,-2.23277873159856,-9.18243971587732));
#59643=CARTESIAN_POINT('',(0.,-2.23277873159856,-9.18243971587732));
#59644=CARTESIAN_POINT('',(0.,-2.95504658727499,-8.97609044445489));
#59645=CARTESIAN_POINT('',(0.,-2.95504658727499,-8.97609044445489));
#59646=CARTESIAN_POINT('',(0.,-3.65864321169901,-8.71302644604553));
#59647=CARTESIAN_POINT('',(0.,-3.65864321169901,-8.71302644604553));
#59648=CARTESIAN_POINT('',(0.,-4.33912298450726,-8.39490986999389));
#59649=CARTESIAN_POINT('',(0.,-4.33912298450726,-8.39490986999389));
#59650=CARTESIAN_POINT('',(0.,-4.99218634735932,-8.02375071106021));
#59651=CARTESIAN_POINT('',(0.,-4.99218634735932,-8.02375071106021));
#59652=CARTESIAN_POINT('',(0.,-5.6137069703615,-7.60189410942528));
#59653=CARTESIAN_POINT('',(0.,-5.6137069703615,-7.60189410942528));
#59654=CARTESIAN_POINT('',(0.,-6.1997578239603,-7.13200553310519));
#59655=CARTESIAN_POINT('',(0.,-6.1997578239603,-7.13200553310519));
#59656=CARTESIAN_POINT('',(0.,-6.74663599157215,-6.61705393639974));
#59657=CARTESIAN_POINT('',(0.,-6.74663599157215,-6.61705393639974));
#59658=CARTESIAN_POINT('',(0.,-7.2508860661729,-6.06029300078632));
#59659=CARTESIAN_POINT('',(0.,-7.2508860661729,-6.06029300078632));
#59660=CARTESIAN_POINT('',(0.,-7.70932198301743,-5.46524057678747));
#59661=CARTESIAN_POINT('',(0.,-7.70932198301743,-5.46524057678747));
#59662=CARTESIAN_POINT('',(0.,-8.11904715054109,-4.83565645670684));
#59663=CARTESIAN_POINT('',(0.,-8.11904715054109,-4.83565645670684));
#59664=CARTESIAN_POINT('',(0.,-8.47747275224749,-4.17551861867497));
#59665=CARTESIAN_POINT('',(0.,-8.47747275224749,-4.17551861867497));
#59666=CARTESIAN_POINT('',(0.,-8.78233410394347,-3.48899809210486));
#59667=CARTESIAN_POINT('',(0.,-8.78233410394347,-3.48899809210486));
#59668=CARTESIAN_POINT('',(0.,-9.03170496296946,-2.7804326033682));
#59669=CARTESIAN_POINT('',(0.,-9.03170496296946,-2.7804326033682));
#59670=CARTESIAN_POINT('',(0.,-9.22400969901338,-2.0542991682097));
#59671=CARTESIAN_POINT('',(0.,-9.22400969901338,-2.0542991682097));
#59672=CARTESIAN_POINT('',(0.,-9.35803324960784,-1.31518580407261));
#59673=CARTESIAN_POINT('',(0.,-9.35803324960784,-1.31518580407261));
#59674=CARTESIAN_POINT('',(0.,-9.43292879740749,-0.567762541068457));
#59675=CARTESIAN_POINT('',(0.,-9.43292879740749,-0.567762541068457));
#59676=CARTESIAN_POINT('',(0.,-9.44822312073834,0.183248085243744));
#59677=CARTESIAN_POINT('',(0.,-9.44822312073834,0.183248085243744));
#59678=CARTESIAN_POINT('',(0.,-9.40381958361198,0.933100872829854));
#59679=CARTESIAN_POINT('',(0.,-9.40381958361198,0.933100872829854));
#59680=CARTESIAN_POINT('',(0.,-9.29999874631253,1.67705793536938));
#59681=CARTESIAN_POINT('',(0.,-9.29999874631253,1.67705793536938));
#59682=CARTESIAN_POINT('',(0.,-9.13741659269838,2.41041863822042));
#59683=CARTESIAN_POINT('',(0.,-9.13741659269838,2.41041863822042));
#59684=CARTESIAN_POINT('',(0.,-8.91710038541936,3.12854929901286));
#59685=CARTESIAN_POINT('',(0.,-8.91710038541936,3.12854929901286));
#59686=CARTESIAN_POINT('',(0.,-8.64044217523789,3.82691246520877));
#59687=CARTESIAN_POINT('',(0.,-8.64044217523789,3.82691246520877));
#59688=CARTESIAN_POINT('',(0.,-8.30919000546483,4.5010955836422));
#59689=CARTESIAN_POINT('',(0.,-8.30919000546483,4.5010955836422));
#59690=CARTESIAN_POINT('',(0.,-7.92543686708426,5.14683888089201));
#59691=CARTESIAN_POINT('',(0.,-7.92543686708426,5.14683888089201));
#59692=CARTESIAN_POINT('',(0.,-7.49160747435326,5.76006227832776));
#59693=CARTESIAN_POINT('',(0.,-7.49160747435326,5.76006227832776));
#59694=CARTESIAN_POINT('',(0.,-7.01044294443414,6.33689117176819));
#59695=CARTESIAN_POINT('',(0.,-7.01044294443414,6.33689117176819));
#59696=CARTESIAN_POINT('',(0.,-6.48498347785953,6.87368091286531));
#59697=CARTESIAN_POINT('',(0.,-6.48498347785953,6.87368091286531));
#59698=CARTESIAN_POINT('',(0.,-5.91854914926258,7.36703983753062));
#59699=CARTESIAN_POINT('',(0.,-5.91854914926258,7.36703983753062));
#59700=CARTESIAN_POINT('',(0.,-5.31471892974448,7.81385069589992));
#59701=CARTESIAN_POINT('',(0.,-5.31471892974448,7.81385069589992));
#59702=CARTESIAN_POINT('',(0.,-4.67730807342486,8.21129034843335));
#59703=CARTESIAN_POINT('',(0.,-4.67730807342486,8.21129034843335));
#59704=CARTESIAN_POINT('',(0.,-4.01034401105639,8.5568476037022));
#59705=CARTESIAN_POINT('',(0.,-4.01034401105639,8.5568476037022));
#59706=CARTESIAN_POINT('',(0.,-3.31804090301785,8.84833908515606));
#59707=CARTESIAN_POINT('',(0.,-3.31804090301785,8.84833908515606));
#59708=CARTESIAN_POINT('',(0.,-2.60477301247064,9.08392302661711));
#59709=CARTESIAN_POINT('',(0.,2.88925991435643,7.72529047046021));
#59710=CARTESIAN_POINT('Origin',(0.,2.88925991435643,6.97529047046021));
#59711=CARTESIAN_POINT('Origin',(0.9,-2.88925991435643,6.97529047046021));
#59712=CARTESIAN_POINT('',(1.,-2.88925991435643,7.72529047046022));
#59713=CARTESIAN_POINT('Origin',(1.,-2.88925991435643,6.97529047046021));
#59714=CARTESIAN_POINT('',(0.9,-2.88925991435643,7.62529047046022));
#59715=CARTESIAN_POINT('Origin',(1.,0.,-0.183038486691444));
#59716=CARTESIAN_POINT('',(1.,-1.84677028397389,6.44045336278674));
#59717=CARTESIAN_POINT('',(1.,-2.60477301247064,9.08392302661711));
#59718=CARTESIAN_POINT('',(1.,-1.84677028397389,6.44045336278674));
#59719=CARTESIAN_POINT('',(1.,-3.31804090301785,8.84833908515606));
#59720=CARTESIAN_POINT('',(1.,-2.60477301247064,9.08392302661711));
#59721=CARTESIAN_POINT('',(1.,-4.01034401105639,8.5568476037022));
#59722=CARTESIAN_POINT('',(1.,-3.31804090301785,8.84833908515606));
#59723=CARTESIAN_POINT('',(1.,-4.67730807342486,8.21129034843335));
#59724=CARTESIAN_POINT('',(1.,-4.01034401105639,8.5568476037022));
#59725=CARTESIAN_POINT('',(1.,-5.31471892974448,7.81385069589992));
#59726=CARTESIAN_POINT('',(1.,-4.67730807342486,8.21129034843335));
#59727=CARTESIAN_POINT('',(1.,-5.91854914926258,7.36703983753062));
#59728=CARTESIAN_POINT('',(1.,-5.31471892974448,7.81385069589992));
#59729=CARTESIAN_POINT('',(1.,-6.48498347785953,6.87368091286531));
#59730=CARTESIAN_POINT('',(1.,-5.91854914926258,7.36703983753062));
#59731=CARTESIAN_POINT('',(1.,-7.01044294443414,6.33689117176819));
#59732=CARTESIAN_POINT('',(1.,-6.48498347785953,6.87368091286531));
#59733=CARTESIAN_POINT('',(1.,-7.49160747435326,5.76006227832776));
#59734=CARTESIAN_POINT('',(1.,-7.01044294443414,6.33689117176819));
#59735=CARTESIAN_POINT('',(1.,-7.92543686708425,5.14683888089201));
#59736=CARTESIAN_POINT('',(1.,-7.49160747435326,5.76006227832776));
#59737=CARTESIAN_POINT('',(1.,-8.30919000546483,4.5010955836422));
#59738=CARTESIAN_POINT('',(1.,-7.92543686708426,5.14683888089201));
#59739=CARTESIAN_POINT('',(1.,-8.64044217523789,3.82691246520877));
#59740=CARTESIAN_POINT('',(1.,-8.30919000546483,4.5010955836422));
#59741=CARTESIAN_POINT('',(1.,-8.91710038541936,3.12854929901286));
#59742=CARTESIAN_POINT('',(1.,-8.64044217523789,3.82691246520877));
#59743=CARTESIAN_POINT('',(1.,-9.13741659269838,2.41041863822042));
#59744=CARTESIAN_POINT('',(1.,-8.91710038541936,3.12854929901286));
#59745=CARTESIAN_POINT('',(1.,-9.29999874631253,1.67705793536937));
#59746=CARTESIAN_POINT('',(1.,-9.13741659269838,2.41041863822042));
#59747=CARTESIAN_POINT('',(1.,-9.40381958361198,0.933100872829854));
#59748=CARTESIAN_POINT('',(1.,-9.29999874631253,1.67705793536938));
#59749=CARTESIAN_POINT('',(1.,-9.44822312073834,0.183248085243743));
#59750=CARTESIAN_POINT('',(1.,-9.40381958361198,0.933100872829854));
#59751=CARTESIAN_POINT('',(1.,-9.43292879740749,-0.567762541068457));
#59752=CARTESIAN_POINT('',(1.,-9.44822312073834,0.183248085243744));
#59753=CARTESIAN_POINT('',(1.,-9.35803324960784,-1.31518580407261));
#59754=CARTESIAN_POINT('',(1.,-9.43292879740749,-0.567762541068457));
#59755=CARTESIAN_POINT('',(1.,-9.22400969901338,-2.0542991682097));
#59756=CARTESIAN_POINT('',(1.,-9.35803324960784,-1.31518580407261));
#59757=CARTESIAN_POINT('',(1.,-9.03170496296946,-2.7804326033682));
#59758=CARTESIAN_POINT('',(1.,-9.22400969901338,-2.0542991682097));
#59759=CARTESIAN_POINT('',(1.,-8.78233410394347,-3.48899809210486));
#59760=CARTESIAN_POINT('',(1.,-9.03170496296946,-2.7804326033682));
#59761=CARTESIAN_POINT('',(1.,-8.47747275224749,-4.17551861867497));
#59762=CARTESIAN_POINT('',(1.,-8.78233410394347,-3.48899809210486));
#59763=CARTESIAN_POINT('',(1.,-8.11904715054109,-4.83565645670684));
#59764=CARTESIAN_POINT('',(1.,-8.47747275224749,-4.17551861867497));
#59765=CARTESIAN_POINT('',(1.,-7.70932198301743,-5.46524057678747));
#59766=CARTESIAN_POINT('',(1.,-8.11904715054109,-4.83565645670684));
#59767=CARTESIAN_POINT('',(1.,-7.2508860661729,-6.06029300078632));
#59768=CARTESIAN_POINT('',(1.,-7.70932198301743,-5.46524057678747));
#59769=CARTESIAN_POINT('',(1.,-6.74663599157215,-6.61705393639974));
#59770=CARTESIAN_POINT('',(1.,-7.2508860661729,-6.06029300078632));
#59771=CARTESIAN_POINT('',(1.,-6.1997578239603,-7.13200553310519));
#59772=CARTESIAN_POINT('',(1.,-6.74663599157215,-6.61705393639974));
#59773=CARTESIAN_POINT('',(1.,-5.6137069703615,-7.60189410942528));
#59774=CARTESIAN_POINT('',(1.,-6.1997578239603,-7.13200553310519));
#59775=CARTESIAN_POINT('',(1.,-4.99218634735932,-8.02375071106021));
#59776=CARTESIAN_POINT('',(1.,-5.6137069703615,-7.60189410942528));
#59777=CARTESIAN_POINT('',(1.,-4.33912298450726,-8.39490986999389));
#59778=CARTESIAN_POINT('',(1.,-4.99218634735932,-8.02375071106021));
#59779=CARTESIAN_POINT('',(1.,-3.65864321169901,-8.71302644604553));
#59780=CARTESIAN_POINT('',(1.,-4.33912298450726,-8.39490986999389));
#59781=CARTESIAN_POINT('',(1.,-2.95504658727499,-8.97609044445489));
#59782=CARTESIAN_POINT('',(1.,-3.65864321169901,-8.71302644604553));
#59783=CARTESIAN_POINT('',(1.,-2.23277873159856,-9.18243971587732));
#59784=CARTESIAN_POINT('',(1.,-2.95504658727499,-8.97609044445489));
#59785=CARTESIAN_POINT('',(1.,-1.49640323775065,-9.33077045854464));
#59786=CARTESIAN_POINT('',(1.,-2.23277873159856,-9.18243971587732));
#59787=CARTESIAN_POINT('',(1.,-0.750572836823032,-9.42014545623492));
#59788=CARTESIAN_POINT('',(1.,-1.49640323775065,-9.33077045854464));
#59789=CARTESIAN_POINT('',(1.,-1.66533453693773E-15,-9.45));
#59790=CARTESIAN_POINT('',(1.,-0.750572836823032,-9.42014545623492));
#59791=CARTESIAN_POINT('',(1.,0.750572836823029,-9.42014545623492));
#59792=CARTESIAN_POINT('',(1.,-1.73593683779137E-15,-9.45));
#59793=CARTESIAN_POINT('',(1.,1.49640323775065,-9.33077045854464));
#59794=CARTESIAN_POINT('',(1.,0.750572836823028,-9.42014545623492));
#59795=CARTESIAN_POINT('',(1.,2.23277873159856,-9.18243971587732));
#59796=CARTESIAN_POINT('',(1.,1.49640323775065,-9.33077045854464));
#59797=CARTESIAN_POINT('',(1.,2.95504658727499,-8.9760904444549));
#59798=CARTESIAN_POINT('',(1.,2.23277873159856,-9.18243971587732));
#59799=CARTESIAN_POINT('',(1.,3.658643211699,-8.71302644604553));
#59800=CARTESIAN_POINT('',(1.,2.95504658727499,-8.97609044445489));
#59801=CARTESIAN_POINT('',(1.,4.33912298450726,-8.39490986999389));
#59802=CARTESIAN_POINT('',(1.,3.658643211699,-8.71302644604553));
#59803=CARTESIAN_POINT('',(1.,4.99218634735931,-8.02375071106021));
#59804=CARTESIAN_POINT('',(1.,4.33912298450726,-8.39490986999389));
#59805=CARTESIAN_POINT('',(1.,5.6137069703615,-7.60189410942528));
#59806=CARTESIAN_POINT('',(1.,4.99218634735931,-8.02375071106021));
#59807=CARTESIAN_POINT('',(1.,6.19975782396029,-7.1320055331052));
#59808=CARTESIAN_POINT('',(1.,5.61370697036149,-7.60189410942528));
#59809=CARTESIAN_POINT('',(1.,6.74663599157214,-6.61705393639975));
#59810=CARTESIAN_POINT('',(1.,6.19975782396029,-7.1320055331052));
#59811=CARTESIAN_POINT('',(1.,7.25088606617289,-6.06029300078633));
#59812=CARTESIAN_POINT('',(1.,6.74663599157214,-6.61705393639975));
#59813=CARTESIAN_POINT('',(1.,7.70932198301742,-5.46524057678747));
#59814=CARTESIAN_POINT('',(1.,7.25088606617289,-6.06029300078633));
#59815=CARTESIAN_POINT('',(1.,8.11904715054109,-4.83565645670685));
#59816=CARTESIAN_POINT('',(1.,7.70932198301742,-5.46524057678747));
#59817=CARTESIAN_POINT('',(1.,8.47747275224749,-4.17551861867497));
#59818=CARTESIAN_POINT('',(1.,8.11904715054109,-4.83565645670685));
#59819=CARTESIAN_POINT('',(1.,8.78233410394347,-3.48899809210487));
#59820=CARTESIAN_POINT('',(1.,8.47747275224749,-4.17551861867497));
#59821=CARTESIAN_POINT('',(1.,9.03170496296946,-2.7804326033682));
#59822=CARTESIAN_POINT('',(1.,8.78233410394347,-3.48899809210487));
#59823=CARTESIAN_POINT('',(1.,9.22400969901338,-2.05429916820971));
#59824=CARTESIAN_POINT('',(1.,9.03170496296946,-2.7804326033682));
#59825=CARTESIAN_POINT('',(1.,9.35803324960784,-1.31518580407262));
#59826=CARTESIAN_POINT('',(1.,9.22400969901338,-2.05429916820971));
#59827=CARTESIAN_POINT('',(1.,9.43292879740749,-0.567762541068465));
#59828=CARTESIAN_POINT('',(1.,9.35803324960784,-1.31518580407262));
#59829=CARTESIAN_POINT('',(1.,9.44822312073834,0.183248085243736));
#59830=CARTESIAN_POINT('',(1.,9.43292879740749,-0.567762541068464));
#59831=CARTESIAN_POINT('',(1.,9.40381958361198,0.933100872829846));
#59832=CARTESIAN_POINT('',(1.,9.44822312073834,0.183248085243736));
#59833=CARTESIAN_POINT('',(1.,9.29999874631253,1.67705793536937));
#59834=CARTESIAN_POINT('',(1.,9.40381958361198,0.933100872829846));
#59835=CARTESIAN_POINT('',(1.,9.13741659269838,2.41041863822041));
#59836=CARTESIAN_POINT('',(1.,9.29999874631253,1.67705793536937));
#59837=CARTESIAN_POINT('',(1.,8.91710038541937,3.12854929901285));
#59838=CARTESIAN_POINT('',(1.,9.13741659269838,2.41041863822041));
#59839=CARTESIAN_POINT('',(1.,8.6404421752379,3.82691246520876));
#59840=CARTESIAN_POINT('',(1.,8.91710038541937,3.12854929901285));
#59841=CARTESIAN_POINT('',(1.,8.30919000546483,4.5010955836422));
#59842=CARTESIAN_POINT('',(1.,8.6404421752379,3.82691246520876));
#59843=CARTESIAN_POINT('',(1.,7.92543686708426,5.146838880892));
#59844=CARTESIAN_POINT('',(1.,8.30919000546483,4.5010955836422));
#59845=CARTESIAN_POINT('',(1.,7.49160747435326,5.76006227832775));
#59846=CARTESIAN_POINT('',(1.,7.92543686708426,5.146838880892));
#59847=CARTESIAN_POINT('',(1.,7.01044294443415,6.33689117176818));
#59848=CARTESIAN_POINT('',(1.,7.49160747435326,5.76006227832775));
#59849=CARTESIAN_POINT('',(1.,6.48498347785954,6.87368091286531));
#59850=CARTESIAN_POINT('',(1.,7.01044294443415,6.33689117176818));
#59851=CARTESIAN_POINT('',(1.,5.91854914926258,7.36703983753062));
#59852=CARTESIAN_POINT('',(1.,6.48498347785954,6.87368091286531));
#59853=CARTESIAN_POINT('',(1.,5.31471892974448,7.81385069589992));
#59854=CARTESIAN_POINT('',(1.,5.91854914926258,7.36703983753062));
#59855=CARTESIAN_POINT('',(1.,4.67730807342487,8.21129034843334));
#59856=CARTESIAN_POINT('',(1.,5.31471892974448,7.81385069589992));
#59857=CARTESIAN_POINT('',(1.,4.0103440110564,8.5568476037022));
#59858=CARTESIAN_POINT('',(1.,4.67730807342487,8.21129034843334));
#59859=CARTESIAN_POINT('',(1.,3.31804090301786,8.84833908515606));
#59860=CARTESIAN_POINT('',(1.,4.0103440110564,8.5568476037022));
#59861=CARTESIAN_POINT('',(1.,2.60477301247065,9.08392302661711));
#59862=CARTESIAN_POINT('',(1.,3.31804090301786,8.84833908515606));
#59863=CARTESIAN_POINT('',(1.,1.8467702839739,6.44045336278674));
#59864=CARTESIAN_POINT('',(1.,2.60477301247065,9.08392302661711));
#59865=CARTESIAN_POINT('',(1.,3.24822445565046,5.85995203783395));
#59866=CARTESIAN_POINT('',(1.,1.8467702839739,6.44045336278674));
#59867=CARTESIAN_POINT('',(1.,3.8784769619707,6.99695765711516));
#59868=CARTESIAN_POINT('',(1.,3.24822445565046,5.85995203783395));
#59869=CARTESIAN_POINT('',(1.,4.37985668768992,6.69453922202999));
#59870=CARTESIAN_POINT('',(1.,3.8784769619707,6.99695765711516));
#59871=CARTESIAN_POINT('',(1.,4.85777416858264,6.35625912994831));
#59872=CARTESIAN_POINT('',(1.,4.37985668768992,6.69453922202999));
#59873=CARTESIAN_POINT('',(1.,5.30966927135158,5.98392949731736));
#59874=CARTESIAN_POINT('',(1.,4.85777416858264,6.35625912994831));
#59875=CARTESIAN_POINT('',(1.,5.73312126073229,5.57954483893976));
#59876=CARTESIAN_POINT('',(1.,5.30966927135158,5.98392949731736));
#59877=CARTESIAN_POINT('',(1.,6.12586176701418,5.14527138365256));
#59878=CARTESIAN_POINT('',(1.,5.73312126073229,5.57954483893976));
#59879=CARTESIAN_POINT('',(1.,6.4857869373617,4.68343547015952));
#59880=CARTESIAN_POINT('',(1.,6.12586176701418,5.14527138365256));
#59881=CARTESIAN_POINT('',(1.,6.81096870584301,4.19651108517863));
#59882=CARTESIAN_POINT('',(1.,6.4857869373617,4.68343547015952));
#59883=CARTESIAN_POINT('',(1.,7.09966512179414,3.68710661066097));
#59884=CARTESIAN_POINT('',(1.,6.81096870584301,4.19651108517863));
#59885=CARTESIAN_POINT('',(1.,7.35032968119119,3.15795085107413));
#59886=CARTESIAN_POINT('',(1.,7.09966512179414,3.68710661066097));
#59887=CARTESIAN_POINT('',(1.,7.5616196110438,2.61187841560012));
#59888=CARTESIAN_POINT('',(1.,7.35032968119119,3.15795085107413));
#59889=CARTESIAN_POINT('',(1.,7.73240306243155,2.05181453355297));
#59890=CARTESIAN_POINT('',(1.,7.5616196110438,2.61187841560012));
#59891=CARTESIAN_POINT('',(1.,7.86176517365131,1.48075938435771));
#59892=CARTESIAN_POINT('',(1.,7.73240306243155,2.05181453355297));
#59893=CARTESIAN_POINT('',(1.,7.94901297099613,0.901772026032747));
#59894=CARTESIAN_POINT('',(1.,7.86176517365131,1.48075938435771));
#59895=CARTESIAN_POINT('',(1.,7.99367908091301,0.317954008268194));
#59896=CARTESIAN_POINT('',(1.,7.94901297099613,0.901772026032747));
#59897=CARTESIAN_POINT('',(1.,7.99552423365383,-0.267567242117314));
#59898=CARTESIAN_POINT('',(1.,7.99367908091301,0.317954008268194));
#59899=CARTESIAN_POINT('',(1.,7.95453854500815,-0.851655174339753));
#59900=CARTESIAN_POINT('',(1.,7.99552423365383,-0.267567242117314));
#59901=CARTESIAN_POINT('',(1.,7.87094156925134,-1.43118091568862));
#59902=CARTESIAN_POINT('',(1.,7.95453854500815,-0.851655174339752));
#59903=CARTESIAN_POINT('',(1.,7.74518112302486,-2.00304003243554));
#59904=CARTESIAN_POINT('',(1.,7.87094156925134,-1.43118091568862));
#59905=CARTESIAN_POINT('',(1.,7.5779308864487,-2.56416915982678));
#59906=CARTESIAN_POINT('',(1.,7.74518112302486,-2.00304003243554));
#59907=CARTESIAN_POINT('',(1.,7.37008679431654,-3.11156241207547));
#59908=CARTESIAN_POINT('',(1.,7.5779308864487,-2.56416915982678));
#59909=CARTESIAN_POINT('',(1.,7.12276223670551,-3.64228748444737));
#59910=CARTESIAN_POINT('',(1.,7.37008679431654,-3.11156241207547));
#59911=CARTESIAN_POINT('',(1.,6.83728209471014,-4.15350136118385));
#59912=CARTESIAN_POINT('',(1.,7.12276223670551,-3.64228748444737));
#59913=CARTESIAN_POINT('',(1.,6.51517564325019,-4.64246554511711));
#59914=CARTESIAN_POINT('',(1.,6.83728209471014,-4.15350136118385));
#59915=CARTESIAN_POINT('',(1.,6.15816835897094,-5.10656072739463));
#59916=CARTESIAN_POINT('',(1.,6.51517564325019,-4.64246554511711));
#59917=CARTESIAN_POINT('',(1.,5.76817267711992,-5.54330081872951));
#59918=CARTESIAN_POINT('',(1.,6.15816835897094,-5.10656072739463));
#59919=CARTESIAN_POINT('',(1.,5.34727774691393,-5.95034626701329));
#59920=CARTESIAN_POINT('',(1.,5.76817267711992,-5.54330081872951));
#59921=CARTESIAN_POINT('',(1.,4.89773824027559,-6.32551658995075));
#59922=CARTESIAN_POINT('',(1.,5.34727774691393,-5.95034626701329));
#59923=CARTESIAN_POINT('',(1.,4.42196227388906,-6.66680205558121));
#59924=CARTESIAN_POINT('',(1.,4.89773824027559,-6.32551658995075));
#59925=CARTESIAN_POINT('',(1.,3.922498509275,-6.97237444811561));
#59926=CARTESIAN_POINT('',(1.,4.42196227388906,-6.66680205558121));
#59927=CARTESIAN_POINT('',(1.,3.40202249998754,-7.24059686141816));
#59928=CARTESIAN_POINT('',(1.,3.922498509275,-6.97237444811561));
#59929=CARTESIAN_POINT('',(1.,2.86332235906941,-7.47003246767062));
#59930=CARTESIAN_POINT('',(1.,3.40202249998754,-7.24059686141816));
#59931=CARTESIAN_POINT('',(1.,2.30928382354251,-7.65945221424645));
#59932=CARTESIAN_POINT('',(1.,2.86332235906941,-7.47003246767062));
#59933=CARTESIAN_POINT('',(1.,1.74287479594128,-7.80784140756411));
#59934=CARTESIAN_POINT('',(1.,2.30928382354251,-7.65945221424645));
#59935=CARTESIAN_POINT('',(1.,1.16712944569751,-7.91440514865052));
#59936=CARTESIAN_POINT('',(1.,1.74287479594128,-7.80784140756411));
#59937=CARTESIAN_POINT('',(1.,0.585131955543308,-7.9785725912974));
#59938=CARTESIAN_POINT('',(1.,1.16712944569752,-7.91440514865052));
#59939=CARTESIAN_POINT('',(1.,-1.38777878078145E-15,-8.));
#59940=CARTESIAN_POINT('',(1.,0.585131955543308,-7.9785725912974));
#59941=CARTESIAN_POINT('',(1.,-0.585131955543311,-7.9785725912974));
#59942=CARTESIAN_POINT('',(1.,-1.46957615897682E-15,-8.));
#59943=CARTESIAN_POINT('',(1.,-1.16712944569752,-7.91440514865052));
#59944=CARTESIAN_POINT('',(1.,-0.585131955543311,-7.9785725912974));
#59945=CARTESIAN_POINT('',(1.,-1.74287479594128,-7.80784140756411));
#59946=CARTESIAN_POINT('',(1.,-1.16712944569752,-7.91440514865052));
#59947=CARTESIAN_POINT('',(1.,-2.30928382354251,-7.65945221424645));
#59948=CARTESIAN_POINT('',(1.,-1.74287479594128,-7.80784140756411));
#59949=CARTESIAN_POINT('',(1.,-2.86332235906941,-7.47003246767062));
#59950=CARTESIAN_POINT('',(1.,-2.30928382354251,-7.65945221424645));
#59951=CARTESIAN_POINT('',(1.,-3.40202249998754,-7.24059686141816));
#59952=CARTESIAN_POINT('',(1.,-2.86332235906941,-7.47003246767062));
#59953=CARTESIAN_POINT('',(1.,-3.922498509275,-6.9723744481156));
#59954=CARTESIAN_POINT('',(1.,-3.40202249998754,-7.24059686141816));
#59955=CARTESIAN_POINT('',(1.,-4.42196227388907,-6.66680205558121));
#59956=CARTESIAN_POINT('',(1.,-3.922498509275,-6.9723744481156));
#59957=CARTESIAN_POINT('',(1.,-4.89773824027559,-6.32551658995075));
#59958=CARTESIAN_POINT('',(1.,-4.42196227388907,-6.66680205558121));
#59959=CARTESIAN_POINT('',(1.,-5.34727774691394,-5.95034626701329));
#59960=CARTESIAN_POINT('',(1.,-4.89773824027559,-6.32551658995075));
#59961=CARTESIAN_POINT('',(1.,-5.76817267711992,-5.54330081872951));
#59962=CARTESIAN_POINT('',(1.,-5.34727774691394,-5.95034626701329));
#59963=CARTESIAN_POINT('',(1.,-6.15816835897094,-5.10656072739463));
#59964=CARTESIAN_POINT('',(1.,-5.76817267711992,-5.54330081872951));
#59965=CARTESIAN_POINT('',(1.,-6.51517564325019,-4.64246554511711));
#59966=CARTESIAN_POINT('',(1.,-6.15816835897094,-5.10656072739463));
#59967=CARTESIAN_POINT('',(1.,-6.83728209471014,-4.15350136118385));
#59968=CARTESIAN_POINT('',(1.,-6.51517564325019,-4.64246554511711));
#59969=CARTESIAN_POINT('',(1.,-7.12276223670551,-3.64228748444736));
#59970=CARTESIAN_POINT('',(1.,-6.83728209471014,-4.15350136118385));
#59971=CARTESIAN_POINT('',(1.,-7.37008679431654,-3.11156241207547));
#59972=CARTESIAN_POINT('',(1.,-7.12276223670551,-3.64228748444736));
#59973=CARTESIAN_POINT('',(1.,-7.5779308864487,-2.56416915982678));
#59974=CARTESIAN_POINT('',(1.,-7.37008679431654,-3.11156241207547));
#59975=CARTESIAN_POINT('',(1.,-7.74518112302486,-2.00304003243553));
#59976=CARTESIAN_POINT('',(1.,-7.5779308864487,-2.56416915982678));
#59977=CARTESIAN_POINT('',(1.,-7.87094156925134,-1.43118091568862));
#59978=CARTESIAN_POINT('',(1.,-7.74518112302486,-2.00304003243553));
#59979=CARTESIAN_POINT('',(1.,-7.95453854500815,-0.851655174339749));
#59980=CARTESIAN_POINT('',(1.,-7.87094156925134,-1.43118091568862));
#59981=CARTESIAN_POINT('',(1.,-7.99552423365383,-0.26756724211731));
#59982=CARTESIAN_POINT('',(1.,-7.95453854500815,-0.85165517433975));
#59983=CARTESIAN_POINT('',(1.,-7.99367908091301,0.317954008268198));
#59984=CARTESIAN_POINT('',(1.,-7.99552423365383,-0.267567242117311));
#59985=CARTESIAN_POINT('',(1.,-7.94901297099613,0.901772026032757));
#59986=CARTESIAN_POINT('',(1.,-7.99367908091301,0.317954008268197));
#59987=CARTESIAN_POINT('',(1.,-7.86176517365131,1.48075938435771));
#59988=CARTESIAN_POINT('',(1.,-7.94901297099613,0.901772026032757));
#59989=CARTESIAN_POINT('',(1.,-7.73240306243155,2.05181453355296));
#59990=CARTESIAN_POINT('',(1.,-7.86176517365131,1.48075938435772));
#59991=CARTESIAN_POINT('',(1.,-7.5616196110438,2.61187841560012));
#59992=CARTESIAN_POINT('',(1.,-7.73240306243155,2.05181453355296));
#59993=CARTESIAN_POINT('',(1.,-7.35032968119119,3.15795085107414));
#59994=CARTESIAN_POINT('',(1.,-7.5616196110438,2.61187841560012));
#59995=CARTESIAN_POINT('',(1.,-7.09966512179413,3.68710661066098));
#59996=CARTESIAN_POINT('',(1.,-7.35032968119119,3.15795085107414));
#59997=CARTESIAN_POINT('',(1.,-6.81096870584301,4.19651108517864));
#59998=CARTESIAN_POINT('',(1.,-7.09966512179413,3.68710661066098));
#59999=CARTESIAN_POINT('',(1.,-6.4857869373617,4.68343547015952));
#60000=CARTESIAN_POINT('',(1.,-6.81096870584301,4.19651108517864));
#60001=CARTESIAN_POINT('',(1.,-6.12586176701418,5.14527138365256));
#60002=CARTESIAN_POINT('',(1.,-6.4857869373617,4.68343547015952));
#60003=CARTESIAN_POINT('',(1.,-5.73312126073229,5.57954483893977));
#60004=CARTESIAN_POINT('',(1.,-6.12586176701418,5.14527138365256));
#60005=CARTESIAN_POINT('',(1.,-5.30966927135158,5.98392949731736));
#60006=CARTESIAN_POINT('',(1.,-5.73312126073229,5.57954483893977));
#60007=CARTESIAN_POINT('',(1.,-4.85777416858265,6.3562591299483));
#60008=CARTESIAN_POINT('',(1.,-5.30966927135158,5.98392949731736));
#60009=CARTESIAN_POINT('',(1.,-4.37985668768992,6.69453922202999));
#60010=CARTESIAN_POINT('',(1.,-4.85777416858265,6.3562591299483));
#60011=CARTESIAN_POINT('',(1.,-3.8784769619707,6.99695765711517));
#60012=CARTESIAN_POINT('',(1.,-4.37985668768992,6.69453922202999));
#60013=CARTESIAN_POINT('',(1.,-3.24822445565046,5.85995203783395));
#60014=CARTESIAN_POINT('',(1.,-3.8784769619707,6.99695765711517));
#60015=CARTESIAN_POINT('',(1.,-3.24822445565046,5.85995203783395));
#60016=CARTESIAN_POINT('',(1.,2.88925991435643,7.72529047046021));
#60017=CARTESIAN_POINT('Origin',(1.,2.88925991435643,6.97529047046021));
#60018=CARTESIAN_POINT('Origin',(0.1,2.88925991435643,6.97529047046021));
#60019=CARTESIAN_POINT('',(0.2,2.88925991435643,7.52529047046021));
#60020=CARTESIAN_POINT('',(0.1,2.88925991435643,7.62529047046021));
#60021=CARTESIAN_POINT('Origin',(0.2,2.88925991435643,6.97529047046021));
#60022=CARTESIAN_POINT('Origin',(0.,2.88925991435643,6.97529047046021));
#60023=CARTESIAN_POINT('',(0.8,2.88925991435643,7.52529047046021));
#60024=CARTESIAN_POINT('',(0.,2.88925991435643,7.52529047046021));
#60025=CARTESIAN_POINT('Origin',(0.8,2.88925991435643,6.97529047046021));
#60026=CARTESIAN_POINT('Origin',(0.9,2.88925991435643,6.97529047046021));
#60027=CARTESIAN_POINT('',(0.9,2.88925991435643,7.62529047046021));
#60028=CARTESIAN_POINT('Origin',(0.,-3.24822445565046,5.85995203783395));
#60029=CARTESIAN_POINT('',(0.,-1.84677028397389,6.44045336278674));
#60030=CARTESIAN_POINT('',(0.,-3.24822445565046,5.85995203783395));
#60031=CARTESIAN_POINT('Origin',(0.,-3.8784769619707,6.99695765711517));
#60032=CARTESIAN_POINT('',(0.,-3.8784769619707,6.99695765711517));
#60033=CARTESIAN_POINT('Origin',(0.,-4.37985668768992,6.69453922202999));
#60034=CARTESIAN_POINT('',(0.,-4.37985668768992,6.69453922202999));
#60035=CARTESIAN_POINT('Origin',(0.,-4.85777416858265,6.3562591299483));
#60036=CARTESIAN_POINT('',(0.,-4.85777416858265,6.3562591299483));
#60037=CARTESIAN_POINT('Origin',(0.,-5.30966927135158,5.98392949731736));
#60038=CARTESIAN_POINT('',(0.,-5.30966927135158,5.98392949731736));
#60039=CARTESIAN_POINT('Origin',(0.,-5.73312126073229,5.57954483893977));
#60040=CARTESIAN_POINT('',(0.,-5.73312126073229,5.57954483893977));
#60041=CARTESIAN_POINT('Origin',(0.,-6.12586176701418,5.14527138365256));
#60042=CARTESIAN_POINT('',(0.,-6.12586176701418,5.14527138365256));
#60043=CARTESIAN_POINT('Origin',(0.,-6.4857869373617,4.68343547015952));
#60044=CARTESIAN_POINT('',(0.,-6.4857869373617,4.68343547015952));
#60045=CARTESIAN_POINT('Origin',(0.,-6.81096870584301,4.19651108517864));
#60046=CARTESIAN_POINT('',(0.,-6.81096870584301,4.19651108517864));
#60047=CARTESIAN_POINT('Origin',(0.,-7.09966512179413,3.68710661066098));
#60048=CARTESIAN_POINT('',(0.,-7.09966512179413,3.68710661066098));
#60049=CARTESIAN_POINT('Origin',(0.,-7.35032968119119,3.15795085107414));
#60050=CARTESIAN_POINT('',(0.,-7.35032968119119,3.15795085107414));
#60051=CARTESIAN_POINT('Origin',(0.,-7.5616196110438,2.61187841560012));
#60052=CARTESIAN_POINT('',(0.,-7.5616196110438,2.61187841560012));
#60053=CARTESIAN_POINT('Origin',(0.,-7.73240306243155,2.05181453355296));
#60054=CARTESIAN_POINT('',(0.,-7.73240306243155,2.05181453355296));
#60055=CARTESIAN_POINT('Origin',(0.,-7.86176517365131,1.48075938435772));
#60056=CARTESIAN_POINT('',(0.,-7.86176517365131,1.48075938435772));
#60057=CARTESIAN_POINT('Origin',(0.,-7.94901297099613,0.901772026032757));
#60058=CARTESIAN_POINT('',(0.,-7.94901297099613,0.901772026032757));
#60059=CARTESIAN_POINT('Origin',(0.,-7.99367908091301,0.317954008268197));
#60060=CARTESIAN_POINT('',(0.,-7.99367908091301,0.317954008268197));
#60061=CARTESIAN_POINT('Origin',(0.,-7.99552423365383,-0.267567242117311));
#60062=CARTESIAN_POINT('',(0.,-7.99552423365383,-0.267567242117311));
#60063=CARTESIAN_POINT('Origin',(0.,-7.95453854500815,-0.85165517433975));
#60064=CARTESIAN_POINT('',(0.,-7.95453854500815,-0.85165517433975));
#60065=CARTESIAN_POINT('Origin',(0.,-7.87094156925134,-1.43118091568862));
#60066=CARTESIAN_POINT('',(0.,-7.87094156925134,-1.43118091568862));
#60067=CARTESIAN_POINT('Origin',(0.,-7.74518112302486,-2.00304003243553));
#60068=CARTESIAN_POINT('',(0.,-7.74518112302486,-2.00304003243553));
#60069=CARTESIAN_POINT('Origin',(0.,-7.5779308864487,-2.56416915982678));
#60070=CARTESIAN_POINT('',(0.,-7.5779308864487,-2.56416915982678));
#60071=CARTESIAN_POINT('Origin',(0.,-7.37008679431654,-3.11156241207547));
#60072=CARTESIAN_POINT('',(0.,-7.37008679431654,-3.11156241207547));
#60073=CARTESIAN_POINT('Origin',(0.,-7.12276223670551,-3.64228748444736));
#60074=CARTESIAN_POINT('',(0.,-7.12276223670551,-3.64228748444736));
#60075=CARTESIAN_POINT('Origin',(0.,-6.83728209471014,-4.15350136118385));
#60076=CARTESIAN_POINT('',(0.,-6.83728209471014,-4.15350136118385));
#60077=CARTESIAN_POINT('Origin',(0.,-6.51517564325019,-4.64246554511711));
#60078=CARTESIAN_POINT('',(0.,-6.51517564325019,-4.64246554511711));
#60079=CARTESIAN_POINT('Origin',(0.,-6.15816835897094,-5.10656072739463));
#60080=CARTESIAN_POINT('',(0.,-6.15816835897094,-5.10656072739463));
#60081=CARTESIAN_POINT('Origin',(0.,-5.76817267711992,-5.54330081872951));
#60082=CARTESIAN_POINT('',(0.,-5.76817267711992,-5.54330081872951));
#60083=CARTESIAN_POINT('Origin',(0.,-5.34727774691394,-5.95034626701329));
#60084=CARTESIAN_POINT('',(0.,-5.34727774691394,-5.95034626701329));
#60085=CARTESIAN_POINT('Origin',(0.,-4.89773824027559,-6.32551658995075));
#60086=CARTESIAN_POINT('',(0.,-4.89773824027559,-6.32551658995075));
#60087=CARTESIAN_POINT('Origin',(0.,-4.42196227388907,-6.66680205558121));
#60088=CARTESIAN_POINT('',(0.,-4.42196227388907,-6.66680205558121));
#60089=CARTESIAN_POINT('Origin',(0.,-3.922498509275,-6.9723744481156));
#60090=CARTESIAN_POINT('',(0.,-3.922498509275,-6.9723744481156));
#60091=CARTESIAN_POINT('Origin',(0.,-3.40202249998754,-7.24059686141816));
#60092=CARTESIAN_POINT('',(0.,-3.40202249998754,-7.24059686141816));
#60093=CARTESIAN_POINT('Origin',(0.,-2.86332235906941,-7.47003246767062));
#60094=CARTESIAN_POINT('',(0.,-2.86332235906941,-7.47003246767062));
#60095=CARTESIAN_POINT('Origin',(0.,-2.30928382354251,-7.65945221424645));
#60096=CARTESIAN_POINT('',(0.,-2.30928382354251,-7.65945221424645));
#60097=CARTESIAN_POINT('Origin',(0.,-1.74287479594128,-7.80784140756411));
#60098=CARTESIAN_POINT('',(0.,-1.74287479594128,-7.80784140756411));
#60099=CARTESIAN_POINT('Origin',(0.,-1.16712944569752,-7.91440514865052));
#60100=CARTESIAN_POINT('',(0.,-1.16712944569752,-7.91440514865052));
#60101=CARTESIAN_POINT('Origin',(0.,-0.585131955543311,-7.9785725912974));
#60102=CARTESIAN_POINT('',(0.,-0.585131955543311,-7.9785725912974));
#60103=CARTESIAN_POINT('Origin',(0.,-1.46957615897682E-15,-8.));
#60104=CARTESIAN_POINT('',(0.,-1.46957615897682E-15,-8.));
#60105=CARTESIAN_POINT('Origin',(0.,0.585131955543308,-7.9785725912974));
#60106=CARTESIAN_POINT('',(0.,0.585131955543308,-7.9785725912974));
#60107=CARTESIAN_POINT('Origin',(0.,1.16712944569752,-7.91440514865052));
#60108=CARTESIAN_POINT('',(0.,1.16712944569752,-7.91440514865052));
#60109=CARTESIAN_POINT('Origin',(0.,1.74287479594128,-7.80784140756411));
#60110=CARTESIAN_POINT('',(0.,1.74287479594128,-7.80784140756411));
#60111=CARTESIAN_POINT('Origin',(0.,2.30928382354251,-7.65945221424645));
#60112=CARTESIAN_POINT('',(0.,2.30928382354251,-7.65945221424645));
#60113=CARTESIAN_POINT('Origin',(0.,2.86332235906941,-7.47003246767062));
#60114=CARTESIAN_POINT('',(0.,2.86332235906941,-7.47003246767062));
#60115=CARTESIAN_POINT('Origin',(0.,3.40202249998754,-7.24059686141816));
#60116=CARTESIAN_POINT('',(0.,3.40202249998754,-7.24059686141816));
#60117=CARTESIAN_POINT('Origin',(0.,3.922498509275,-6.97237444811561));
#60118=CARTESIAN_POINT('',(0.,3.922498509275,-6.97237444811561));
#60119=CARTESIAN_POINT('Origin',(0.,4.42196227388906,-6.66680205558121));
#60120=CARTESIAN_POINT('',(0.,4.42196227388906,-6.66680205558121));
#60121=CARTESIAN_POINT('Origin',(0.,4.89773824027559,-6.32551658995075));
#60122=CARTESIAN_POINT('',(0.,4.89773824027559,-6.32551658995075));
#60123=CARTESIAN_POINT('Origin',(0.,5.34727774691393,-5.95034626701329));
#60124=CARTESIAN_POINT('',(0.,5.34727774691393,-5.95034626701329));
#60125=CARTESIAN_POINT('Origin',(0.,5.76817267711992,-5.54330081872951));
#60126=CARTESIAN_POINT('',(0.,5.76817267711992,-5.54330081872951));
#60127=CARTESIAN_POINT('Origin',(0.,6.15816835897094,-5.10656072739463));
#60128=CARTESIAN_POINT('',(0.,6.15816835897094,-5.10656072739463));
#60129=CARTESIAN_POINT('Origin',(0.,6.51517564325019,-4.64246554511711));
#60130=CARTESIAN_POINT('',(0.,6.51517564325019,-4.64246554511711));
#60131=CARTESIAN_POINT('Origin',(0.,6.83728209471014,-4.15350136118385));
#60132=CARTESIAN_POINT('',(0.,6.83728209471014,-4.15350136118385));
#60133=CARTESIAN_POINT('Origin',(0.,7.12276223670551,-3.64228748444737));
#60134=CARTESIAN_POINT('',(0.,7.12276223670551,-3.64228748444737));
#60135=CARTESIAN_POINT('Origin',(0.,7.37008679431654,-3.11156241207547));
#60136=CARTESIAN_POINT('',(0.,7.37008679431654,-3.11156241207547));
#60137=CARTESIAN_POINT('Origin',(0.,7.5779308864487,-2.56416915982678));
#60138=CARTESIAN_POINT('',(0.,7.5779308864487,-2.56416915982678));
#60139=CARTESIAN_POINT('Origin',(0.,7.74518112302486,-2.00304003243554));
#60140=CARTESIAN_POINT('',(0.,7.74518112302486,-2.00304003243554));
#60141=CARTESIAN_POINT('Origin',(0.,7.87094156925134,-1.43118091568862));
#60142=CARTESIAN_POINT('',(0.,7.87094156925134,-1.43118091568862));
#60143=CARTESIAN_POINT('Origin',(0.,7.95453854500815,-0.851655174339752));
#60144=CARTESIAN_POINT('',(0.,7.95453854500815,-0.851655174339752));
#60145=CARTESIAN_POINT('Origin',(0.,7.99552423365383,-0.267567242117314));
#60146=CARTESIAN_POINT('',(0.,7.99552423365383,-0.267567242117314));
#60147=CARTESIAN_POINT('Origin',(0.,7.99367908091301,0.317954008268194));
#60148=CARTESIAN_POINT('',(0.,7.99367908091301,0.317954008268194));
#60149=CARTESIAN_POINT('Origin',(0.,7.94901297099613,0.901772026032747));
#60150=CARTESIAN_POINT('',(0.,7.94901297099613,0.901772026032747));
#60151=CARTESIAN_POINT('Origin',(0.,7.86176517365131,1.48075938435771));
#60152=CARTESIAN_POINT('',(0.,7.86176517365131,1.48075938435771));
#60153=CARTESIAN_POINT('Origin',(0.,7.73240306243155,2.05181453355297));
#60154=CARTESIAN_POINT('',(0.,7.73240306243155,2.05181453355297));
#60155=CARTESIAN_POINT('Origin',(0.,7.5616196110438,2.61187841560012));
#60156=CARTESIAN_POINT('',(0.,7.5616196110438,2.61187841560012));
#60157=CARTESIAN_POINT('Origin',(0.,7.35032968119119,3.15795085107413));
#60158=CARTESIAN_POINT('',(0.,7.35032968119119,3.15795085107413));
#60159=CARTESIAN_POINT('Origin',(0.,7.09966512179414,3.68710661066097));
#60160=CARTESIAN_POINT('',(0.,7.09966512179414,3.68710661066097));
#60161=CARTESIAN_POINT('Origin',(0.,6.81096870584301,4.19651108517863));
#60162=CARTESIAN_POINT('',(0.,6.81096870584301,4.19651108517863));
#60163=CARTESIAN_POINT('Origin',(0.,6.4857869373617,4.68343547015952));
#60164=CARTESIAN_POINT('',(0.,6.4857869373617,4.68343547015952));
#60165=CARTESIAN_POINT('Origin',(0.,6.12586176701418,5.14527138365256));
#60166=CARTESIAN_POINT('',(0.,6.12586176701418,5.14527138365256));
#60167=CARTESIAN_POINT('Origin',(0.,5.73312126073229,5.57954483893976));
#60168=CARTESIAN_POINT('',(0.,5.73312126073229,5.57954483893976));
#60169=CARTESIAN_POINT('Origin',(0.,5.30966927135158,5.98392949731736));
#60170=CARTESIAN_POINT('',(0.,5.30966927135158,5.98392949731736));
#60171=CARTESIAN_POINT('Origin',(0.,4.85777416858264,6.35625912994831));
#60172=CARTESIAN_POINT('',(0.,4.85777416858264,6.35625912994831));
#60173=CARTESIAN_POINT('Origin',(0.,4.37985668768992,6.69453922202999));
#60174=CARTESIAN_POINT('',(0.,4.37985668768992,6.69453922202999));
#60175=CARTESIAN_POINT('Origin',(0.,3.8784769619707,6.99695765711516));
#60176=CARTESIAN_POINT('',(0.,3.8784769619707,6.99695765711516));
#60177=CARTESIAN_POINT('Origin',(0.,3.24822445565046,5.85995203783395));
#60178=CARTESIAN_POINT('',(0.,3.24822445565046,5.85995203783395));
#60179=CARTESIAN_POINT('Origin',(0.,1.8467702839739,6.44045336278674));
#60180=CARTESIAN_POINT('',(0.,1.8467702839739,6.44045336278674));
#60181=CARTESIAN_POINT('Origin',(0.,2.60477301247065,9.08392302661711));
#60182=CARTESIAN_POINT('',(0.,2.60477301247065,9.08392302661711));
#60183=CARTESIAN_POINT('Origin',(0.,3.31804090301786,8.84833908515606));
#60184=CARTESIAN_POINT('',(0.,3.31804090301786,8.84833908515606));
#60185=CARTESIAN_POINT('Origin',(0.,4.0103440110564,8.5568476037022));
#60186=CARTESIAN_POINT('',(0.,4.0103440110564,8.5568476037022));
#60187=CARTESIAN_POINT('Origin',(0.,4.67730807342487,8.21129034843334));
#60188=CARTESIAN_POINT('',(0.,4.67730807342487,8.21129034843334));
#60189=CARTESIAN_POINT('Origin',(0.,5.31471892974448,7.81385069589992));
#60190=CARTESIAN_POINT('',(0.,5.31471892974448,7.81385069589992));
#60191=CARTESIAN_POINT('Origin',(0.,5.91854914926258,7.36703983753062));
#60192=CARTESIAN_POINT('',(0.,5.91854914926258,7.36703983753062));
#60193=CARTESIAN_POINT('Origin',(0.,6.48498347785954,6.87368091286531));
#60194=CARTESIAN_POINT('',(0.,6.48498347785954,6.87368091286531));
#60195=CARTESIAN_POINT('Origin',(0.,7.01044294443415,6.33689117176818));
#60196=CARTESIAN_POINT('',(0.,7.01044294443415,6.33689117176818));
#60197=CARTESIAN_POINT('Origin',(0.,7.49160747435326,5.76006227832775));
#60198=CARTESIAN_POINT('',(0.,7.49160747435326,5.76006227832775));
#60199=CARTESIAN_POINT('Origin',(0.,7.92543686708426,5.146838880892));
#60200=CARTESIAN_POINT('',(0.,7.92543686708426,5.146838880892));
#60201=CARTESIAN_POINT('Origin',(0.,8.30919000546483,4.5010955836422));
#60202=CARTESIAN_POINT('',(0.,8.30919000546483,4.5010955836422));
#60203=CARTESIAN_POINT('Origin',(0.,8.6404421752379,3.82691246520876));
#60204=CARTESIAN_POINT('',(0.,8.6404421752379,3.82691246520876));
#60205=CARTESIAN_POINT('Origin',(0.,8.91710038541937,3.12854929901285));
#60206=CARTESIAN_POINT('',(0.,8.91710038541937,3.12854929901285));
#60207=CARTESIAN_POINT('Origin',(0.,9.13741659269838,2.41041863822041));
#60208=CARTESIAN_POINT('',(0.,9.13741659269838,2.41041863822041));
#60209=CARTESIAN_POINT('Origin',(0.,9.29999874631253,1.67705793536937));
#60210=CARTESIAN_POINT('',(0.,9.29999874631253,1.67705793536937));
#60211=CARTESIAN_POINT('Origin',(0.,9.40381958361198,0.933100872829846));
#60212=CARTESIAN_POINT('',(0.,9.40381958361198,0.933100872829846));
#60213=CARTESIAN_POINT('Origin',(0.,9.44822312073834,0.183248085243736));
#60214=CARTESIAN_POINT('',(0.,9.44822312073834,0.183248085243736));
#60215=CARTESIAN_POINT('Origin',(0.,9.43292879740749,-0.567762541068464));
#60216=CARTESIAN_POINT('',(0.,9.43292879740749,-0.567762541068464));
#60217=CARTESIAN_POINT('Origin',(0.,9.35803324960784,-1.31518580407262));
#60218=CARTESIAN_POINT('',(0.,9.35803324960784,-1.31518580407262));
#60219=CARTESIAN_POINT('Origin',(0.,9.22400969901338,-2.05429916820971));
#60220=CARTESIAN_POINT('',(0.,9.22400969901338,-2.05429916820971));
#60221=CARTESIAN_POINT('Origin',(0.,9.03170496296946,-2.7804326033682));
#60222=CARTESIAN_POINT('',(0.,9.03170496296946,-2.7804326033682));
#60223=CARTESIAN_POINT('Origin',(0.,8.78233410394347,-3.48899809210487));
#60224=CARTESIAN_POINT('',(0.,8.78233410394347,-3.48899809210487));
#60225=CARTESIAN_POINT('Origin',(0.,8.47747275224749,-4.17551861867497));
#60226=CARTESIAN_POINT('',(0.,8.47747275224749,-4.17551861867497));
#60227=CARTESIAN_POINT('Origin',(0.,8.11904715054109,-4.83565645670685));
#60228=CARTESIAN_POINT('',(0.,8.11904715054109,-4.83565645670685));
#60229=CARTESIAN_POINT('Origin',(0.,7.70932198301742,-5.46524057678747));
#60230=CARTESIAN_POINT('',(0.,7.70932198301742,-5.46524057678747));
#60231=CARTESIAN_POINT('Origin',(0.,7.25088606617289,-6.06029300078633));
#60232=CARTESIAN_POINT('',(0.,7.25088606617289,-6.06029300078633));
#60233=CARTESIAN_POINT('Origin',(0.,6.74663599157214,-6.61705393639975));
#60234=CARTESIAN_POINT('',(0.,6.74663599157214,-6.61705393639975));
#60235=CARTESIAN_POINT('Origin',(0.,6.19975782396029,-7.1320055331052));
#60236=CARTESIAN_POINT('',(0.,6.19975782396029,-7.1320055331052));
#60237=CARTESIAN_POINT('Origin',(0.,5.61370697036149,-7.60189410942528));
#60238=CARTESIAN_POINT('',(0.,5.61370697036149,-7.60189410942528));
#60239=CARTESIAN_POINT('Origin',(0.,4.99218634735931,-8.02375071106021));
#60240=CARTESIAN_POINT('',(0.,4.99218634735931,-8.02375071106021));
#60241=CARTESIAN_POINT('Origin',(0.,4.33912298450726,-8.39490986999389));
#60242=CARTESIAN_POINT('',(0.,4.33912298450726,-8.39490986999389));
#60243=CARTESIAN_POINT('Origin',(0.,3.658643211699,-8.71302644604553));
#60244=CARTESIAN_POINT('',(0.,3.658643211699,-8.71302644604553));
#60245=CARTESIAN_POINT('Origin',(0.,2.95504658727499,-8.97609044445489));
#60246=CARTESIAN_POINT('',(0.,2.95504658727499,-8.97609044445489));
#60247=CARTESIAN_POINT('Origin',(0.,2.23277873159856,-9.18243971587732));
#60248=CARTESIAN_POINT('',(0.,2.23277873159856,-9.18243971587732));
#60249=CARTESIAN_POINT('Origin',(0.,1.49640323775065,-9.33077045854464));
#60250=CARTESIAN_POINT('',(0.,1.49640323775065,-9.33077045854464));
#60251=CARTESIAN_POINT('Origin',(0.,0.750572836823028,-9.42014545623492));
#60252=CARTESIAN_POINT('',(0.,0.750572836823028,-9.42014545623492));
#60253=CARTESIAN_POINT('Origin',(0.,-1.73593683779137E-15,-9.45));
#60254=CARTESIAN_POINT('',(0.,-1.73593683779137E-15,-9.45));
#60255=CARTESIAN_POINT('Origin',(0.,-0.750572836823032,-9.42014545623492));
#60256=CARTESIAN_POINT('',(0.,-0.750572836823032,-9.42014545623492));
#60257=CARTESIAN_POINT('Origin',(0.,-1.49640323775065,-9.33077045854464));
#60258=CARTESIAN_POINT('',(0.,-1.49640323775065,-9.33077045854464));
#60259=CARTESIAN_POINT('Origin',(0.,-2.23277873159856,-9.18243971587732));
#60260=CARTESIAN_POINT('',(0.,-2.23277873159856,-9.18243971587732));
#60261=CARTESIAN_POINT('Origin',(0.,-2.95504658727499,-8.97609044445489));
#60262=CARTESIAN_POINT('',(0.,-2.95504658727499,-8.97609044445489));
#60263=CARTESIAN_POINT('Origin',(0.,-3.65864321169901,-8.71302644604553));
#60264=CARTESIAN_POINT('',(0.,-3.65864321169901,-8.71302644604553));
#60265=CARTESIAN_POINT('Origin',(0.,-4.33912298450726,-8.39490986999389));
#60266=CARTESIAN_POINT('',(0.,-4.33912298450726,-8.39490986999389));
#60267=CARTESIAN_POINT('Origin',(0.,-4.99218634735932,-8.02375071106021));
#60268=CARTESIAN_POINT('',(0.,-4.99218634735932,-8.02375071106021));
#60269=CARTESIAN_POINT('Origin',(0.,-5.6137069703615,-7.60189410942528));
#60270=CARTESIAN_POINT('',(0.,-5.6137069703615,-7.60189410942528));
#60271=CARTESIAN_POINT('Origin',(0.,-6.1997578239603,-7.13200553310519));
#60272=CARTESIAN_POINT('',(0.,-6.1997578239603,-7.13200553310519));
#60273=CARTESIAN_POINT('Origin',(0.,-6.74663599157215,-6.61705393639974));
#60274=CARTESIAN_POINT('',(0.,-6.74663599157215,-6.61705393639974));
#60275=CARTESIAN_POINT('Origin',(0.,-7.2508860661729,-6.06029300078632));
#60276=CARTESIAN_POINT('',(0.,-7.2508860661729,-6.06029300078632));
#60277=CARTESIAN_POINT('Origin',(0.,-7.70932198301743,-5.46524057678747));
#60278=CARTESIAN_POINT('',(0.,-7.70932198301743,-5.46524057678747));
#60279=CARTESIAN_POINT('Origin',(0.,-8.11904715054109,-4.83565645670684));
#60280=CARTESIAN_POINT('',(0.,-8.11904715054109,-4.83565645670684));
#60281=CARTESIAN_POINT('Origin',(0.,-8.47747275224749,-4.17551861867497));
#60282=CARTESIAN_POINT('',(0.,-8.47747275224749,-4.17551861867497));
#60283=CARTESIAN_POINT('Origin',(0.,-8.78233410394347,-3.48899809210486));
#60284=CARTESIAN_POINT('',(0.,-8.78233410394347,-3.48899809210486));
#60285=CARTESIAN_POINT('Origin',(0.,-9.03170496296946,-2.7804326033682));
#60286=CARTESIAN_POINT('',(0.,-9.03170496296946,-2.7804326033682));
#60287=CARTESIAN_POINT('Origin',(0.,-9.22400969901338,-2.0542991682097));
#60288=CARTESIAN_POINT('',(0.,-9.22400969901338,-2.0542991682097));
#60289=CARTESIAN_POINT('Origin',(0.,-9.35803324960784,-1.31518580407261));
#60290=CARTESIAN_POINT('',(0.,-9.35803324960784,-1.31518580407261));
#60291=CARTESIAN_POINT('Origin',(0.,-9.43292879740749,-0.567762541068457));
#60292=CARTESIAN_POINT('',(0.,-9.43292879740749,-0.567762541068457));
#60293=CARTESIAN_POINT('Origin',(0.,-9.44822312073834,0.183248085243744));
#60294=CARTESIAN_POINT('',(0.,-9.44822312073834,0.183248085243744));
#60295=CARTESIAN_POINT('Origin',(0.,-9.40381958361198,0.933100872829854));
#60296=CARTESIAN_POINT('',(0.,-9.40381958361198,0.933100872829854));
#60297=CARTESIAN_POINT('Origin',(0.,-9.29999874631253,1.67705793536938));
#60298=CARTESIAN_POINT('',(0.,-9.29999874631253,1.67705793536938));
#60299=CARTESIAN_POINT('Origin',(0.,-9.13741659269838,2.41041863822042));
#60300=CARTESIAN_POINT('',(0.,-9.13741659269838,2.41041863822042));
#60301=CARTESIAN_POINT('Origin',(0.,-8.91710038541936,3.12854929901286));
#60302=CARTESIAN_POINT('',(0.,-8.91710038541936,3.12854929901286));
#60303=CARTESIAN_POINT('Origin',(0.,-8.64044217523789,3.82691246520877));
#60304=CARTESIAN_POINT('',(0.,-8.64044217523789,3.82691246520877));
#60305=CARTESIAN_POINT('Origin',(0.,-8.30919000546483,4.5010955836422));
#60306=CARTESIAN_POINT('',(0.,-8.30919000546483,4.5010955836422));
#60307=CARTESIAN_POINT('Origin',(0.,-7.92543686708426,5.14683888089201));
#60308=CARTESIAN_POINT('',(0.,-7.92543686708426,5.14683888089201));
#60309=CARTESIAN_POINT('Origin',(0.,-7.49160747435326,5.76006227832776));
#60310=CARTESIAN_POINT('',(0.,-7.49160747435326,5.76006227832776));
#60311=CARTESIAN_POINT('Origin',(0.,-7.01044294443414,6.33689117176819));
#60312=CARTESIAN_POINT('',(0.,-7.01044294443414,6.33689117176819));
#60313=CARTESIAN_POINT('Origin',(0.,-6.48498347785953,6.87368091286531));
#60314=CARTESIAN_POINT('',(0.,-6.48498347785953,6.87368091286531));
#60315=CARTESIAN_POINT('Origin',(0.,-5.91854914926258,7.36703983753062));
#60316=CARTESIAN_POINT('',(0.,-5.91854914926258,7.36703983753062));
#60317=CARTESIAN_POINT('Origin',(0.,-5.31471892974448,7.81385069589992));
#60318=CARTESIAN_POINT('',(0.,-5.31471892974448,7.81385069589992));
#60319=CARTESIAN_POINT('Origin',(0.,-4.67730807342486,8.21129034843335));
#60320=CARTESIAN_POINT('',(0.,-4.67730807342486,8.21129034843335));
#60321=CARTESIAN_POINT('Origin',(0.,-4.01034401105639,8.5568476037022));
#60322=CARTESIAN_POINT('',(0.,-4.01034401105639,8.5568476037022));
#60323=CARTESIAN_POINT('Origin',(0.,-3.31804090301785,8.84833908515606));
#60324=CARTESIAN_POINT('',(0.,-3.31804090301785,8.84833908515606));
#60325=CARTESIAN_POINT('Origin',(0.,-2.60477301247064,9.08392302661711));
#60326=CARTESIAN_POINT('',(0.,-2.60477301247064,9.08392302661711));
#60327=CARTESIAN_POINT('Origin',(0.,-1.84677028397389,6.44045336278674));
#60328=CARTESIAN_POINT('',(0.,0.,0.));
#60329=CARTESIAN_POINT('',(48.075,0.,0.));
#60330=CARTESIAN_POINT('',(114.,0.,0.));
#60331=CARTESIAN_POINT('',(117.55,0.,0.));
#60332=CARTESIAN_POINT('',(117.5,0.,0.));
#60333=CARTESIAN_POINT('',(127.075,0.,0.));
#60334=CARTESIAN_POINT('',(133.,0.,0.));
#60335=CARTESIAN_POINT('',(164.,0.,0.));
#60336=CARTESIAN_POINT('',(61.,0.,0.));
#60337=CARTESIAN_POINT('',(100.,0.,0.));
#60338=CARTESIAN_POINT('',(59.5,0.,0.));
#60339=CARTESIAN_POINT('',(72.,0.,0.));
#60340=CARTESIAN_POINT('',(98.5,0.,0.));
#60341=CARTESIAN_POINT('',(111.,0.,0.));
#60342=UNCERTAINTY_MEASURE_WITH_UNIT(LENGTH_MEASURE(0.01),#60366,
'DISTANCE_ACCURACY_VALUE',
'Maximum model space distance between geometric entities at asserted c
onnectivities');
#60343=UNCERTAINTY_MEASURE_WITH_UNIT(LENGTH_MEASURE(0.01),#60366,
'DISTANCE_ACCURACY_VALUE',
'Maximum model space distance between geometric entities at asserted c
onnectivities');
#60344=UNCERTAINTY_MEASURE_WITH_UNIT(LENGTH_MEASURE(0.01),#60366,
'DISTANCE_ACCURACY_VALUE',
'Maximum model space distance between geometric entities at asserted c
onnectivities');
#60345=UNCERTAINTY_MEASURE_WITH_UNIT(LENGTH_MEASURE(0.01),#60366,
'DISTANCE_ACCURACY_VALUE',
'Maximum model space distance between geometric entities at asserted c
onnectivities');
#60346=UNCERTAINTY_MEASURE_WITH_UNIT(LENGTH_MEASURE(0.01),#60366,
'DISTANCE_ACCURACY_VALUE',
'Maximum model space distance between geometric entities at asserted c
onnectivities');
#60347=UNCERTAINTY_MEASURE_WITH_UNIT(LENGTH_MEASURE(0.01),#60366,
'DISTANCE_ACCURACY_VALUE',
'Maximum model space distance between geometric entities at asserted c
onnectivities');
#60348=UNCERTAINTY_MEASURE_WITH_UNIT(LENGTH_MEASURE(0.01),#60366,
'DISTANCE_ACCURACY_VALUE',
'Maximum model space distance between geometric entities at asserted c
onnectivities');
#60349=UNCERTAINTY_MEASURE_WITH_UNIT(LENGTH_MEASURE(0.01),#60366,
'DISTANCE_ACCURACY_VALUE',
'Maximum model space distance between geometric entities at asserted c
onnectivities');
#60350=UNCERTAINTY_MEASURE_WITH_UNIT(LENGTH_MEASURE(0.01),#60366,
'DISTANCE_ACCURACY_VALUE',
'Maximum model space distance between geometric entities at asserted c
onnectivities');
#60351=UNCERTAINTY_MEASURE_WITH_UNIT(LENGTH_MEASURE(0.01),#60366,
'DISTANCE_ACCURACY_VALUE',
'Maximum model space distance between geometric entities at asserted c
onnectivities');
#60352=UNCERTAINTY_MEASURE_WITH_UNIT(LENGTH_MEASURE(0.01),#60366,
'DISTANCE_ACCURACY_VALUE',
'Maximum model space distance between geometric entities at asserted c
onnectivities');
#60353=UNCERTAINTY_MEASURE_WITH_UNIT(LENGTH_MEASURE(0.01),#60366,
'DISTANCE_ACCURACY_VALUE',
'Maximum model space distance between geometric entities at asserted c
onnectivities');
#60354=(
GEOMETRIC_REPRESENTATION_CONTEXT(3)
GLOBAL_UNCERTAINTY_ASSIGNED_CONTEXT((#60342))
GLOBAL_UNIT_ASSIGNED_CONTEXT((#60366,#60368,#60369))
REPRESENTATION_CONTEXT('','3D')
);
#60355=(
GEOMETRIC_REPRESENTATION_CONTEXT(3)
GLOBAL_UNCERTAINTY_ASSIGNED_CONTEXT((#60343))
GLOBAL_UNIT_ASSIGNED_CONTEXT((#60366,#60368,#60369))
REPRESENTATION_CONTEXT('','3D')
);
#60356=(
GEOMETRIC_REPRESENTATION_CONTEXT(3)
GLOBAL_UNCERTAINTY_ASSIGNED_CONTEXT((#60344))
GLOBAL_UNIT_ASSIGNED_CONTEXT((#60366,#60368,#60369))
REPRESENTATION_CONTEXT('','3D')
);
#60357=(
GEOMETRIC_REPRESENTATION_CONTEXT(3)
GLOBAL_UNCERTAINTY_ASSIGNED_CONTEXT((#60345))
GLOBAL_UNIT_ASSIGNED_CONTEXT((#60366,#60368,#60369))
REPRESENTATION_CONTEXT('','3D')
);
#60358=(
GEOMETRIC_REPRESENTATION_CONTEXT(3)
GLOBAL_UNCERTAINTY_ASSIGNED_CONTEXT((#60346))
GLOBAL_UNIT_ASSIGNED_CONTEXT((#60366,#60368,#60369))
REPRESENTATION_CONTEXT('','3D')
);
#60359=(
GEOMETRIC_REPRESENTATION_CONTEXT(3)
GLOBAL_UNCERTAINTY_ASSIGNED_CONTEXT((#60347))
GLOBAL_UNIT_ASSIGNED_CONTEXT((#60366,#60368,#60369))
REPRESENTATION_CONTEXT('','3D')
);
#60360=(
GEOMETRIC_REPRESENTATION_CONTEXT(3)
GLOBAL_UNCERTAINTY_ASSIGNED_CONTEXT((#60348))
GLOBAL_UNIT_ASSIGNED_CONTEXT((#60366,#60368,#60369))
REPRESENTATION_CONTEXT('','3D')
);
#60361=(
GEOMETRIC_REPRESENTATION_CONTEXT(3)
GLOBAL_UNCERTAINTY_ASSIGNED_CONTEXT((#60349))
GLOBAL_UNIT_ASSIGNED_CONTEXT((#60366,#60368,#60369))
REPRESENTATION_CONTEXT('','3D')
);
#60362=(
GEOMETRIC_REPRESENTATION_CONTEXT(3)
GLOBAL_UNCERTAINTY_ASSIGNED_CONTEXT((#60350))
GLOBAL_UNIT_ASSIGNED_CONTEXT((#60366,#60368,#60369))
REPRESENTATION_CONTEXT('','3D')
);
#60363=(
GEOMETRIC_REPRESENTATION_CONTEXT(3)
GLOBAL_UNCERTAINTY_ASSIGNED_CONTEXT((#60351))
GLOBAL_UNIT_ASSIGNED_CONTEXT((#60366,#60368,#60369))
REPRESENTATION_CONTEXT('','3D')
);
#60364=(
GEOMETRIC_REPRESENTATION_CONTEXT(3)
GLOBAL_UNCERTAINTY_ASSIGNED_CONTEXT((#60352))
GLOBAL_UNIT_ASSIGNED_CONTEXT((#60366,#60368,#60369))
REPRESENTATION_CONTEXT('','3D')
);
#60365=(
GEOMETRIC_REPRESENTATION_CONTEXT(3)
GLOBAL_UNCERTAINTY_ASSIGNED_CONTEXT((#60353))
GLOBAL_UNIT_ASSIGNED_CONTEXT((#60366,#60368,#60369))
REPRESENTATION_CONTEXT('','3D')
);
#60366=(
LENGTH_UNIT()
NAMED_UNIT(*)
SI_UNIT(.MILLI.,.METRE.)
);
#60367=(
LENGTH_UNIT()
NAMED_UNIT(*)
SI_UNIT($,.METRE.)
);
#60368=(
NAMED_UNIT(*)
PLANE_ANGLE_UNIT()
SI_UNIT($,.RADIAN.)
);
#60369=(
NAMED_UNIT(*)
SI_UNIT($,.STERADIAN.)
SOLID_ANGLE_UNIT()
);
#60370=SHAPE_DEFINITION_REPRESENTATION(#60381,#60406);
#60371=SHAPE_DEFINITION_REPRESENTATION(#60382,#60407);
#60372=SHAPE_DEFINITION_REPRESENTATION(#60383,#60408);
#60373=SHAPE_DEFINITION_REPRESENTATION(#60384,#60409);
#60374=SHAPE_DEFINITION_REPRESENTATION(#60385,#60410);
#60375=SHAPE_DEFINITION_REPRESENTATION(#60386,#60411);
#60376=SHAPE_DEFINITION_REPRESENTATION(#60387,#60412);
#60377=SHAPE_DEFINITION_REPRESENTATION(#60388,#60413);
#60378=SHAPE_DEFINITION_REPRESENTATION(#60389,#60414);
#60379=SHAPE_DEFINITION_REPRESENTATION(#60390,#60415);
#60380=SHAPE_DEFINITION_REPRESENTATION(#60391,#60416);
#60381=PRODUCT_DEFINITION_SHAPE('',$,#60418);
#60382=PRODUCT_DEFINITION_SHAPE('',$,#60419);
#60383=PRODUCT_DEFINITION_SHAPE('',$,#60420);
#60384=PRODUCT_DEFINITION_SHAPE('',$,#60421);
#60385=PRODUCT_DEFINITION_SHAPE('',$,#60422);
#60386=PRODUCT_DEFINITION_SHAPE('',$,#60423);
#60387=PRODUCT_DEFINITION_SHAPE('',$,#60424);
#60388=PRODUCT_DEFINITION_SHAPE('',$,#60425);
#60389=PRODUCT_DEFINITION_SHAPE('',$,#60426);
#60390=PRODUCT_DEFINITION_SHAPE('',$,#60427);
#60391=PRODUCT_DEFINITION_SHAPE('',$,#60428);
#60392=PRODUCT_DEFINITION_SHAPE($,$,#53);
#60393=PRODUCT_DEFINITION_SHAPE($,$,#54);
#60394=PRODUCT_DEFINITION_SHAPE($,$,#55);
#60395=PRODUCT_DEFINITION_SHAPE($,$,#56);
#60396=PRODUCT_DEFINITION_SHAPE($,$,#57);
#60397=PRODUCT_DEFINITION_SHAPE($,$,#58);
#60398=PRODUCT_DEFINITION_SHAPE($,$,#59);
#60399=PRODUCT_DEFINITION_SHAPE($,$,#60);
#60400=PRODUCT_DEFINITION_SHAPE($,$,#61);
#60401=PRODUCT_DEFINITION_SHAPE($,$,#62);
#60402=PRODUCT_DEFINITION_SHAPE($,$,#63);
#60403=PRODUCT_DEFINITION_SHAPE($,$,#64);
#60404=PRODUCT_DEFINITION_SHAPE($,$,#65);
#60405=PRODUCT_DEFINITION_SHAPE($,$,#66);
#60406=SHAPE_REPRESENTATION('',(#18418,#19664,#19665,#19666,#19667,#19668,
#19669,#19670,#19671,#19672,#19673,#19674,#19675,#19676,#19677),#60354);
#60407=SHAPE_REPRESENTATION('',(#18419),#60355);
#60408=SHAPE_REPRESENTATION('',(#18916),#60356);
#60409=SHAPE_REPRESENTATION('',(#18921),#60357);
#60410=SHAPE_REPRESENTATION('',(#18938),#60358);
#60411=SHAPE_REPRESENTATION('',(#19163),#60359);
#60412=SHAPE_REPRESENTATION('',(#19226),#60360);
#60413=SHAPE_REPRESENTATION('',(#19231),#60361);
#60414=SHAPE_REPRESENTATION('',(#19368),#60362);
#60415=SHAPE_REPRESENTATION('',(#19440),#60363);
#60416=SHAPE_REPRESENTATION('',(#19497),#60364);
#60417=PRODUCT_DEFINITION_CONTEXT('part definition',#60452,'design');
#60418=PRODUCT_DEFINITION('2026-10-25-00-06-13-923','MAS-496',#60429,#60417);
#60419=PRODUCT_DEFINITION('2026-10-25-00-06-14-899',
'01_Turbine_Wheel_and_Shaft_HX35_60x70_12B',#60430,#60417);
#60420=PRODUCT_DEFINITION('2026-10-25-00-06-27-341',
'02_Piston_Ring_Turbine_D19',#60431,#60417);
#60421=PRODUCT_DEFINITION('2026-10-25-00-06-30-524','05_Thrust_Collar',
#60432,#60417);
#60422=PRODUCT_DEFINITION('2026-10-25-00-06-30-685','06_Thrust_Bearing',
#60433,#60417);
#60423=PRODUCT_DEFINITION('2026-10-25-00-06-35-053','07_Oil_Flinger',#60434,
#60417);
#60424=PRODUCT_DEFINITION('2026-10-25-00-06-35-685',
'08_Piston_Ring_Compressor_D16',#60435,#60417);
#60425=PRODUCT_DEFINITION('2026-10-25-00-06-36-701',
'09_Compressor_Wheel_54x78_7plus7',#60436,#60417);
#60426=PRODUCT_DEFINITION('2026-10-25-00-06-43-044',
'10_Compressor_Locknut_12pt_M7x1_LH',#60437,#60417);
#60427=PRODUCT_DEFINITION('2026-10-25-00-06-28-201',
'03_Journal_Bearing_D11',#60438,#60417);
#60428=PRODUCT_DEFINITION('2026-10-25-00-06-28-626',
'04_Journal_Retaining_Ring_D18',#60439,#60417);
#60429=PRODUCT_DEFINITION_FORMATION('',$,#60454);
#60430=PRODUCT_DEFINITION_FORMATION('',$,#60455);
#60431=PRODUCT_DEFINITION_FORMATION('',$,#60456);
#60432=PRODUCT_DEFINITION_FORMATION('',$,#60457);
#60433=PRODUCT_DEFINITION_FORMATION('',$,#60458);
#60434=PRODUCT_DEFINITION_FORMATION('',$,#60459);
#60435=PRODUCT_DEFINITION_FORMATION('',$,#60460);
#60436=PRODUCT_DEFINITION_FORMATION('',$,#60461);
#60437=PRODUCT_DEFINITION_FORMATION('',$,#60462);
#60438=PRODUCT_DEFINITION_FORMATION('',$,#60463);
#60439=PRODUCT_DEFINITION_FORMATION('',$,#60464);
#60440=PRODUCT_RELATED_PRODUCT_CATEGORY('MAS-496','MAS-496',(#60454));
#60441=PRODUCT_RELATED_PRODUCT_CATEGORY(
'01_Turbine_Wheel_and_Shaft_HX35_60x70_12B',
'01_Turbine_Wheel_and_Shaft_HX35_60x70_12B',(#60455));
#60442=PRODUCT_RELATED_PRODUCT_CATEGORY('02_Piston_Ring_Turbine_D19',
'02_Piston_Ring_Turbine_D19',(#60456));
#60443=PRODUCT_RELATED_PRODUCT_CATEGORY('05_Thrust_Collar',
'05_Thrust_Collar',(#60457));
#60444=PRODUCT_RELATED_PRODUCT_CATEGORY('06_Thrust_Bearing',
'06_Thrust_Bearing',(#60458));
#60445=PRODUCT_RELATED_PRODUCT_CATEGORY('07_Oil_Flinger',
'07_Oil_Flinger',(#60459));
#60446=PRODUCT_RELATED_PRODUCT_CATEGORY('08_Piston_Ring_Compressor_D16',
'08_Piston_Ring_Compressor_D16',(#60460));
#60447=PRODUCT_RELATED_PRODUCT_CATEGORY(
'09_Compressor_Wheel_54x78_7plus7','09_Compressor_Wheel_54x78_7plus7',(#60461));
#60448=PRODUCT_RELATED_PRODUCT_CATEGORY(
'10_Compressor_Locknut_12pt_M7x1_LH',
'10_Compressor_Locknut_12pt_M7x1_LH',(#60462));
#60449=PRODUCT_RELATED_PRODUCT_CATEGORY('03_Journal_Bearing_D11',
'03_Journal_Bearing_D11',(#60463));
#60450=PRODUCT_RELATED_PRODUCT_CATEGORY('04_Journal_Retaining_Ring_D18',
'04_Journal_Retaining_Ring_D18',(#60464));
#60451=APPLICATION_PROTOCOL_DEFINITION('international standard',
'automotive_design',2009,#60452);
#60452=APPLICATION_CONTEXT(
'Core Data for Automotive Mechanical Design Process');
#60453=PRODUCT_CONTEXT('part definition',#60452,'mechanical');
#60454=PRODUCT('2026-10-25-00-06-13-923','MAS-496',$,(#60453));
#60455=PRODUCT('2026-10-25-00-06-14-899',
'01_Turbine_Wheel_and_Shaft_HX35_60x70_12B',$,(#60453));
#60456=PRODUCT('2026-10-25-00-06-27-341','02_Piston_Ring_Turbine_D19',$,
(#60453));
#60457=PRODUCT('2026-10-25-00-06-30-524','05_Thrust_Collar',$,(#60453));
#60458=PRODUCT('2026-10-25-00-06-30-685','06_Thrust_Bearing',$,(#60453));
#60459=PRODUCT('2026-10-25-00-06-35-053','07_Oil_Flinger',$,(#60453));
#60460=PRODUCT('2026-10-25-00-06-35-685',
'08_Piston_Ring_Compressor_D16',$,(#60453));
#60461=PRODUCT('2026-10-25-00-06-36-701',
'09_Compressor_Wheel_54x78_7plus7',$,(#60453));
#60462=PRODUCT('2026-10-25-00-06-43-044',
'10_Compressor_Locknut_12pt_M7x1_LH',$,(#60453));
#60463=PRODUCT('2026-10-25-00-06-28-201','03_Journal_Bearing_D11',$,(#60453));
#60464=PRODUCT('2026-10-25-00-06-28-626',
'04_Journal_Retaining_Ring_D18',$,(#60453));
#60465=PRESENTATION_STYLE_ASSIGNMENT((#60470));
#60466=PRESENTATION_STYLE_ASSIGNMENT((#60471));
#60467=PRESENTATION_STYLE_ASSIGNMENT((#60472));
#60468=PRESENTATION_STYLE_ASSIGNMENT((#60473));
#60469=PRESENTATION_STYLE_ASSIGNMENT((#60474));
#60470=SURFACE_STYLE_USAGE(.BOTH.,#60475);
#60471=SURFACE_STYLE_USAGE(.BOTH.,#60476);
#60472=SURFACE_STYLE_USAGE(.BOTH.,#60477);
#60473=SURFACE_STYLE_USAGE(.BOTH.,#60478);
#60474=SURFACE_STYLE_USAGE(.BOTH.,#60479);
#60475=SURFACE_SIDE_STYLE('',(#60480));
#60476=SURFACE_SIDE_STYLE('',(#60481));
#60477=SURFACE_SIDE_STYLE('',(#60482));
#60478=SURFACE_SIDE_STYLE('',(#60483));
#60479=SURFACE_SIDE_STYLE('',(#60484));
#60480=SURFACE_STYLE_FILL_AREA(#60485);
#60481=SURFACE_STYLE_FILL_AREA(#60486);
#60482=SURFACE_STYLE_FILL_AREA(#60487);
#60483=SURFACE_STYLE_FILL_AREA(#60488);
#60484=SURFACE_STYLE_FILL_AREA(#60489);
#60485=FILL_AREA_STYLE('Steel - Satin',(#60490));
#60486=FILL_AREA_STYLE('MAS496_ss',(#60491));
#60487=FILL_AREA_STYLE('MAS496_ti',(#60492));
#60488=FILL_AREA_STYLE('MAS496_al',(#60493));
#60489=FILL_AREA_STYLE('MAS496_gun',(#60494));
#60490=FILL_AREA_STYLE_COLOUR('Steel - Satin',#60495);
#60491=FILL_AREA_STYLE_COLOUR('MAS496_ss',#60496);
#60492=FILL_AREA_STYLE_COLOUR('MAS496_ti',#60497);
#60493=FILL_AREA_STYLE_COLOUR('MAS496_al',#60498);
#60494=FILL_AREA_STYLE_COLOUR('MAS496_gun',#60499);
#60495=COLOUR_RGB('Steel - Satin',0.627450980392157,0.627450980392157,0.627450980392157);
#60496=COLOUR_RGB('MAS496_ss',0.83921568627451,0.850980392156863,0.862745098039216);
#60497=COLOUR_RGB('MAS496_ti',0.549019607843137,0.572549019607843,0.596078431372549);
#60498=COLOUR_RGB('MAS496_al',0.67843137254902,0.705882352941177,0.729411764705882);
#60499=COLOUR_RGB('MAS496_gun',0.313725490196078,0.337254901960784,0.364705882352941);
#60500=COLOUR_RGB('Dark Blue',0.08,0.2,0.34);
#60501=FILL_AREA_STYLE_COLOUR('',#60500);
#60502=FILL_AREA_STYLE('',(#60501));
#60503=SURFACE_STYLE_FILL_AREA(#60502);
#60504=SURFACE_SIDE_STYLE('',(#60503));
#60505=SURFACE_STYLE_USAGE(.BOTH.,#60504);
#60506=PRESENTATION_STYLE_ASSIGNMENT((#60505));
#60507=COLOUR_RGB('Light Blue',0.38,0.62,0.78);
#60508=FILL_AREA_STYLE_COLOUR('',#60507);
#60509=FILL_AREA_STYLE('',(#60508));
#60510=SURFACE_STYLE_FILL_AREA(#60509);
#60511=SURFACE_SIDE_STYLE('',(#60510));
#60512=SURFACE_STYLE_USAGE(.BOTH.,#60511);
#60513=PRESENTATION_STYLE_ASSIGNMENT((#60512));
#60514=COLOUR_RGB('Sky Blue',0.24,0.69,0.87);
#60515=FILL_AREA_STYLE_COLOUR('',#60514);
#60516=FILL_AREA_STYLE('',(#60515));
#60517=SURFACE_STYLE_FILL_AREA(#60516);
#60518=SURFACE_SIDE_STYLE('',(#60517));
#60519=SURFACE_STYLE_USAGE(.BOTH.,#60518);
#60520=PRESENTATION_STYLE_ASSIGNMENT((#60519));
#60521=COLOUR_RGB('Grey',0.48,0.52,0.57);
#60522=FILL_AREA_STYLE_COLOUR('',#60521);
#60523=FILL_AREA_STYLE('',(#60522));
#60524=SURFACE_STYLE_FILL_AREA(#60523);
#60525=SURFACE_SIDE_STYLE('',(#60524));
#60526=SURFACE_STYLE_USAGE(.BOTH.,#60525);
#60527=PRESENTATION_STYLE_ASSIGNMENT((#60526));
#60528=COLOUR_RGB('Black',0.12,0.14,0.17);
#60529=FILL_AREA_STYLE_COLOUR('',#60528);
#60530=FILL_AREA_STYLE('',(#60529));
#60531=SURFACE_STYLE_FILL_AREA(#60530);
#60532=SURFACE_SIDE_STYLE('',(#60531));
#60533=SURFACE_STYLE_USAGE(.BOTH.,#60532);
#60534=PRESENTATION_STYLE_ASSIGNMENT((#60533));
#60535=COLOUR_RGB('Off White',0.89,0.88,0.83);
#60536=FILL_AREA_STYLE_COLOUR('',#60535);
#60537=FILL_AREA_STYLE('',(#60536));
#60538=SURFACE_STYLE_FILL_AREA(#60537);
#60539=SURFACE_SIDE_STYLE('',(#60538));
#60540=SURFACE_STYLE_USAGE(.BOTH.,#60539);
#60541=PRESENTATION_STYLE_ASSIGNMENT((#60540));
ENDSEC;
END-ISO-10303-21;
